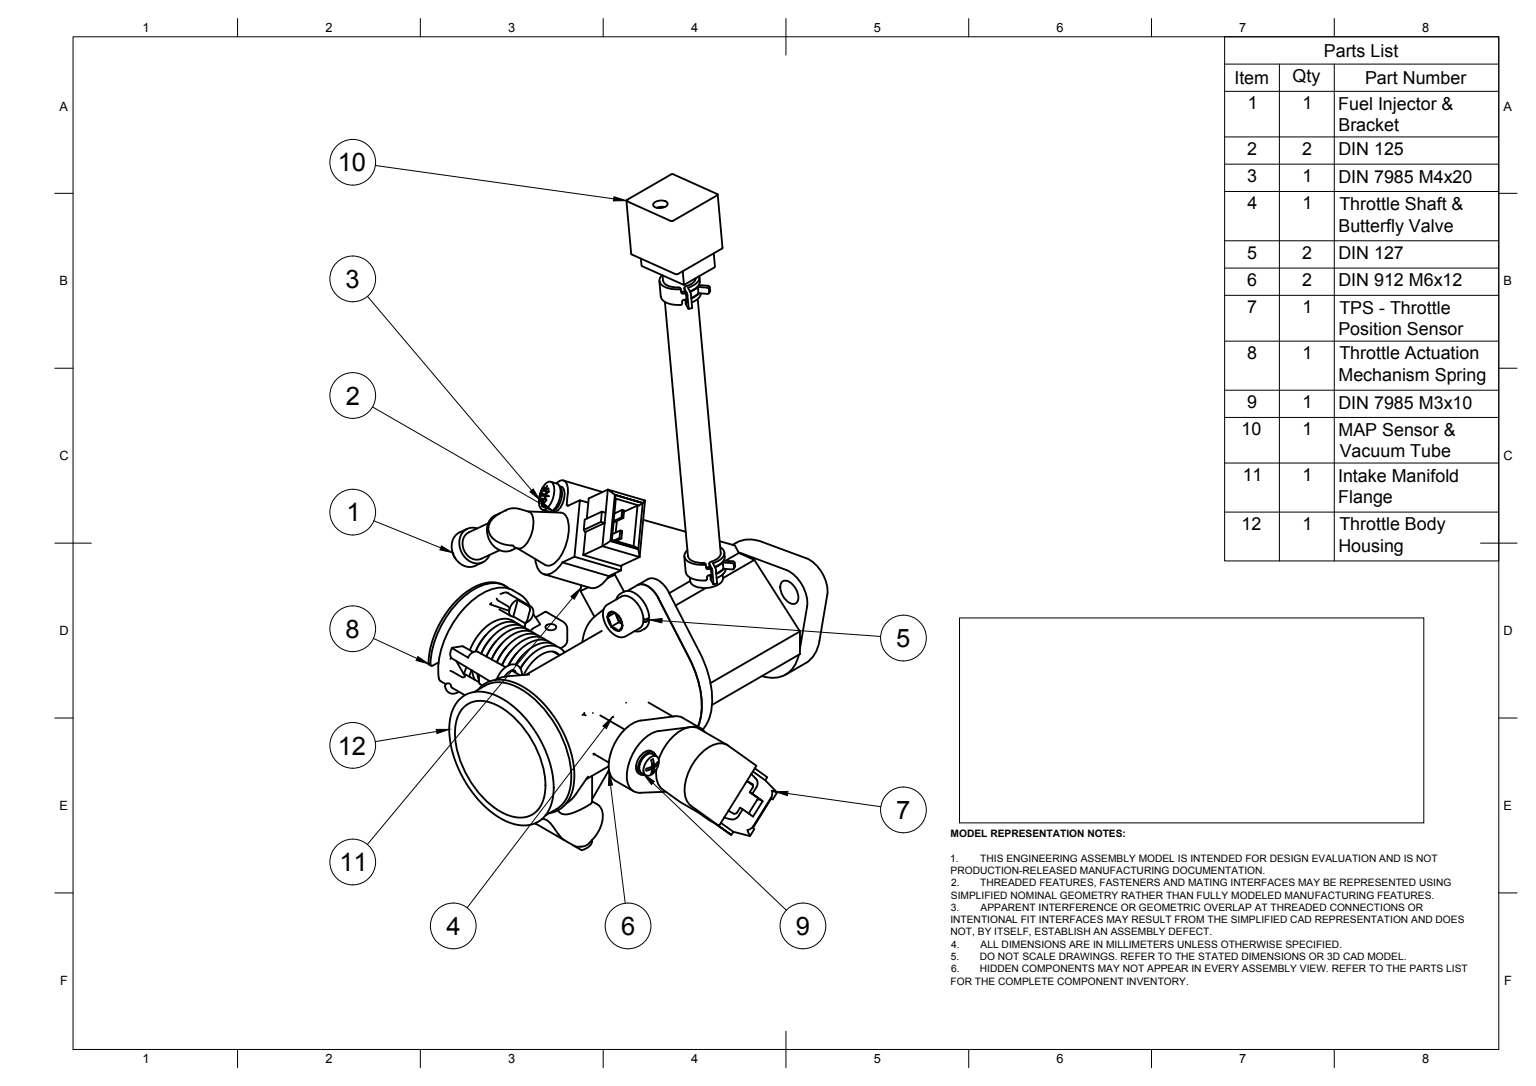
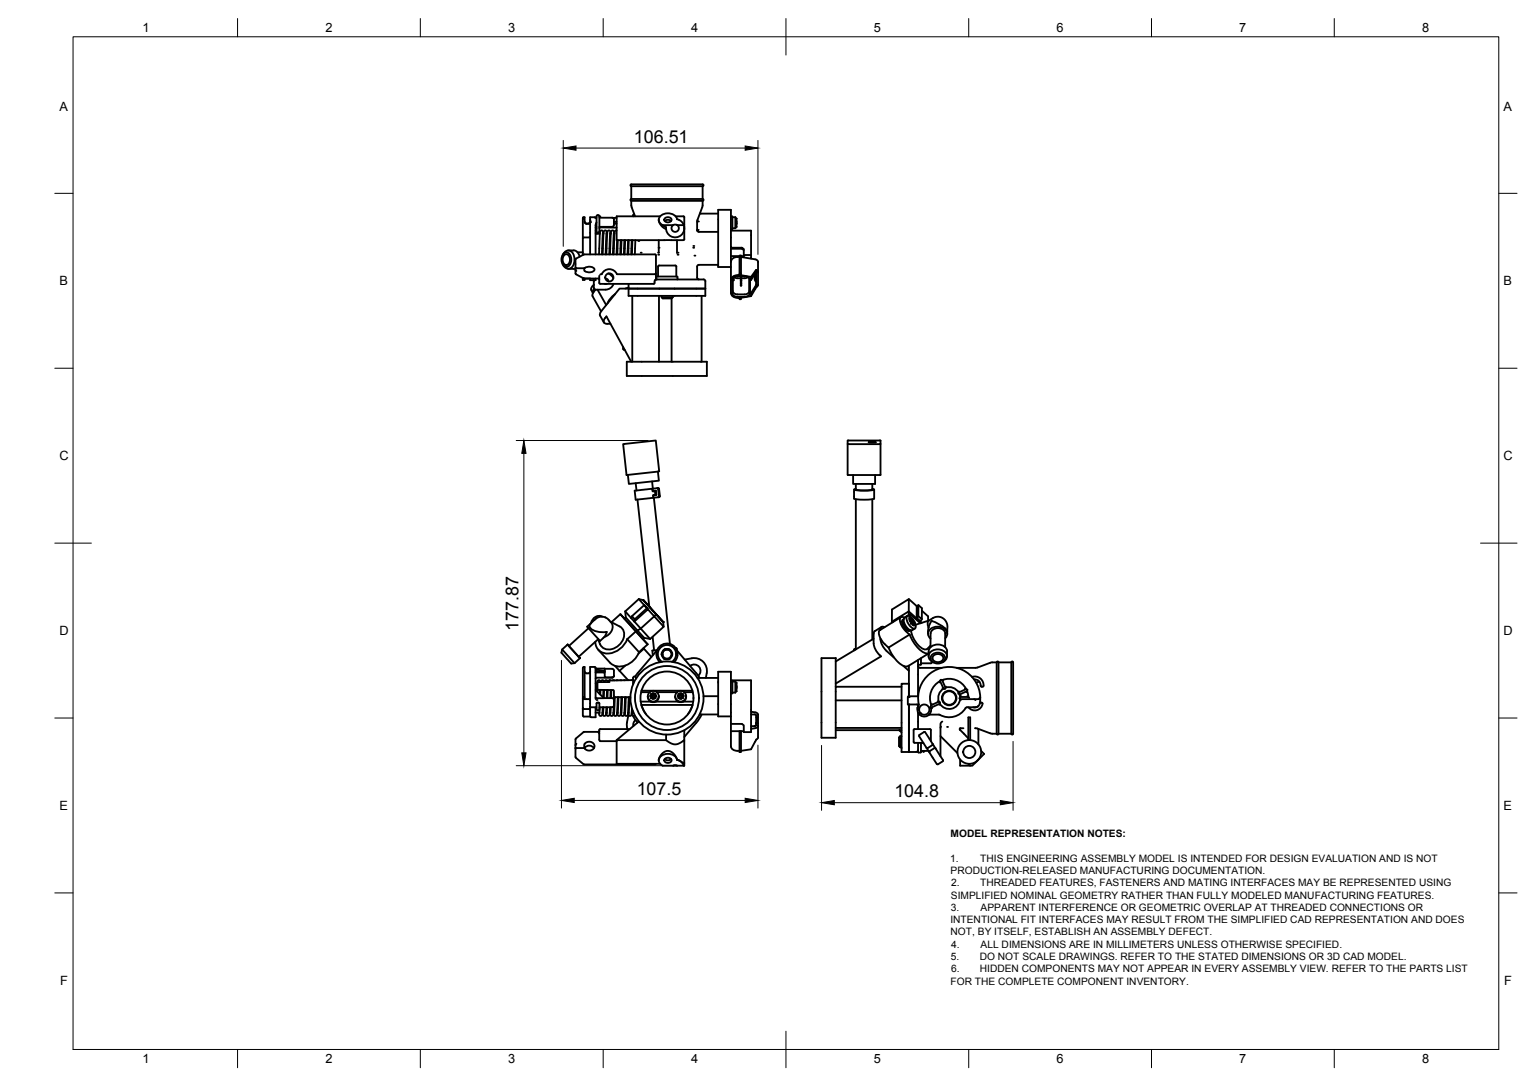
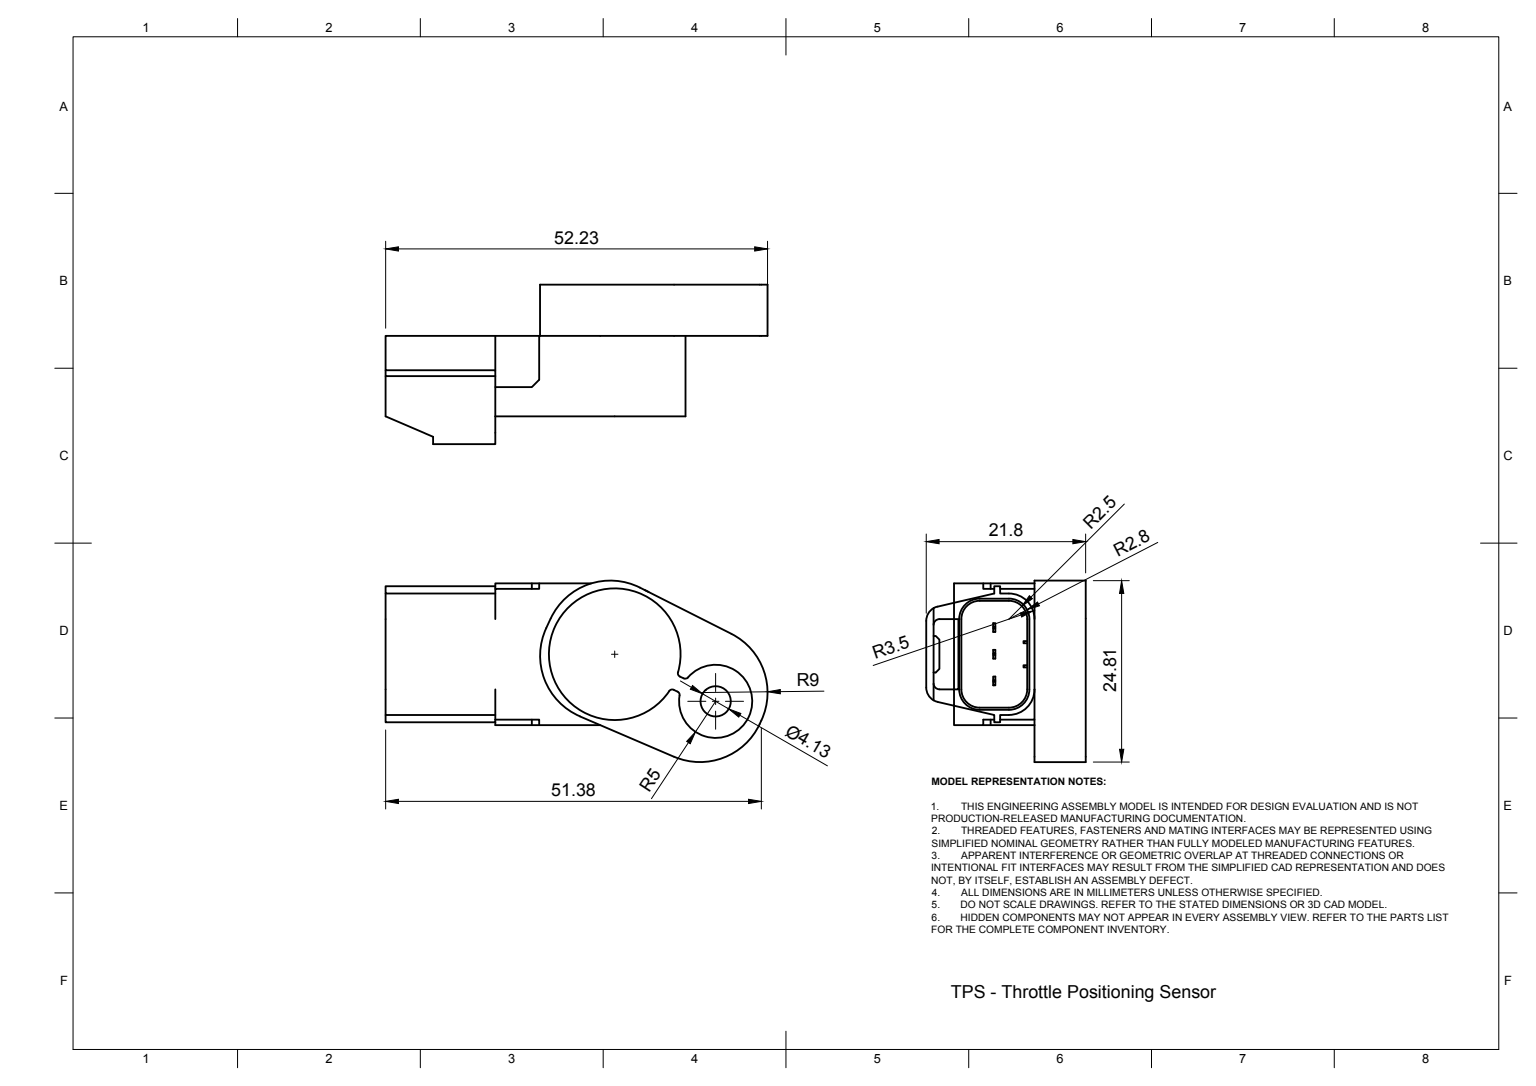
ISO-10303-21;
HEADER;
/* Generated by software containing ST-Developer
 * from STEP Tools, Inc. (www.steptools.com) 
 */

FILE_DESCRIPTION(
/* description */ ('STEP AP214'),
/* implementation_level */ '2;1');

FILE_NAME(
/* name */ 'MAS-617',
/* time_stamp */ '2026-10-07T12:18:07-07:00',
/* author */ (''),
/* organization */ (''),
/* preprocessor_version */ 'ST-DEVELOPER v20.2',
/* originating_system */ 'Autodesk Translation Framework v15.15.0.0',
/* authorisation */ '');

FILE_SCHEMA (('AUTOMOTIVE_DESIGN { 1 0 10303 214 3 1 1 }'));
ENDSEC;

DATA;
#10=MECHANICAL_DESIGN_GEOMETRIC_PRESENTATION_REPRESENTATION('',(#122,#123,
#124,#125,#126,#127,#128,#129,#130,#131,#132,#133),#62974);
#11=ITEM_DEFINED_TRANSFORMATION($,$,#15338,#16941);
#12=ITEM_DEFINED_TRANSFORMATION($,$,#16856,#16942);
#13=ITEM_DEFINED_TRANSFORMATION($,$,#15471,#16943);
#14=ITEM_DEFINED_TRANSFORMATION($,$,#15531,#16944);
#15=ITEM_DEFINED_TRANSFORMATION($,$,#16865,#16945);
#16=ITEM_DEFINED_TRANSFORMATION($,$,#16884,#16946);
#17=ITEM_DEFINED_TRANSFORMATION($,$,#15679,#16947);
#18=ITEM_DEFINED_TRANSFORMATION($,$,#15858,#16948);
#19=ITEM_DEFINED_TRANSFORMATION($,$,#16176,#16949);
#20=ITEM_DEFINED_TRANSFORMATION($,$,#16214,#16950);
#21=ITEM_DEFINED_TRANSFORMATION($,$,#16388,#16951);
#22=ITEM_DEFINED_TRANSFORMATION($,$,#16488,#16952);
#23=ITEM_DEFINED_TRANSFORMATION($,$,#16856,#16953);
#24=ITEM_DEFINED_TRANSFORMATION($,$,#16865,#16954);
#25=ITEM_DEFINED_TRANSFORMATION($,$,#16884,#16955);
#26=(
REPRESENTATION_RELATIONSHIP($,$,#63021,#63020)
REPRESENTATION_RELATIONSHIP_WITH_TRANSFORMATION(#11)
SHAPE_REPRESENTATION_RELATIONSHIP()
);
#27=(
REPRESENTATION_RELATIONSHIP($,$,#63030,#63020)
REPRESENTATION_RELATIONSHIP_WITH_TRANSFORMATION(#12)
SHAPE_REPRESENTATION_RELATIONSHIP()
);
#28=(
REPRESENTATION_RELATIONSHIP($,$,#63022,#63020)
REPRESENTATION_RELATIONSHIP_WITH_TRANSFORMATION(#13)
SHAPE_REPRESENTATION_RELATIONSHIP()
);
#29=(
REPRESENTATION_RELATIONSHIP($,$,#63023,#63020)
REPRESENTATION_RELATIONSHIP_WITH_TRANSFORMATION(#14)
SHAPE_REPRESENTATION_RELATIONSHIP()
);
#30=(
REPRESENTATION_RELATIONSHIP($,$,#63031,#63020)
REPRESENTATION_RELATIONSHIP_WITH_TRANSFORMATION(#15)
SHAPE_REPRESENTATION_RELATIONSHIP()
);
#31=(
REPRESENTATION_RELATIONSHIP($,$,#63032,#63020)
REPRESENTATION_RELATIONSHIP_WITH_TRANSFORMATION(#16)
SHAPE_REPRESENTATION_RELATIONSHIP()
);
#32=(
REPRESENTATION_RELATIONSHIP($,$,#63024,#63020)
REPRESENTATION_RELATIONSHIP_WITH_TRANSFORMATION(#17)
SHAPE_REPRESENTATION_RELATIONSHIP()
);
#33=(
REPRESENTATION_RELATIONSHIP($,$,#63025,#63020)
REPRESENTATION_RELATIONSHIP_WITH_TRANSFORMATION(#18)
SHAPE_REPRESENTATION_RELATIONSHIP()
);
#34=(
REPRESENTATION_RELATIONSHIP($,$,#63026,#63020)
REPRESENTATION_RELATIONSHIP_WITH_TRANSFORMATION(#19)
SHAPE_REPRESENTATION_RELATIONSHIP()
);
#35=(
REPRESENTATION_RELATIONSHIP($,$,#63027,#63020)
REPRESENTATION_RELATIONSHIP_WITH_TRANSFORMATION(#20)
SHAPE_REPRESENTATION_RELATIONSHIP()
);
#36=(
REPRESENTATION_RELATIONSHIP($,$,#63028,#63020)
REPRESENTATION_RELATIONSHIP_WITH_TRANSFORMATION(#21)
SHAPE_REPRESENTATION_RELATIONSHIP()
);
#37=(
REPRESENTATION_RELATIONSHIP($,$,#63029,#63020)
REPRESENTATION_RELATIONSHIP_WITH_TRANSFORMATION(#22)
SHAPE_REPRESENTATION_RELATIONSHIP()
);
#38=(
REPRESENTATION_RELATIONSHIP($,$,#63030,#63020)
REPRESENTATION_RELATIONSHIP_WITH_TRANSFORMATION(#23)
SHAPE_REPRESENTATION_RELATIONSHIP()
);
#39=(
REPRESENTATION_RELATIONSHIP($,$,#63031,#63020)
REPRESENTATION_RELATIONSHIP_WITH_TRANSFORMATION(#24)
SHAPE_REPRESENTATION_RELATIONSHIP()
);
#40=(
REPRESENTATION_RELATIONSHIP($,$,#63032,#63020)
REPRESENTATION_RELATIONSHIP_WITH_TRANSFORMATION(#25)
SHAPE_REPRESENTATION_RELATIONSHIP()
);
#41=CONTEXT_DEPENDENT_SHAPE_REPRESENTATION(#26,#63005);
#42=CONTEXT_DEPENDENT_SHAPE_REPRESENTATION(#27,#63006);
#43=CONTEXT_DEPENDENT_SHAPE_REPRESENTATION(#28,#63007);
#44=CONTEXT_DEPENDENT_SHAPE_REPRESENTATION(#29,#63008);
#45=CONTEXT_DEPENDENT_SHAPE_REPRESENTATION(#30,#63009);
#46=CONTEXT_DEPENDENT_SHAPE_REPRESENTATION(#31,#63010);
#47=CONTEXT_DEPENDENT_SHAPE_REPRESENTATION(#32,#63011);
#48=CONTEXT_DEPENDENT_SHAPE_REPRESENTATION(#33,#63012);
#49=CONTEXT_DEPENDENT_SHAPE_REPRESENTATION(#34,#63013);
#50=CONTEXT_DEPENDENT_SHAPE_REPRESENTATION(#35,#63014);
#51=CONTEXT_DEPENDENT_SHAPE_REPRESENTATION(#36,#63015);
#52=CONTEXT_DEPENDENT_SHAPE_REPRESENTATION(#37,#63016);
#53=CONTEXT_DEPENDENT_SHAPE_REPRESENTATION(#38,#63017);
#54=CONTEXT_DEPENDENT_SHAPE_REPRESENTATION(#39,#63018);
#55=CONTEXT_DEPENDENT_SHAPE_REPRESENTATION(#40,#63019);
#56=NEXT_ASSEMBLY_USAGE_OCCURRENCE('Fuel Injector & Bracket:1',
'Fuel Injector & Bracket:1','Fuel Injector & Bracket:1',#63034,#63035,
'Fuel Injector & Bracket:1');
#57=NEXT_ASSEMBLY_USAGE_OCCURRENCE('DIN 125:1','DIN 125:1','DIN 125:1',
#63034,#63044,'DIN 125:1');
#58=NEXT_ASSEMBLY_USAGE_OCCURRENCE('DIN 7985 M4x20:1',
'DIN 7985 M4x20:1','DIN 7985 M4x20:1',#63034,#63036,'DIN 7985 M4x20:1');
#59=NEXT_ASSEMBLY_USAGE_OCCURRENCE('Throttle Shaft & Butterfly Valve:1',
'Throttle Shaft & Butterfly Valve:1',
'Throttle Shaft & Butterfly Valve:1',#63034,#63037,
'Throttle Shaft & Butterfly Valve:1');
#60=NEXT_ASSEMBLY_USAGE_OCCURRENCE('DIN 127:1','DIN 127:1','DIN 127:1',
#63034,#63045,'DIN 127:1');
#61=NEXT_ASSEMBLY_USAGE_OCCURRENCE('DIN 912 M6x12:1','DIN 912 M6x12:1',
'DIN 912 M6x12:1',#63034,#63046,'DIN 912 M6x12:1');
#62=NEXT_ASSEMBLY_USAGE_OCCURRENCE('TPS - Throttle Position Sensor:1',
'TPS - Throttle Position Sensor:1','TPS - Throttle Position Sensor:1',#63034,
#63038,'TPS - Throttle Position Sensor:1');
#63=NEXT_ASSEMBLY_USAGE_OCCURRENCE(
'Throttle Actuation Mechanism Spring:1',
'Throttle Actuation Mechanism Spring:1',
'Throttle Actuation Mechanism Spring:1',#63034,#63039,
'Throttle Actuation Mechanism Spring:1');
#64=NEXT_ASSEMBLY_USAGE_OCCURRENCE('DIN 7985 M3x10:1',
'DIN 7985 M3x10:1','DIN 7985 M3x10:1',#63034,#63040,'DIN 7985 M3x10:1');
#65=NEXT_ASSEMBLY_USAGE_OCCURRENCE('MAP Sensor & Vacuum Tube:1',
'MAP Sensor & Vacuum Tube:1','MAP Sensor & Vacuum Tube:1',#63034,#63041,
'MAP Sensor & Vacuum Tube:1');
#66=NEXT_ASSEMBLY_USAGE_OCCURRENCE('Intake Manifold Flange:1',
'Intake Manifold Flange:1','Intake Manifold Flange:1',#63034,#63042,
'Intake Manifold Flange:1');
#67=NEXT_ASSEMBLY_USAGE_OCCURRENCE('Throttle Body Housing:1',
'Throttle Body Housing:1','Throttle Body Housing:1',#63034,#63043,
'Throttle Body Housing:1');
#68=NEXT_ASSEMBLY_USAGE_OCCURRENCE('DIN 125:2','DIN 125:2','DIN 125:2',
#63034,#63044,'DIN 125:2');
#69=NEXT_ASSEMBLY_USAGE_OCCURRENCE('DIN 127:2','DIN 127:2','DIN 127:2',
#63034,#63045,'DIN 127:2');
#70=NEXT_ASSEMBLY_USAGE_OCCURRENCE('DIN 912 M6x12:2','DIN 912 M6x12:2',
'DIN 912 M6x12:2',#63034,#63046,'DIN 912 M6x12:2');
#71=(
BOUNDED_CURVE()
B_SPLINE_CURVE(2,(#37611,#37612,#37613,#37614,#37615,#37616,#37617,#37618,
#37619,#37620,#37621,#37622,#37623,#37624,#37625,#37626,#37627,#37628,#37629,
#37630,#37631,#37632,#37633,#37634,#37635,#37636,#37637,#37638,#37639,#37640,
#37641,#37642,#37643,#37644,#37645,#37646,#37647,#37648,#37649,#37650,#37651,
#37652,#37653,#37654,#37655,#37656,#37657,#37658,#37659,#37660,#37661,#37662,
#37663,#37664,#37665,#37666,#37667,#37668,#37669,#37670,#37671,#37672,#37673,
#37674,#37675,#37676,#37677,#37678,#37679,#37680,#37681,#37682,#37683,#37684,
#37685,#37686,#37687,#37688,#37689,#37690,#37691,#37692,#37693,#37694,#37695,
#37696,#37697,#37698,#37699,#37700,#37701,#37702,#37703,#37704,#37705,#37706,
#37707,#37708,#37709,#37710,#37711,#37712,#37713,#37714,#37715,#37716,#37717,
#37718,#37719,#37720,#37721,#37722,#37723,#37724,#37725,#37726,#37727,#37728,
#37729,#37730,#37731),.UNSPECIFIED.,.F.,.F.)
B_SPLINE_CURVE_WITH_KNOTS((3,2,2,2,2,2,2,2,2,2,2,2,2,2,2,2,2,2,2,2,2,2,
2,2,2,2,2,2,2,2,2,2,2,2,2,2,2,2,2,2,2,2,2,2,2,2,2,2,2,2,2,2,2,2,2,2,2,2,
2,2,3),(0.,0.0166666666666666,0.0333333333333333,0.05,0.0666666666666667,
0.0833333333333333,0.1,0.116666666666667,0.133333333333333,0.15,0.166666666666667,
0.183333333333334,0.2,0.216666666666667,0.233333333333334,0.25,0.266666666666667,
0.283333333333334,0.3,0.316666666666666,0.333333333333334,0.35,0.366666666666666,
0.383333333333334,0.4,0.416666666666667,0.433333333333334,0.45,0.466666666666667,
0.483333333333333,0.5,0.516666666666667,0.533333333333333,0.55,0.566666666666667,
0.583333333333333,0.6,0.616666666666667,0.633333333333333,0.65,0.666666666666667,
0.683333333333333,0.7,0.716666666666667,0.733333333333333,0.75,0.766666666666667,
0.783333333333333,0.8,0.816666666666667,0.833333333333333,0.85,0.866666666666667,
0.883333333333333,0.9,0.916666666666667,0.933333333333333,0.95,0.966666666666667,
0.983333333333333,1.),.UNSPECIFIED.)
CURVE()
GEOMETRIC_REPRESENTATION_ITEM()
RATIONAL_B_SPLINE_CURVE((1.,0.866025403784439,1.,0.866025403784439,1.,0.866025403784439,
1.,0.866025403784439,1.,0.866025403784439,1.,0.866025403784439,1.,0.866025403784439,
1.,0.866025403784439,1.,0.866025403784439,1.,0.866025403784439,1.,0.866025403784439,
1.,0.866025403784439,1.,0.866025403784439,1.,0.866025403784439,1.,0.866025403784439,
1.,0.866025403784439,1.,0.866025403784439,1.,0.866025403784439,1.,0.866025403784439,
1.,0.866025403784439,1.,0.866025403784439,1.,0.866025403784439,1.,0.866025403784439,
1.,0.866025403784439,1.,0.866025403784439,1.,0.866025403784439,1.,0.866025403784439,
1.,0.866025403784439,1.,0.866025403784439,1.,0.866025403784439,1.,0.866025403784439,
1.,0.866025403784439,1.,0.866025403784439,1.,0.866025403784439,1.,0.866025403784439,
1.,0.866025403784439,1.,0.866025403784439,1.,0.866025403784439,1.,0.866025403784439,
1.,0.866025403784439,1.,0.866025403784439,1.,0.866025403784439,1.,0.866025403784439,
1.,0.866025403784439,1.,0.866025403784439,1.,0.866025403784439,1.,0.866025403784439,
1.,0.866025403784439,1.,0.866025403784439,1.,0.866025403784439,1.,0.866025403784439,
1.,0.866025403784439,1.,0.866025403784439,1.,0.866025403784439,1.,0.866025403784439,
1.,0.866025403784439,1.,0.866025403784439,1.,0.866025403784439,1.,0.866025403784439,
1.,0.866025403784439,1.))
REPRESENTATION_ITEM('')
);
#72=(
BOUNDED_CURVE()
B_SPLINE_CURVE(2,(#37732,#37733,#37734,#37735,#37736,#37737,#37738,#37739,
#37740,#37741,#37742,#37743,#37744,#37745,#37746,#37747,#37748,#37749,#37750,
#37751,#37752,#37753,#37754,#37755,#37756,#37757,#37758,#37759,#37760,#37761,
#37762,#37763,#37764,#37765,#37766,#37767,#37768,#37769,#37770,#37771,#37772,
#37773,#37774,#37775,#37776,#37777,#37778,#37779,#37780,#37781,#37782,#37783,
#37784,#37785,#37786,#37787,#37788,#37789,#37790,#37791,#37792,#37793,#37794,
#37795,#37796,#37797,#37798,#37799,#37800,#37801,#37802,#37803,#37804,#37805,
#37806,#37807,#37808,#37809,#37810,#37811,#37812,#37813,#37814,#37815,#37816,
#37817,#37818,#37819,#37820,#37821,#37822,#37823,#37824,#37825,#37826,#37827,
#37828,#37829,#37830,#37831,#37832,#37833,#37834,#37835,#37836,#37837,#37838,
#37839,#37840,#37841,#37842,#37843,#37844,#37845,#37846,#37847,#37848,#37849,
#37850,#37851,#37852),.UNSPECIFIED.,.F.,.F.)
B_SPLINE_CURVE_WITH_KNOTS((3,2,2,2,2,2,2,2,2,2,2,2,2,2,2,2,2,2,2,2,2,2,
2,2,2,2,2,2,2,2,2,2,2,2,2,2,2,2,2,2,2,2,2,2,2,2,2,2,2,2,2,2,2,2,2,2,2,2,
2,2,3),(0.,0.0166666666666666,0.0333333333333333,0.05,0.0666666666666667,
0.0833333333333333,0.1,0.116666666666667,0.133333333333333,0.15,0.166666666666667,
0.183333333333334,0.2,0.216666666666667,0.233333333333334,0.25,0.266666666666667,
0.283333333333334,0.3,0.316666666666666,0.333333333333334,0.35,0.366666666666666,
0.383333333333334,0.4,0.416666666666667,0.433333333333334,0.45,0.466666666666667,
0.483333333333333,0.5,0.516666666666667,0.533333333333333,0.55,0.566666666666667,
0.583333333333333,0.6,0.616666666666667,0.633333333333333,0.65,0.666666666666667,
0.683333333333333,0.7,0.716666666666667,0.733333333333333,0.75,0.766666666666667,
0.783333333333333,0.8,0.816666666666667,0.833333333333333,0.85,0.866666666666667,
0.883333333333333,0.9,0.916666666666667,0.933333333333333,0.95,0.966666666666667,
0.983333333333333,1.),.UNSPECIFIED.)
CURVE()
GEOMETRIC_REPRESENTATION_ITEM()
RATIONAL_B_SPLINE_CURVE((1.,0.866025403784439,1.,0.866025403784439,1.,0.866025403784439,
1.,0.866025403784439,1.,0.866025403784439,1.,0.866025403784439,1.,0.866025403784439,
1.,0.866025403784439,1.,0.866025403784439,1.,0.866025403784439,1.,0.866025403784439,
1.,0.866025403784439,1.,0.866025403784439,1.,0.866025403784439,1.,0.866025403784439,
1.,0.866025403784439,1.,0.866025403784439,1.,0.866025403784439,1.,0.866025403784439,
1.,0.866025403784439,1.,0.866025403784439,1.,0.866025403784439,1.,0.866025403784439,
1.,0.866025403784439,1.,0.866025403784439,1.,0.866025403784439,1.,0.866025403784439,
1.,0.866025403784439,1.,0.866025403784439,1.,0.866025403784439,1.,0.866025403784439,
1.,0.866025403784439,1.,0.866025403784439,1.,0.866025403784439,1.,0.866025403784439,
1.,0.866025403784439,1.,0.866025403784439,1.,0.866025403784439,1.,0.866025403784439,
1.,0.866025403784439,1.,0.866025403784439,1.,0.866025403784439,1.,0.866025403784439,
1.,0.866025403784439,1.,0.866025403784439,1.,0.866025403784439,1.,0.866025403784439,
1.,0.866025403784439,1.,0.866025403784439,1.,0.866025403784439,1.,0.866025403784439,
1.,0.866025403784439,1.,0.866025403784439,1.,0.866025403784439,1.,0.866025403784439,
1.,0.866025403784439,1.,0.866025403784439,1.,0.866025403784439,1.,0.866025403784439,
1.,0.866025403784439,1.))
REPRESENTATION_ITEM('')
);
#73=(
BOUNDED_CURVE()
B_SPLINE_CURVE(2,(#62798,#62799,#62800),.UNSPECIFIED.,.F.,.F.)
B_SPLINE_CURVE_WITH_KNOTS((3,3),(-0.604448710450841,-0.208150383555822),
 .UNSPECIFIED.)
CURVE()
GEOMETRIC_REPRESENTATION_ITEM()
RATIONAL_B_SPLINE_CURVE((1.32194252928783,1.52287779373958,1.32194252928783))
REPRESENTATION_ITEM('')
);
#74=(
BOUNDED_CURVE()
B_SPLINE_CURVE(2,(#62844,#62845,#62846),.UNSPECIFIED.,.F.,.F.)
B_SPLINE_CURVE_WITH_KNOTS((3,3),(0.208150383555825,0.60444871045084),
 .UNSPECIFIED.)
CURVE()
GEOMETRIC_REPRESENTATION_ITEM()
RATIONAL_B_SPLINE_CURVE((1.32194252928783,1.52287779373957,1.32194252928783))
REPRESENTATION_ITEM('')
);
#75=(
BOUNDED_CURVE()
B_SPLINE_CURVE(2,(#62851,#62852,#62853),.UNSPECIFIED.,.F.,.F.)
B_SPLINE_CURVE_WITH_KNOTS((3,3),(0.208150383555826,0.604448710450838),
 .UNSPECIFIED.)
CURVE()
GEOMETRIC_REPRESENTATION_ITEM()
RATIONAL_B_SPLINE_CURVE((1.32194252928783,1.52287779373957,1.32194252928783))
REPRESENTATION_ITEM('')
);
#76=(
BOUNDED_CURVE()
B_SPLINE_CURVE(2,(#62858,#62859,#62860),.UNSPECIFIED.,.F.,.F.)
B_SPLINE_CURVE_WITH_KNOTS((3,3),(0.208150383555825,0.60444871045084),
 .UNSPECIFIED.)
CURVE()
GEOMETRIC_REPRESENTATION_ITEM()
RATIONAL_B_SPLINE_CURVE((1.32194252928783,1.52287779373957,1.32194252928783))
REPRESENTATION_ITEM('')
);
#77=(
BOUNDED_CURVE()
B_SPLINE_CURVE(2,(#62869,#62870,#62871),.UNSPECIFIED.,.F.,.F.)
B_SPLINE_CURVE_WITH_KNOTS((3,3),(0.208150383555823,0.604448710450839),
 .UNSPECIFIED.)
CURVE()
GEOMETRIC_REPRESENTATION_ITEM()
RATIONAL_B_SPLINE_CURVE((1.32194252928783,1.52287779373958,1.32194252928783))
REPRESENTATION_ITEM('')
);
#78=(
BOUNDED_CURVE()
B_SPLINE_CURVE(2,(#62876,#62877,#62878),.UNSPECIFIED.,.F.,.F.)
B_SPLINE_CURVE_WITH_KNOTS((3,3),(0.208150383555823,0.604448710450836),
 .UNSPECIFIED.)
CURVE()
GEOMETRIC_REPRESENTATION_ITEM()
RATIONAL_B_SPLINE_CURVE((1.32194252928783,1.52287779373958,1.32194252928783))
REPRESENTATION_ITEM('')
);
#79=SPHERICAL_SURFACE('',#15475,8.00000000000091);
#80=SPHERICAL_SURFACE('',#15545,6.);
#81=SPHERICAL_SURFACE('',#15579,6.);
#82=SPHERICAL_SURFACE('',#16177,6.);
#83=SPHERICAL_SURFACE('',#16593,0.5);
#84=SPHERICAL_SURFACE('',#16603,0.5);
#85=SPHERICAL_SURFACE('',#16608,0.5);
#86=SPHERICAL_SURFACE('',#16674,0.5);
#87=SPHERICAL_SURFACE('',#16680,0.5);
#88=SPHERICAL_SURFACE('',#16687,0.5);
#89=SPHERICAL_SURFACE('',#16695,0.5);
#90=SPHERICAL_SURFACE('',#16702,0.5);
#91=SPHERICAL_SURFACE('',#16709,0.5);
#92=SPHERICAL_SURFACE('',#16717,0.5);
#93=SPHERICAL_SURFACE('',#16725,0.5);
#94=SPHERICAL_SURFACE('',#16730,0.5);
#95=SPHERICAL_SURFACE('',#16733,0.5);
#96=SPHERICAL_SURFACE('',#16778,0.5);
#97=SPHERICAL_SURFACE('',#16816,1.);
#98=SHAPE_REPRESENTATION_RELATIONSHIP('SRR','None',#63021,#110);
#99=SHAPE_REPRESENTATION_RELATIONSHIP('SRR','None',#63022,#111);
#100=SHAPE_REPRESENTATION_RELATIONSHIP('SRR','None',#63023,#112);
#101=SHAPE_REPRESENTATION_RELATIONSHIP('SRR','None',#63024,#113);
#102=SHAPE_REPRESENTATION_RELATIONSHIP('SRR','None',#63025,#114);
#103=SHAPE_REPRESENTATION_RELATIONSHIP('SRR','None',#63026,#115);
#104=SHAPE_REPRESENTATION_RELATIONSHIP('SRR','None',#63027,#116);
#105=SHAPE_REPRESENTATION_RELATIONSHIP('SRR','None',#63028,#117);
#106=SHAPE_REPRESENTATION_RELATIONSHIP('SRR','None',#63029,#118);
#107=SHAPE_REPRESENTATION_RELATIONSHIP('SRR','None',#63030,#119);
#108=SHAPE_REPRESENTATION_RELATIONSHIP('SRR','None',#63031,#120);
#109=SHAPE_REPRESENTATION_RELATIONSHIP('SRR','None',#63032,#121);
#110=ADVANCED_BREP_SHAPE_REPRESENTATION('',(#134),#62962);
#111=ADVANCED_BREP_SHAPE_REPRESENTATION('',(#135),#62963);
#112=ADVANCED_BREP_SHAPE_REPRESENTATION('',(#136),#62964);
#113=ADVANCED_BREP_SHAPE_REPRESENTATION('',(#137),#62965);
#114=ADVANCED_BREP_SHAPE_REPRESENTATION('',(#138),#62966);
#115=ADVANCED_BREP_SHAPE_REPRESENTATION('',(#139),#62967);
#116=ADVANCED_BREP_SHAPE_REPRESENTATION('',(#140),#62968);
#117=ADVANCED_BREP_SHAPE_REPRESENTATION('',(#141),#62969);
#118=ADVANCED_BREP_SHAPE_REPRESENTATION('',(#142),#62970);
#119=ADVANCED_BREP_SHAPE_REPRESENTATION('',(#143),#62971);
#120=ADVANCED_BREP_SHAPE_REPRESENTATION('',(#144),#62972);
#121=ADVANCED_BREP_SHAPE_REPRESENTATION('',(#145),#62973);
#122=STYLED_ITEM('',(#63090),#134);
#123=STYLED_ITEM('',(#63090),#135);
#124=STYLED_ITEM('',(#63090),#136);
#125=STYLED_ITEM('',(#63090),#137);
#126=STYLED_ITEM('',(#63090),#138);
#127=STYLED_ITEM('',(#63090),#139);
#128=STYLED_ITEM('',(#63090),#140);
#129=STYLED_ITEM('',(#63090),#141);
#130=STYLED_ITEM('',(#63090),#142);
#131=STYLED_ITEM('',(#63090),#143);
#132=STYLED_ITEM('',(#63090),#144);
#133=STYLED_ITEM('',(#63090),#145);
#134=MANIFOLD_SOLID_BREP('Body1',#15192);
#135=MANIFOLD_SOLID_BREP('Body1',#15193);
#136=MANIFOLD_SOLID_BREP('Body1',#15194);
#137=MANIFOLD_SOLID_BREP('Body1',#15195);
#138=MANIFOLD_SOLID_BREP('Body1',#15196);
#139=MANIFOLD_SOLID_BREP('Body1',#15197);
#140=MANIFOLD_SOLID_BREP('Body1',#15198);
#141=MANIFOLD_SOLID_BREP('Body1',#15199);
#142=MANIFOLD_SOLID_BREP('Body1',#15200);
#143=MANIFOLD_SOLID_BREP('Body1',#15201);
#144=MANIFOLD_SOLID_BREP('Body1',#15202);
#145=MANIFOLD_SOLID_BREP('Body1',#15203);
#146=(
BOUNDED_SURFACE()
B_SPLINE_SURFACE(2,2,((#27768,#27769,#27770,#27771,#27772,#27773,#27774),
(#27775,#27776,#27777,#27778,#27779,#27780,#27781),(#27782,#27783,#27784,
#27785,#27786,#27787,#27788)),.UNSPECIFIED.,.F.,.F.,.F.)
B_SPLINE_SURFACE_WITH_KNOTS((3,3),(3,2,2,3),(-1.57079632681342,3.50763862399952E-12),
(-1.6184333897888,-0.539477796596266,0.539477796596266,1.6184333897888),
 .UNSPECIFIED.)
GEOMETRIC_REPRESENTATION_ITEM()
RATIONAL_B_SPLINE_SURFACE(((1.,0.857977047969415,1.,0.857977047969415,1.,
0.857977047969415,1.),(0.707106781178761,0.606681388714908,0.707106781178761,
0.606681388714908,0.707106781178761,0.606681388714908,0.707106781178761),
(1.,0.857977047969415,1.,0.857977047969415,1.,0.857977047969415,1.)))
REPRESENTATION_ITEM('')
SURFACE()
);
#147=(
BOUNDED_SURFACE()
B_SPLINE_SURFACE(3,1,((#34070,#34071),(#34072,#34073),(#34074,#34075),(#34076,
#34077)),.UNSPECIFIED.,.F.,.F.,.F.)
B_SPLINE_SURFACE_WITH_KNOTS((4,4),(2,2),(0.,1.),(0.,0.12),.UNSPECIFIED.)
GEOMETRIC_REPRESENTATION_ITEM()
RATIONAL_B_SPLINE_SURFACE(((1.,1.),(0.333333333333333,0.333333333333333),
(0.333333333333333,0.333333333333333),(1.,1.)))
REPRESENTATION_ITEM('')
SURFACE()
);
#148=(
BOUNDED_SURFACE()
B_SPLINE_SURFACE(3,1,((#34465,#34466),(#34467,#34468),(#34469,#34470),(#34471,
#34472)),.UNSPECIFIED.,.F.,.F.,.F.)
B_SPLINE_SURFACE_WITH_KNOTS((4,4),(2,2),(0.,1.),(0.,0.120000000000004),
 .UNSPECIFIED.)
GEOMETRIC_REPRESENTATION_ITEM()
RATIONAL_B_SPLINE_SURFACE(((1.,1.),(0.333333333333333,0.333333333333333),
(0.333333333333333,0.333333333333333),(1.,1.)))
REPRESENTATION_ITEM('')
SURFACE()
);
#149=(
BOUNDED_SURFACE()
B_SPLINE_SURFACE(3,2,((#36764,#36765,#36766,#36767,#36768,#36769,#36770,
#36771,#36772,#36773,#36774,#36775,#36776,#36777,#36778,#36779,#36780,#36781,
#36782,#36783,#36784,#36785,#36786,#36787,#36788,#36789,#36790,#36791,#36792,
#36793,#36794,#36795,#36796,#36797,#36798,#36799,#36800,#36801,#36802,#36803,
#36804,#36805,#36806,#36807,#36808,#36809,#36810,#36811,#36812,#36813,#36814,
#36815,#36816,#36817,#36818,#36819,#36820,#36821,#36822,#36823,#36824,#36825,
#36826,#36827,#36828,#36829,#36830,#36831,#36832,#36833,#36834,#36835,#36836,
#36837,#36838,#36839,#36840,#36841,#36842,#36843,#36844,#36845,#36846,#36847,
#36848,#36849,#36850,#36851,#36852,#36853,#36854,#36855,#36856,#36857,#36858,
#36859,#36860,#36861,#36862,#36863,#36864,#36865,#36866,#36867,#36868,#36869,
#36870,#36871,#36872,#36873,#36874,#36875,#36876,#36877,#36878,#36879,#36880,
#36881,#36882,#36883,#36884),(#36885,#36886,#36887,#36888,#36889,#36890,
#36891,#36892,#36893,#36894,#36895,#36896,#36897,#36898,#36899,#36900,#36901,
#36902,#36903,#36904,#36905,#36906,#36907,#36908,#36909,#36910,#36911,#36912,
#36913,#36914,#36915,#36916,#36917,#36918,#36919,#36920,#36921,#36922,#36923,
#36924,#36925,#36926,#36927,#36928,#36929,#36930,#36931,#36932,#36933,#36934,
#36935,#36936,#36937,#36938,#36939,#36940,#36941,#36942,#36943,#36944,#36945,
#36946,#36947,#36948,#36949,#36950,#36951,#36952,#36953,#36954,#36955,#36956,
#36957,#36958,#36959,#36960,#36961,#36962,#36963,#36964,#36965,#36966,#36967,
#36968,#36969,#36970,#36971,#36972,#36973,#36974,#36975,#36976,#36977,#36978,
#36979,#36980,#36981,#36982,#36983,#36984,#36985,#36986,#36987,#36988,#36989,
#36990,#36991,#36992,#36993,#36994,#36995,#36996,#36997,#36998,#36999,#37000,
#37001,#37002,#37003,#37004,#37005),(#37006,#37007,#37008,#37009,#37010,
#37011,#37012,#37013,#37014,#37015,#37016,#37017,#37018,#37019,#37020,#37021,
#37022,#37023,#37024,#37025,#37026,#37027,#37028,#37029,#37030,#37031,#37032,
#37033,#37034,#37035,#37036,#37037,#37038,#37039,#37040,#37041,#37042,#37043,
#37044,#37045,#37046,#37047,#37048,#37049,#37050,#37051,#37052,#37053,#37054,
#37055,#37056,#37057,#37058,#37059,#37060,#37061,#37062,#37063,#37064,#37065,
#37066,#37067,#37068,#37069,#37070,#37071,#37072,#37073,#37074,#37075,#37076,
#37077,#37078,#37079,#37080,#37081,#37082,#37083,#37084,#37085,#37086,#37087,
#37088,#37089,#37090,#37091,#37092,#37093,#37094,#37095,#37096,#37097,#37098,
#37099,#37100,#37101,#37102,#37103,#37104,#37105,#37106,#37107,#37108,#37109,
#37110,#37111,#37112,#37113,#37114,#37115,#37116,#37117,#37118,#37119,#37120,
#37121,#37122,#37123,#37124,#37125,#37126),(#37127,#37128,#37129,#37130,
#37131,#37132,#37133,#37134,#37135,#37136,#37137,#37138,#37139,#37140,#37141,
#37142,#37143,#37144,#37145,#37146,#37147,#37148,#37149,#37150,#37151,#37152,
#37153,#37154,#37155,#37156,#37157,#37158,#37159,#37160,#37161,#37162,#37163,
#37164,#37165,#37166,#37167,#37168,#37169,#37170,#37171,#37172,#37173,#37174,
#37175,#37176,#37177,#37178,#37179,#37180,#37181,#37182,#37183,#37184,#37185,
#37186,#37187,#37188,#37189,#37190,#37191,#37192,#37193,#37194,#37195,#37196,
#37197,#37198,#37199,#37200,#37201,#37202,#37203,#37204,#37205,#37206,#37207,
#37208,#37209,#37210,#37211,#37212,#37213,#37214,#37215,#37216,#37217,#37218,
#37219,#37220,#37221,#37222,#37223,#37224,#37225,#37226,#37227,#37228,#37229,
#37230,#37231,#37232,#37233,#37234,#37235,#37236,#37237,#37238,#37239,#37240,
#37241,#37242,#37243,#37244,#37245,#37246,#37247),(#37248,#37249,#37250,
#37251,#37252,#37253,#37254,#37255,#37256,#37257,#37258,#37259,#37260,#37261,
#37262,#37263,#37264,#37265,#37266,#37267,#37268,#37269,#37270,#37271,#37272,
#37273,#37274,#37275,#37276,#37277,#37278,#37279,#37280,#37281,#37282,#37283,
#37284,#37285,#37286,#37287,#37288,#37289,#37290,#37291,#37292,#37293,#37294,
#37295,#37296,#37297,#37298,#37299,#37300,#37301,#37302,#37303,#37304,#37305,
#37306,#37307,#37308,#37309,#37310,#37311,#37312,#37313,#37314,#37315,#37316,
#37317,#37318,#37319,#37320,#37321,#37322,#37323,#37324,#37325,#37326,#37327,
#37328,#37329,#37330,#37331,#37332,#37333,#37334,#37335,#37336,#37337,#37338,
#37339,#37340,#37341,#37342,#37343,#37344,#37345,#37346,#37347,#37348,#37349,
#37350,#37351,#37352,#37353,#37354,#37355,#37356,#37357,#37358,#37359,#37360,
#37361,#37362,#37363,#37364,#37365,#37366,#37367,#37368),(#37369,#37370,
#37371,#37372,#37373,#37374,#37375,#37376,#37377,#37378,#37379,#37380,#37381,
#37382,#37383,#37384,#37385,#37386,#37387,#37388,#37389,#37390,#37391,#37392,
#37393,#37394,#37395,#37396,#37397,#37398,#37399,#37400,#37401,#37402,#37403,
#37404,#37405,#37406,#37407,#37408,#37409,#37410,#37411,#37412,#37413,#37414,
#37415,#37416,#37417,#37418,#37419,#37420,#37421,#37422,#37423,#37424,#37425,
#37426,#37427,#37428,#37429,#37430,#37431,#37432,#37433,#37434,#37435,#37436,
#37437,#37438,#37439,#37440,#37441,#37442,#37443,#37444,#37445,#37446,#37447,
#37448,#37449,#37450,#37451,#37452,#37453,#37454,#37455,#37456,#37457,#37458,
#37459,#37460,#37461,#37462,#37463,#37464,#37465,#37466,#37467,#37468,#37469,
#37470,#37471,#37472,#37473,#37474,#37475,#37476,#37477,#37478,#37479,#37480,
#37481,#37482,#37483,#37484,#37485,#37486,#37487,#37488,#37489),(#37490,
#37491,#37492,#37493,#37494,#37495,#37496,#37497,#37498,#37499,#37500,#37501,
#37502,#37503,#37504,#37505,#37506,#37507,#37508,#37509,#37510,#37511,#37512,
#37513,#37514,#37515,#37516,#37517,#37518,#37519,#37520,#37521,#37522,#37523,
#37524,#37525,#37526,#37527,#37528,#37529,#37530,#37531,#37532,#37533,#37534,
#37535,#37536,#37537,#37538,#37539,#37540,#37541,#37542,#37543,#37544,#37545,
#37546,#37547,#37548,#37549,#37550,#37551,#37552,#37553,#37554,#37555,#37556,
#37557,#37558,#37559,#37560,#37561,#37562,#37563,#37564,#37565,#37566,#37567,
#37568,#37569,#37570,#37571,#37572,#37573,#37574,#37575,#37576,#37577,#37578,
#37579,#37580,#37581,#37582,#37583,#37584,#37585,#37586,#37587,#37588,#37589,
#37590,#37591,#37592,#37593,#37594,#37595,#37596,#37597,#37598,#37599,#37600,
#37601,#37602,#37603,#37604,#37605,#37606,#37607,#37608,#37609,#37610)),
 .UNSPECIFIED.,.T.,.F.,.F.)
B_SPLINE_SURFACE_WITH_KNOTS((4,3,4),(3,2,2,2,2,2,2,2,2,2,2,2,2,2,2,2,2,
2,2,2,2,2,2,2,2,2,2,2,2,2,2,2,2,2,2,2,2,2,2,2,2,2,2,2,2,2,2,2,2,2,2,2,2,
2,2,2,2,2,2,2,3),(0.,0.5,1.),(0.,0.0166666666666666,0.0333333333333333,
0.05,0.0666666666666667,0.0833333333333333,0.1,0.116666666666667,0.133333333333333,
0.15,0.166666666666667,0.183333333333334,0.2,0.216666666666667,0.233333333333334,
0.25,0.266666666666667,0.283333333333334,0.3,0.316666666666666,0.333333333333334,
0.35,0.366666666666666,0.383333333333334,0.4,0.416666666666667,0.433333333333334,
0.45,0.466666666666667,0.483333333333333,0.5,0.516666666666667,0.533333333333333,
0.55,0.566666666666667,0.583333333333333,0.6,0.616666666666667,0.633333333333333,
0.65,0.666666666666667,0.683333333333333,0.7,0.716666666666667,0.733333333333333,
0.75,0.766666666666667,0.783333333333333,0.8,0.816666666666667,0.833333333333333,
0.85,0.866666666666667,0.883333333333333,0.9,0.916666666666667,0.933333333333333,
0.95,0.966666666666667,0.983333333333333,1.),.UNSPECIFIED.)
GEOMETRIC_REPRESENTATION_ITEM()
RATIONAL_B_SPLINE_SURFACE(((1.,0.866025403784439,1.,0.866025403784439,1.,
0.866025403784439,1.,0.866025403784439,1.,0.866025403784439,1.,0.866025403784439,
1.,0.866025403784439,1.,0.866025403784439,1.,0.866025403784439,1.,0.866025403784439,
1.,0.866025403784439,1.,0.866025403784439,1.,0.866025403784439,1.,0.866025403784439,
1.,0.866025403784439,1.,0.866025403784439,1.,0.866025403784439,1.,0.866025403784439,
1.,0.866025403784439,1.,0.866025403784439,1.,0.866025403784439,1.,0.866025403784439,
1.,0.866025403784439,1.,0.866025403784439,1.,0.866025403784439,1.,0.866025403784439,
1.,0.866025403784439,1.,0.866025403784439,1.,0.866025403784439,1.,0.866025403784439,
1.,0.866025403784439,1.,0.866025403784439,1.,0.866025403784439,1.,0.866025403784439,
1.,0.866025403784439,1.,0.866025403784439,1.,0.866025403784439,1.,0.866025403784439,
1.,0.866025403784439,1.,0.866025403784439,1.,0.866025403784439,1.,0.866025403784439,
1.,0.866025403784439,1.,0.866025403784439,1.,0.866025403784439,1.,0.866025403784439,
1.,0.866025403784439,1.,0.866025403784439,1.,0.866025403784439,1.,0.866025403784439,
1.,0.866025403784439,1.,0.866025403784439,1.,0.866025403784439,1.,0.866025403784439,
1.,0.866025403784439,1.,0.866025403784439,1.,0.866025403784439,1.,0.866025403784439,
1.,0.866025403784439,1.,0.866025403784439,1.),(0.333333333333334,0.288675134594813,
0.333333333333334,0.288675134594813,0.333333333333334,0.288675134594813,
0.333333333333334,0.288675134594813,0.333333333333334,0.288675134594813,
0.333333333333334,0.288675134594813,0.333333333333334,0.288675134594813,
0.333333333333334,0.288675134594813,0.333333333333334,0.288675134594813,
0.333333333333334,0.288675134594813,0.333333333333334,0.288675134594813,
0.333333333333334,0.288675134594813,0.333333333333334,0.288675134594813,
0.333333333333334,0.288675134594813,0.333333333333334,0.288675134594813,
0.333333333333334,0.288675134594813,0.333333333333334,0.288675134594813,
0.333333333333334,0.288675134594813,0.333333333333334,0.288675134594813,
0.333333333333334,0.288675134594813,0.333333333333334,0.288675134594813,
0.333333333333334,0.288675134594813,0.333333333333334,0.288675134594813,
0.333333333333334,0.288675134594813,0.333333333333334,0.288675134594813,
0.333333333333334,0.288675134594813,0.333333333333334,0.288675134594813,
0.333333333333334,0.288675134594813,0.333333333333334,0.288675134594813,
0.333333333333334,0.288675134594813,0.333333333333334,0.288675134594813,
0.333333333333334,0.288675134594813,0.333333333333334,0.288675134594813,
0.333333333333334,0.288675134594813,0.333333333333334,0.288675134594813,
0.333333333333334,0.288675134594813,0.333333333333334,0.288675134594813,
0.333333333333334,0.288675134594813,0.333333333333334,0.288675134594813,
0.333333333333334,0.288675134594813,0.333333333333334,0.288675134594813,
0.333333333333334,0.288675134594813,0.333333333333334,0.288675134594813,
0.333333333333334,0.288675134594813,0.333333333333334,0.288675134594813,
0.333333333333334,0.288675134594813,0.333333333333334,0.288675134594813,
0.333333333333334,0.288675134594813,0.333333333333334,0.288675134594813,
0.333333333333334,0.288675134594813,0.333333333333334,0.288675134594813,
0.333333333333334,0.288675134594813,0.333333333333334,0.288675134594813,
0.333333333333334,0.288675134594813,0.333333333333334,0.288675134594813,
0.333333333333334,0.288675134594813,0.333333333333334,0.288675134594813,
0.333333333333334,0.288675134594813,0.333333333333334,0.288675134594813,
0.333333333333334,0.288675134594813,0.333333333333334),(0.333333333333334,
0.288675134594813,0.333333333333334,0.288675134594813,0.333333333333334,
0.288675134594813,0.333333333333334,0.288675134594813,0.333333333333334,
0.288675134594813,0.333333333333334,0.288675134594813,0.333333333333334,
0.288675134594813,0.333333333333334,0.288675134594813,0.333333333333334,
0.288675134594813,0.333333333333334,0.288675134594813,0.333333333333334,
0.288675134594813,0.333333333333334,0.288675134594813,0.333333333333334,
0.288675134594813,0.333333333333334,0.288675134594813,0.333333333333334,
0.288675134594813,0.333333333333334,0.288675134594813,0.333333333333334,
0.288675134594813,0.333333333333334,0.288675134594813,0.333333333333334,
0.288675134594813,0.333333333333334,0.288675134594813,0.333333333333334,
0.288675134594813,0.333333333333334,0.288675134594813,0.333333333333334,
0.288675134594813,0.333333333333334,0.288675134594813,0.333333333333334,
0.288675134594813,0.333333333333334,0.288675134594813,0.333333333333334,
0.288675134594813,0.333333333333334,0.288675134594813,0.333333333333334,
0.288675134594813,0.333333333333334,0.288675134594813,0.333333333333334,
0.288675134594813,0.333333333333334,0.288675134594813,0.333333333333334,
0.288675134594813,0.333333333333334,0.288675134594813,0.333333333333334,
0.288675134594813,0.333333333333334,0.288675134594813,0.333333333333334,
0.288675134594813,0.333333333333334,0.288675134594813,0.333333333333334,
0.288675134594813,0.333333333333334,0.288675134594813,0.333333333333334,
0.288675134594813,0.333333333333334,0.288675134594813,0.333333333333334,
0.288675134594813,0.333333333333334,0.288675134594813,0.333333333333334,
0.288675134594813,0.333333333333334,0.288675134594813,0.333333333333334,
0.288675134594813,0.333333333333334,0.288675134594813,0.333333333333334,
0.288675134594813,0.333333333333334,0.288675134594813,0.333333333333334,
0.288675134594813,0.333333333333334,0.288675134594813,0.333333333333334,
0.288675134594813,0.333333333333334,0.288675134594813,0.333333333333334,
0.288675134594813,0.333333333333334,0.288675134594813,0.333333333333334,
0.288675134594813,0.333333333333334,0.288675134594813,0.333333333333334,
0.288675134594813,0.333333333333334,0.288675134594813,0.333333333333334),
(1.,0.866025403784439,1.,0.866025403784439,1.,0.866025403784439,1.,0.866025403784439,
1.,0.866025403784439,1.,0.866025403784439,1.,0.866025403784439,1.,0.866025403784439,
1.,0.866025403784439,1.,0.866025403784439,1.,0.866025403784439,1.,0.866025403784439,
1.,0.866025403784439,1.,0.866025403784439,1.,0.866025403784439,1.,0.866025403784439,
1.,0.866025403784439,1.,0.866025403784439,1.,0.866025403784439,1.,0.866025403784439,
1.,0.866025403784439,1.,0.866025403784439,1.,0.866025403784439,1.,0.866025403784439,
1.,0.866025403784439,1.,0.866025403784439,1.,0.866025403784439,1.,0.866025403784439,
1.,0.866025403784439,1.,0.866025403784439,1.,0.866025403784439,1.,0.866025403784439,
1.,0.866025403784439,1.,0.866025403784439,1.,0.866025403784439,1.,0.866025403784439,
1.,0.866025403784439,1.,0.866025403784439,1.,0.866025403784439,1.,0.866025403784439,
1.,0.866025403784439,1.,0.866025403784439,1.,0.866025403784439,1.,0.866025403784439,
1.,0.866025403784439,1.,0.866025403784439,1.,0.866025403784439,1.,0.866025403784439,
1.,0.866025403784439,1.,0.866025403784439,1.,0.866025403784439,1.,0.866025403784439,
1.,0.866025403784439,1.,0.866025403784439,1.,0.866025403784439,1.,0.866025403784439,
1.,0.866025403784439,1.,0.866025403784439,1.,0.866025403784439,1.,0.866025403784439,
1.),(0.333333333333334,0.288675134594813,0.333333333333334,0.288675134594813,
0.333333333333334,0.288675134594813,0.333333333333334,0.288675134594813,
0.333333333333334,0.288675134594813,0.333333333333334,0.288675134594813,
0.333333333333334,0.288675134594813,0.333333333333334,0.288675134594813,
0.333333333333334,0.288675134594813,0.333333333333334,0.288675134594813,
0.333333333333334,0.288675134594813,0.333333333333334,0.288675134594813,
0.333333333333334,0.288675134594813,0.333333333333334,0.288675134594813,
0.333333333333334,0.288675134594813,0.333333333333334,0.288675134594813,
0.333333333333334,0.288675134594813,0.333333333333334,0.288675134594813,
0.333333333333334,0.288675134594813,0.333333333333334,0.288675134594813,
0.333333333333334,0.288675134594813,0.333333333333334,0.288675134594813,
0.333333333333334,0.288675134594813,0.333333333333334,0.288675134594813,
0.333333333333334,0.288675134594813,0.333333333333334,0.288675134594813,
0.333333333333334,0.288675134594813,0.333333333333334,0.288675134594813,
0.333333333333334,0.288675134594813,0.333333333333334,0.288675134594813,
0.333333333333334,0.288675134594813,0.333333333333334,0.288675134594813,
0.333333333333334,0.288675134594813,0.333333333333334,0.288675134594813,
0.333333333333334,0.288675134594813,0.333333333333334,0.288675134594813,
0.333333333333334,0.288675134594813,0.333333333333334,0.288675134594813,
0.333333333333334,0.288675134594813,0.333333333333334,0.288675134594813,
0.333333333333334,0.288675134594813,0.333333333333334,0.288675134594813,
0.333333333333334,0.288675134594813,0.333333333333334,0.288675134594813,
0.333333333333334,0.288675134594813,0.333333333333334,0.288675134594813,
0.333333333333334,0.288675134594813,0.333333333333334,0.288675134594813,
0.333333333333334,0.288675134594813,0.333333333333334,0.288675134594813,
0.333333333333334,0.288675134594813,0.333333333333334,0.288675134594813,
0.333333333333334,0.288675134594813,0.333333333333334,0.288675134594813,
0.333333333333334,0.288675134594813,0.333333333333334,0.288675134594813,
0.333333333333334,0.288675134594813,0.333333333333334,0.288675134594813,
0.333333333333334,0.288675134594813,0.333333333333334,0.288675134594813,
0.333333333333334),(0.333333333333334,0.288675134594813,0.333333333333334,
0.288675134594813,0.333333333333334,0.288675134594813,0.333333333333334,
0.288675134594813,0.333333333333334,0.288675134594813,0.333333333333334,
0.288675134594813,0.333333333333334,0.288675134594813,0.333333333333334,
0.288675134594813,0.333333333333334,0.288675134594813,0.333333333333334,
0.288675134594813,0.333333333333334,0.288675134594813,0.333333333333334,
0.288675134594813,0.333333333333334,0.288675134594813,0.333333333333334,
0.288675134594813,0.333333333333334,0.288675134594813,0.333333333333334,
0.288675134594813,0.333333333333334,0.288675134594813,0.333333333333334,
0.288675134594813,0.333333333333334,0.288675134594813,0.333333333333334,
0.288675134594813,0.333333333333334,0.288675134594813,0.333333333333334,
0.288675134594813,0.333333333333334,0.288675134594813,0.333333333333334,
0.288675134594813,0.333333333333334,0.288675134594813,0.333333333333334,
0.288675134594813,0.333333333333334,0.288675134594813,0.333333333333334,
0.288675134594813,0.333333333333334,0.288675134594813,0.333333333333334,
0.288675134594813,0.333333333333334,0.288675134594813,0.333333333333334,
0.288675134594813,0.333333333333334,0.288675134594813,0.333333333333334,
0.288675134594813,0.333333333333334,0.288675134594813,0.333333333333334,
0.288675134594813,0.333333333333334,0.288675134594813,0.333333333333334,
0.288675134594813,0.333333333333334,0.288675134594813,0.333333333333334,
0.288675134594813,0.333333333333334,0.288675134594813,0.333333333333334,
0.288675134594813,0.333333333333334,0.288675134594813,0.333333333333334,
0.288675134594813,0.333333333333334,0.288675134594813,0.333333333333334,
0.288675134594813,0.333333333333334,0.288675134594813,0.333333333333334,
0.288675134594813,0.333333333333334,0.288675134594813,0.333333333333334,
0.288675134594813,0.333333333333334,0.288675134594813,0.333333333333334,
0.288675134594813,0.333333333333334,0.288675134594813,0.333333333333334,
0.288675134594813,0.333333333333334,0.288675134594813,0.333333333333334,
0.288675134594813,0.333333333333334,0.288675134594813,0.333333333333334,
0.288675134594813,0.333333333333334,0.288675134594813,0.333333333333334,
0.288675134594813,0.333333333333334),(1.,0.866025403784439,1.,0.866025403784439,
1.,0.866025403784439,1.,0.866025403784439,1.,0.866025403784439,1.,0.866025403784439,
1.,0.866025403784439,1.,0.866025403784439,1.,0.866025403784439,1.,0.866025403784439,
1.,0.866025403784439,1.,0.866025403784439,1.,0.866025403784439,1.,0.866025403784439,
1.,0.866025403784439,1.,0.866025403784439,1.,0.866025403784439,1.,0.866025403784439,
1.,0.866025403784439,1.,0.866025403784439,1.,0.866025403784439,1.,0.866025403784439,
1.,0.866025403784439,1.,0.866025403784439,1.,0.866025403784439,1.,0.866025403784439,
1.,0.866025403784439,1.,0.866025403784439,1.,0.866025403784439,1.,0.866025403784439,
1.,0.866025403784439,1.,0.866025403784439,1.,0.866025403784439,1.,0.866025403784439,
1.,0.866025403784439,1.,0.866025403784439,1.,0.866025403784439,1.,0.866025403784439,
1.,0.866025403784439,1.,0.866025403784439,1.,0.866025403784439,1.,0.866025403784439,
1.,0.866025403784439,1.,0.866025403784439,1.,0.866025403784439,1.,0.866025403784439,
1.,0.866025403784439,1.,0.866025403784439,1.,0.866025403784439,1.,0.866025403784439,
1.,0.866025403784439,1.,0.866025403784439,1.,0.866025403784439,1.,0.866025403784439,
1.,0.866025403784439,1.,0.866025403784439,1.,0.866025403784439,1.,0.866025403784439,
1.,0.866025403784439,1.,0.866025403784439,1.)))
REPRESENTATION_ITEM('')
SURFACE()
);
#150=(
BOUNDED_SURFACE()
B_SPLINE_SURFACE(3,2,((#37853,#37854,#37855),(#37856,#37857,#37858),(#37859,
#37860,#37861),(#37862,#37863,#37864),(#37865,#37866,#37867),(#37868,#37869,
#37870),(#37871,#37872,#37873),(#37874,#37875,#37876),(#37877,#37878,#37879),
(#37880,#37881,#37882),(#37883,#37884,#37885),(#37886,#37887,#37888),(#37889,
#37890,#37891),(#37892,#37893,#37894),(#37895,#37896,#37897),(#37898,#37899,
#37900),(#37901,#37902,#37903),(#37904,#37905,#37906),(#37907,#37908,#37909),
(#37910,#37911,#37912),(#37913,#37914,#37915),(#37916,#37917,#37918),(#37919,
#37920,#37921),(#37922,#37923,#37924),(#37925,#37926,#37927),(#37928,#37929,
#37930),(#37931,#37932,#37933),(#37934,#37935,#37936),(#37937,#37938,#37939),
(#37940,#37941,#37942),(#37943,#37944,#37945),(#37946,#37947,#37948),(#37949,
#37950,#37951),(#37952,#37953,#37954),(#37955,#37956,#37957),(#37958,#37959,
#37960),(#37961,#37962,#37963),(#37964,#37965,#37966),(#37967,#37968,#37969),
(#37970,#37971,#37972),(#37973,#37974,#37975),(#37976,#37977,#37978),(#37979,
#37980,#37981),(#37982,#37983,#37984),(#37985,#37986,#37987),(#37988,#37989,
#37990),(#37991,#37992,#37993),(#37994,#37995,#37996),(#37997,#37998,#37999),
(#38000,#38001,#38002),(#38003,#38004,#38005),(#38006,#38007,#38008),(#38009,
#38010,#38011),(#38012,#38013,#38014),(#38015,#38016,#38017),(#38018,#38019,
#38020),(#38021,#38022,#38023),(#38024,#38025,#38026),(#38027,#38028,#38029),
(#38030,#38031,#38032),(#38033,#38034,#38035),(#38036,#38037,#38038),(#38039,
#38040,#38041),(#38042,#38043,#38044),(#38045,#38046,#38047),(#38048,#38049,
#38050),(#38051,#38052,#38053),(#38054,#38055,#38056),(#38057,#38058,#38059),
(#38060,#38061,#38062),(#38063,#38064,#38065),(#38066,#38067,#38068),(#38069,
#38070,#38071),(#38072,#38073,#38074),(#38075,#38076,#38077),(#38078,#38079,
#38080),(#38081,#38082,#38083),(#38084,#38085,#38086),(#38087,#38088,#38089),
(#38090,#38091,#38092),(#38093,#38094,#38095),(#38096,#38097,#38098),(#38099,
#38100,#38101),(#38102,#38103,#38104),(#38105,#38106,#38107),(#38108,#38109,
#38110),(#38111,#38112,#38113),(#38114,#38115,#38116),(#38117,#38118,#38119),
(#38120,#38121,#38122),(#38123,#38124,#38125),(#38126,#38127,#38128),(#38129,
#38130,#38131),(#38132,#38133,#38134),(#38135,#38136,#38137),(#38138,#38139,
#38140),(#38141,#38142,#38143),(#38144,#38145,#38146),(#38147,#38148,#38149),
(#38150,#38151,#38152),(#38153,#38154,#38155),(#38156,#38157,#38158),(#38159,
#38160,#38161),(#38162,#38163,#38164),(#38165,#38166,#38167),(#38168,#38169,
#38170),(#38171,#38172,#38173),(#38174,#38175,#38176),(#38177,#38178,#38179),
(#38180,#38181,#38182),(#38183,#38184,#38185),(#38186,#38187,#38188),(#38189,
#38190,#38191),(#38192,#38193,#38194),(#38195,#38196,#38197),(#38198,#38199,
#38200),(#38201,#38202,#38203),(#38204,#38205,#38206),(#38207,#38208,#38209),
(#38210,#38211,#38212),(#38213,#38214,#38215),(#38216,#38217,#38218),(#38219,
#38220,#38221),(#38222,#38223,#38224),(#38225,#38226,#38227),(#38228,#38229,
#38230),(#38231,#38232,#38233),(#38234,#38235,#38236),(#38237,#38238,#38239),
(#38240,#38241,#38242),(#38243,#38244,#38245),(#38246,#38247,#38248),(#38249,
#38250,#38251),(#38252,#38253,#38254),(#38255,#38256,#38257),(#38258,#38259,
#38260),(#38261,#38262,#38263),(#38264,#38265,#38266),(#38267,#38268,#38269),
(#38270,#38271,#38272),(#38273,#38274,#38275),(#38276,#38277,#38278),(#38279,
#38280,#38281),(#38282,#38283,#38284),(#38285,#38286,#38287),(#38288,#38289,
#38290),(#38291,#38292,#38293),(#38294,#38295,#38296)),.UNSPECIFIED.,.T.,
 .F.,.F.)
B_SPLINE_SURFACE_WITH_KNOTS((4,2,2,2,2,2,2,2,2,2,2,2,2,2,2,2,2,2,2,2,2,
2,2,2,2,2,2,2,2,2,2,2,2,2,2,2,2,2,2,2,2,2,2,2,2,2,2,2,2,2,2,2,2,2,2,2,2,
2,2,2,2,2,2,2,2,2,2,2,2,2,2,2,2,4),(3,3),(0.,5.88439546912971E-5,8.82659320369456E-5,
0.00010297692070977,0.000117687909382594,0.000176531864073891,0.000191242852746715,
0.00020595384141954,0.000235375818765188,0.000294219773456485,0.000301575267792897,
0.00030893076212931,0.000323641750802134,0.000353063728147782,0.000382485705493431,
0.000397196694166255,0.000404552188502667,0.000411907682839079,0.000470751637530376,
0.000500173614876025,0.000514884603548849,0.000529595592221674,0.00058843954691297,
0.000603150535585795,0.000617861524258619,0.000647283501604268,0.000706127456295565,
0.000713482950631977,0.000720838444968389,0.000735549433641213,0.000764971410986862,
0.00079439338833251,0.000809104377005334,0.000823815365678159,0.000882659320369456,
0.00089737030904228,0.000912081297715104,0.000941503275060753,0.000970925252406401,
0.000985636241079226,0.00100034722975205,0.00105919118444335,0.00107390217311617,
0.001088613161789,0.00111803513913464,0.00117687909382594,0.00120630107117159,
0.00123572304851724,0.00126514502586289,0.00127985601453571,0.00129456700320854,
0.00135341095789983,0.00136812194657266,0.00138283293524548,0.00141225491259113,
0.00147109886728243,0.00147845436161884,0.00148580985595525,0.00150052084462807,
0.00152994282197372,0.00155936479931937,0.0015740757879922,0.00158878677666502,
0.00164763073135632,0.00167705270870197,0.00168440820303838,0.00169176369737479,
0.00170647468604761,0.00176531864073891,0.00178002962941174,0.00179474061808456,
0.00182416259543021,0.00185358457277586,0.00188300655012151),(0.,1.),
 .UNSPECIFIED.)
GEOMETRIC_REPRESENTATION_ITEM()
RATIONAL_B_SPLINE_SURFACE(((1.,0.715726527571974,1.),(1.,0.712824837312312,
1.),(1.,0.709939183288703,1.),(1.,0.70563780485041,1.),(1.,0.704208324053071,
1.),(1.,0.702070408823295,1.),(1.,0.701358182508267,1.),(1.,0.699938470033913,
1.),(1.,0.699235558344621,1.),(1.,0.695754807328025,1.),(1.,0.693077556893273,
1.),(1.,0.689858407232006,1.),(1.,0.689220997236269,1.),(1.,0.687959045727463,
1.),(1.,0.687333603220981,1.),(1.,0.685482641655898,1.),(1.,0.684295233247551,
1.),(1.,0.680865948622576,1.),(1.,0.678755828779441,1.),(1.,0.676577048170574,
1.),(1.,0.676337696500587,1.),(1.,0.675864499150325,1.),(1.,0.675630328898002,
1.),(1.,0.674939074618547,1.),(1.,0.674493188941281,1.),(1.,0.673199210425328,
1.),(1.,0.672394697221168,1.),(1.,0.670898516819421,1.),(1.,0.67020685543305,
1.),(1.,0.669254011840167,1.),(1.,0.668950530912342,1.),(1.,0.668516758864078,
1.),(1.,0.668375744076451,1.),(1.,0.668100931680429,1.),(1.,0.66796703830326,
1.),(1.,0.666801110120948,1.),(1.,0.666028636022973,1.),(1.,0.665248431462833,
1.),(1.,0.665051947055941,1.),(1.,0.664854970332435,1.),(1.,0.664805603591522,
1.),(1.,0.664740760515236,1.),(1.,0.664725098690157,1.),(1.,0.664729031892036,
1.),(1.,0.664992831063146,1.),(1.,0.665649916349412,1.),(1.,0.665797857858843,
1.),(1.,0.666127492088933,1.),(1.,0.666309421952839,1.),(1.,0.666899952411735,
1.),(1.,0.667354870043226,1.),(1.,0.668899800350139,1.),(1.,0.670168108270442,
1.),(1.,0.671877972859038,1.),(1.,0.672071972172369,1.),(1.,0.672465766634245,
1.),(1.,0.672665825106501,1.),(1.,0.673275414881356,1.),(1.,0.673694356676243,
1.),(1.,0.674988511758639,1.),(1.,0.675900966431535,1.),(1.,0.677825804601594,
1.),(1.,0.678838181026788,1.),(1.,0.680434320387322,1.),(1.,0.680979480786494,
1.),(1.,0.682095794766937,1.),(1.,0.682662909252039,1.),(1.,0.68554058312361,
1.),(1.,0.687978699058213,1.),(1.,0.69120098153353,1.),(1.,0.691854240148126,
1.),(1.,0.693178775224038,1.),(1.,0.693851046877455,1.),(1.,0.695888940711959,
1.),(1.,0.697266250733029,1.),(1.,0.700058726696578,1.),(1.,0.701473890706926,
1.),(1.,0.703625959383263,1.),(1.,0.704345718616287,1.),(1.,0.705783355102051,
1.),(1.,0.706502269097388,1.),(1.,0.71009740810345,1.),(1.,0.712975541569779,
1.),(1.,0.716575141001572,1.),(1.,0.717295144791949,1.),(1.,0.718735249984781,
1.),(1.,0.719451276741359,1.),(1.,0.721578968626909,1.),(1.,0.722973916817993,
1.),(1.,0.727088200171688,1.),(1.,0.729737986565996,1.),(1.,0.733557197223877,
1.),(1.,0.734784504108155,1.),(1.,0.737143649706032,1.),(1.,0.738276364056428,
1.),(1.,0.740446615586834,1.),(1.,0.741484163457107,1.),(1.,0.742965865508942,
1.),(1.,0.743447540320556,1.),(1.,0.744384190268116,1.),(1.,0.744835768417984,
1.),(1.,0.747010115951137,1.),(1.,0.748485471872314,1.),(1.,0.749993321046985,
1.),(1.,0.750277933331016,1.),(1.,0.750812495848506,1.),(1.,0.751062871482513,
1.),(1.,0.751757652067472,1.),(1.,0.752142025968554,1.),(1.,0.753064753379183,
1.),(1.,0.753374703098945,1.),(1.,0.753370274811438,1.),(1.,0.753364836618584,
1.),(1.,0.753343954153974,1.),(1.,0.753328486568168,1.),(1.,0.753267330936153,
1.),(1.,0.753206862795746,1.),(1.,0.752967583346212,1.),(1.,0.752731013298035,
1.),(1.,0.752107006678872,1.),(1.,0.751719566002465,1.),(1.,0.751024658994972,
1.),(1.,0.75077403600156,1.),(1.,0.750234324747068,1.),(1.,0.749944553237197,
1.),(1.,0.748414981448763,1.),(1.,0.746926622748835,1.),(1.,0.744319366838701,
1.),(1.,0.743387383255421,1.),(1.,0.742142765249864,1.),(1.,0.741889533171004,
1.),(1.,0.74137762258562,1.),(1.,0.74111874517533,1.),(1.,0.740333498527515,
1.),(1.,0.739798515633772,1.),(1.,0.737067782822572,1.),(1.,0.73470619863159,
1.),(1.,0.731541347327889,1.),(1.,0.73089763158831,1.),(1.,0.729588498808487,
1.),(1.,0.728926359265131,1.),(1.,0.726927210402846,1.),(1.,0.725573615722195,
1.),(1.,0.722827030199711,1.),(1.,0.721434033464342,1.),(1.,0.718609414473237,
1.),(1.,0.717177372701805,1.),(1.,0.715726527571974,1.)))
REPRESENTATION_ITEM('')
SURFACE()
);
#151=(
BOUNDED_SURFACE()
B_SPLINE_SURFACE(3,2,((#38515,#38516,#38517),(#38518,#38519,#38520),(#38521,
#38522,#38523),(#38524,#38525,#38526),(#38527,#38528,#38529),(#38530,#38531,
#38532),(#38533,#38534,#38535),(#38536,#38537,#38538),(#38539,#38540,#38541),
(#38542,#38543,#38544),(#38545,#38546,#38547),(#38548,#38549,#38550),(#38551,
#38552,#38553),(#38554,#38555,#38556),(#38557,#38558,#38559),(#38560,#38561,
#38562),(#38563,#38564,#38565),(#38566,#38567,#38568),(#38569,#38570,#38571),
(#38572,#38573,#38574),(#38575,#38576,#38577),(#38578,#38579,#38580),(#38581,
#38582,#38583),(#38584,#38585,#38586),(#38587,#38588,#38589),(#38590,#38591,
#38592),(#38593,#38594,#38595),(#38596,#38597,#38598),(#38599,#38600,#38601),
(#38602,#38603,#38604),(#38605,#38606,#38607),(#38608,#38609,#38610),(#38611,
#38612,#38613),(#38614,#38615,#38616),(#38617,#38618,#38619),(#38620,#38621,
#38622),(#38623,#38624,#38625),(#38626,#38627,#38628),(#38629,#38630,#38631),
(#38632,#38633,#38634),(#38635,#38636,#38637),(#38638,#38639,#38640),(#38641,
#38642,#38643),(#38644,#38645,#38646),(#38647,#38648,#38649),(#38650,#38651,
#38652),(#38653,#38654,#38655),(#38656,#38657,#38658),(#38659,#38660,#38661),
(#38662,#38663,#38664),(#38665,#38666,#38667),(#38668,#38669,#38670),(#38671,
#38672,#38673),(#38674,#38675,#38676),(#38677,#38678,#38679),(#38680,#38681,
#38682),(#38683,#38684,#38685),(#38686,#38687,#38688),(#38689,#38690,#38691),
(#38692,#38693,#38694),(#38695,#38696,#38697),(#38698,#38699,#38700),(#38701,
#38702,#38703),(#38704,#38705,#38706),(#38707,#38708,#38709),(#38710,#38711,
#38712),(#38713,#38714,#38715),(#38716,#38717,#38718),(#38719,#38720,#38721),
(#38722,#38723,#38724),(#38725,#38726,#38727),(#38728,#38729,#38730),(#38731,
#38732,#38733),(#38734,#38735,#38736),(#38737,#38738,#38739),(#38740,#38741,
#38742),(#38743,#38744,#38745),(#38746,#38747,#38748),(#38749,#38750,#38751),
(#38752,#38753,#38754),(#38755,#38756,#38757),(#38758,#38759,#38760),(#38761,
#38762,#38763),(#38764,#38765,#38766),(#38767,#38768,#38769),(#38770,#38771,
#38772),(#38773,#38774,#38775),(#38776,#38777,#38778),(#38779,#38780,#38781),
(#38782,#38783,#38784),(#38785,#38786,#38787),(#38788,#38789,#38790),(#38791,
#38792,#38793),(#38794,#38795,#38796),(#38797,#38798,#38799),(#38800,#38801,
#38802),(#38803,#38804,#38805),(#38806,#38807,#38808),(#38809,#38810,#38811),
(#38812,#38813,#38814),(#38815,#38816,#38817),(#38818,#38819,#38820),(#38821,
#38822,#38823),(#38824,#38825,#38826),(#38827,#38828,#38829),(#38830,#38831,
#38832),(#38833,#38834,#38835),(#38836,#38837,#38838),(#38839,#38840,#38841),
(#38842,#38843,#38844),(#38845,#38846,#38847),(#38848,#38849,#38850),(#38851,
#38852,#38853),(#38854,#38855,#38856),(#38857,#38858,#38859),(#38860,#38861,
#38862),(#38863,#38864,#38865),(#38866,#38867,#38868),(#38869,#38870,#38871),
(#38872,#38873,#38874),(#38875,#38876,#38877),(#38878,#38879,#38880),(#38881,
#38882,#38883),(#38884,#38885,#38886),(#38887,#38888,#38889),(#38890,#38891,
#38892),(#38893,#38894,#38895),(#38896,#38897,#38898),(#38899,#38900,#38901),
(#38902,#38903,#38904),(#38905,#38906,#38907),(#38908,#38909,#38910),(#38911,
#38912,#38913),(#38914,#38915,#38916),(#38917,#38918,#38919),(#38920,#38921,
#38922),(#38923,#38924,#38925),(#38926,#38927,#38928),(#38929,#38930,#38931),
(#38932,#38933,#38934),(#38935,#38936,#38937),(#38938,#38939,#38940),(#38941,
#38942,#38943),(#38944,#38945,#38946),(#38947,#38948,#38949),(#38950,#38951,
#38952),(#38953,#38954,#38955),(#38956,#38957,#38958)),.UNSPECIFIED.,.T.,
 .F.,.F.)
B_SPLINE_SURFACE_WITH_KNOTS((4,2,2,2,2,2,2,2,2,2,2,2,2,2,2,2,2,2,2,2,2,
2,2,2,2,2,2,2,2,2,2,2,2,2,2,2,2,2,2,2,2,2,2,2,2,2,2,2,2,2,2,2,2,2,2,2,2,
2,2,2,2,2,2,2,2,2,2,2,2,2,2,2,2,4),(3,3),(0.,2.94572120696205E-5,5.89144241392409E-5,
8.83716362088614E-5,0.000103100242243672,0.000117828848278482,0.000176743272417723,
0.000206200484487343,0.000235657696556964,0.000294572120696205,0.000309300726731015,
0.000324029332765825,0.000353486544835446,0.000382943756905066,0.000397672362939876,
0.000405036665957281,0.000412400968974686,0.000471315393113927,0.000500772605183548,
0.000515501211218358,0.000530229817253168,0.000589144241392409,0.00060387284742722,
0.00061860145346203,0.00064805866553165,0.000706973089670891,0.000721701695705701,
0.000736430301740512,0.000765887513810132,0.000795344725879752,0.000810073331914563,
0.000824801937949373,0.000883716362088614,0.000898444968123424,0.000913173574158234,
0.000942630786227855,0.000972087998297475,0.000986816604332285,0.0010015452103671,
0.00106045963450634,0.00107518824054115,0.00108255254355855,0.00108991684657596,
0.00111937405864558,0.00117828848278482,0.00119301708881963,0.00120774569485444,
0.00123720290692406,0.00126666011899368,0.00128138872502849,0.0012961173310633,
0.00135503175520254,0.00136976036123735,0.00137712466425476,0.00138448896727216,
0.00141394617934178,0.00147286060348102,0.00148758920951583,0.00150231781555064,
0.00153177502762026,0.00156123223968988,0.00157596084572469,0.00159068945175951,
0.00164960387589875,0.00167906108796837,0.00168642539098577,0.00169378969400318,
0.00170851830003799,0.00176743272417723,0.00178216133021204,0.00179688993624685,
0.00182634714831647,0.00185580436038609,0.00188526157245571),(0.,1.),
 .UNSPECIFIED.)
GEOMETRIC_REPRESENTATION_ITEM()
RATIONAL_B_SPLINE_SURFACE(((1.,0.706768250621048,1.),(1.,0.708426298986424,
1.),(1.,0.71008008713948,1.),(1.,0.713376962618569,1.),(1.,0.715020497077106,
1.),(1.,0.718297519423347,1.),(1.,0.719931010200883,1.),(1.,0.722372962983203,
1.),(1.,0.723186044045656,1.),(1.,0.724807250742798,1.),(1.,0.725609732738587,
1.),(1.,0.729581079301821,1.),(1.,0.732629067598119,1.),(1.,0.736998113914005,
1.),(1.,0.738421550016217,1.),(1.,0.741190319959484,1.),(1.,0.742514778054944,
1.),(1.,0.74631005642732,1.),(1.,0.748604628218609,1.),(1.,0.751158032017892,
1.),(1.,0.751653549012408,1.),(1.,0.752608572928937,1.),(1.,0.75306560396881,
1.),(1.,0.754375982622539,1.),(1.,0.755168745312861,1.),(1.,0.756593080986396,
1.),(1.,0.757224656832598,1.),(1.,0.758048217054286,1.),(1.,0.758302072136257,
1.),(1.,0.758651166057736,1.),(1.,0.758762248731274,1.),(1.,0.758973701473796,
1.),(1.,0.759074180129559,1.),(1.,0.75992529243238,1.),(1.,0.760313664756985,
1.),(1.,0.760358379138884,1.),(1.,0.760283061324181,1.),(1.,0.760031210406024,
1.),(1.,0.759923663695399,1.),(1.,0.759664049141739,1.),(1.,0.759511979981949,
1.),(1.,0.758642742016197,1.),(1.,0.757601675913755,1.),(1.,0.755877310483683,
1.),(1.,0.755511111609718,1.),(1.,0.754735567621713,1.),(1.,0.75432615177884,
1.),(1.,0.753047436476538,1.),(1.,0.752123540268788,1.),(1.,0.749147228369339,
1.),(1.,0.746892043597223,1.),(1.,0.743737116871849,1.),(1.,0.743092518946092,
1.),(1.,0.741782460083778,1.),(1.,0.74111613029348,1.),(1.,0.739084256899976,
1.),(1.,0.737685905862985,1.),(1.,0.734804890076589,1.),(1.,0.733322221436288,
1.),(1.,0.731035362741923,1.),(1.,0.730261837049612,1.),(1.,0.728696721731266,
1.),(1.,0.727910041758493,1.),(1.,0.723956994901979,1.),(1.,0.72073248846334,
1.),(1.,0.716630623834303,1.),(1.,0.715806638742097,1.),(1.,0.71415140110213,
1.),(1.,0.713318880580274,1.),(1.,0.710818889674067,1.),(1.,0.709159874596443,
1.),(1.,0.705856827432451,1.),(1.,0.704212795668421,1.),(1.,0.701757740368045,
1.),(1.,0.70094258809021,1.),(1.,0.699329967906212,1.),(1.,0.698530836824196,
1.),(1.,0.694570217898487,1.),(1.,0.691513076412309,1.),(1.,0.68782527710447,
1.),(1.,0.687094446903374,1.),(1.,0.686008340574591,1.),(1.,0.685647981698853,
1.),(1.,0.684934623703741,1.),(1.,0.684581117243663,1.),(1.,0.682829208835022,
1.),(1.,0.681477582738208,1.),(1.,0.677566315979365,1.),(1.,0.675148976138824,
1.),(1.,0.672364992202017,1.),(1.,0.671822976516116,1.),(1.,0.670773369616535,
1.),(1.,0.670264872579329,1.),(1.,0.668787238113039,1.),(1.,0.667865848198686,
1.),(1.,0.666147791049292,1.),(1.,0.665351122681227,1.),(1.,0.664250505737303,
1.),(1.,0.663899342689736,1.),(1.,0.663229258567818,1.),(1.,0.662912812691936,
1.),(1.,0.661423454802151,1.),(1.,0.660523869740149,1.),(1.,0.659755087773086,
1.),(1.,0.659619291059147,1.),(1.,0.659442901571928,1.),(1.,0.659388657238171,
1.),(1.,0.659289365428024,1.),(1.,0.659244263596543,1.),(1.,0.659042755870835,
1.),(1.,0.658958196453633,1.),(1.,0.658926561787994,1.),(1.,0.65919923542524,
1.),(1.,0.659916945733705,1.),(1.,0.660080071316468,1.),(1.,0.66044206006233,
1.),(1.,0.660640827665059,1.),(1.,0.66128959367181,1.),(1.,0.661791926833545,
1.),(1.,0.662935104672839,1.),(1.,0.663575947273059,1.),(1.,0.664643501128785,
1.),(1.,0.665017098787334,1.),(1.,0.665800623734546,1.),(1.,0.666211239135607,
1.),(1.,0.668333553785471,1.),(1.,0.670266144225975,1.),(1.,0.673518819932723,
1.),(1.,0.674662432543349,1.),(1.,0.676169720992961,1.),(1.,0.676475354929264,
1.),(1.,0.677091212222312,1.),(1.,0.677401785378898,1.),(1.,0.67834139879166,
1.),(1.,0.678978329515477,1.),(1.,0.68221536599383,1.),(1.,0.684971199140434,
1.),(1.,0.68863449272668,1.),(1.,0.689378165047444,1.),(1.,0.690888190776147,
1.),(1.,0.691650293315998,1.),(1.,0.693949128739525,1.),(1.,0.695502049311963,
1.),(1.,0.698649001495033,1.),(1.,0.700243032118734,1.),(1.,0.703473401016461,
1.),(1.,0.705110202255672,1.),(1.,0.706768250621048,1.)))
REPRESENTATION_ITEM('')
SURFACE()
);
#152=(
BOUNDED_SURFACE()
B_SPLINE_SURFACE(3,2,((#39384,#39385,#39386),(#39387,#39388,#39389),(#39390,
#39391,#39392),(#39393,#39394,#39395),(#39396,#39397,#39398),(#39399,#39400,
#39401),(#39402,#39403,#39404),(#39405,#39406,#39407),(#39408,#39409,#39410),
(#39411,#39412,#39413),(#39414,#39415,#39416),(#39417,#39418,#39419),(#39420,
#39421,#39422),(#39423,#39424,#39425),(#39426,#39427,#39428),(#39429,#39430,
#39431),(#39432,#39433,#39434),(#39435,#39436,#39437),(#39438,#39439,#39440),
(#39441,#39442,#39443),(#39444,#39445,#39446),(#39447,#39448,#39449),(#39450,
#39451,#39452),(#39453,#39454,#39455),(#39456,#39457,#39458),(#39459,#39460,
#39461),(#39462,#39463,#39464),(#39465,#39466,#39467),(#39468,#39469,#39470),
(#39471,#39472,#39473),(#39474,#39475,#39476),(#39477,#39478,#39479),(#39480,
#39481,#39482),(#39483,#39484,#39485),(#39486,#39487,#39488),(#39489,#39490,
#39491),(#39492,#39493,#39494),(#39495,#39496,#39497),(#39498,#39499,#39500),
(#39501,#39502,#39503),(#39504,#39505,#39506),(#39507,#39508,#39509),(#39510,
#39511,#39512),(#39513,#39514,#39515),(#39516,#39517,#39518),(#39519,#39520,
#39521),(#39522,#39523,#39524),(#39525,#39526,#39527),(#39528,#39529,#39530),
(#39531,#39532,#39533),(#39534,#39535,#39536),(#39537,#39538,#39539),(#39540,
#39541,#39542),(#39543,#39544,#39545),(#39546,#39547,#39548),(#39549,#39550,
#39551),(#39552,#39553,#39554),(#39555,#39556,#39557),(#39558,#39559,#39560),
(#39561,#39562,#39563),(#39564,#39565,#39566),(#39567,#39568,#39569),(#39570,
#39571,#39572),(#39573,#39574,#39575),(#39576,#39577,#39578),(#39579,#39580,
#39581),(#39582,#39583,#39584),(#39585,#39586,#39587),(#39588,#39589,#39590),
(#39591,#39592,#39593),(#39594,#39595,#39596),(#39597,#39598,#39599),(#39600,
#39601,#39602),(#39603,#39604,#39605),(#39606,#39607,#39608),(#39609,#39610,
#39611),(#39612,#39613,#39614),(#39615,#39616,#39617),(#39618,#39619,#39620),
(#39621,#39622,#39623),(#39624,#39625,#39626),(#39627,#39628,#39629),(#39630,
#39631,#39632),(#39633,#39634,#39635),(#39636,#39637,#39638),(#39639,#39640,
#39641),(#39642,#39643,#39644),(#39645,#39646,#39647),(#39648,#39649,#39650),
(#39651,#39652,#39653),(#39654,#39655,#39656),(#39657,#39658,#39659),(#39660,
#39661,#39662),(#39663,#39664,#39665),(#39666,#39667,#39668),(#39669,#39670,
#39671),(#39672,#39673,#39674),(#39675,#39676,#39677),(#39678,#39679,#39680),
(#39681,#39682,#39683),(#39684,#39685,#39686),(#39687,#39688,#39689),(#39690,
#39691,#39692),(#39693,#39694,#39695),(#39696,#39697,#39698),(#39699,#39700,
#39701),(#39702,#39703,#39704),(#39705,#39706,#39707),(#39708,#39709,#39710),
(#39711,#39712,#39713),(#39714,#39715,#39716),(#39717,#39718,#39719),(#39720,
#39721,#39722),(#39723,#39724,#39725),(#39726,#39727,#39728),(#39729,#39730,
#39731),(#39732,#39733,#39734),(#39735,#39736,#39737),(#39738,#39739,#39740),
(#39741,#39742,#39743),(#39744,#39745,#39746),(#39747,#39748,#39749),(#39750,
#39751,#39752),(#39753,#39754,#39755),(#39756,#39757,#39758),(#39759,#39760,
#39761),(#39762,#39763,#39764),(#39765,#39766,#39767),(#39768,#39769,#39770),
(#39771,#39772,#39773),(#39774,#39775,#39776),(#39777,#39778,#39779),(#39780,
#39781,#39782),(#39783,#39784,#39785),(#39786,#39787,#39788),(#39789,#39790,
#39791),(#39792,#39793,#39794),(#39795,#39796,#39797),(#39798,#39799,#39800),
(#39801,#39802,#39803),(#39804,#39805,#39806),(#39807,#39808,#39809),(#39810,
#39811,#39812),(#39813,#39814,#39815),(#39816,#39817,#39818),(#39819,#39820,
#39821),(#39822,#39823,#39824),(#39825,#39826,#39827)),.UNSPECIFIED.,.T.,
 .F.,.F.)
B_SPLINE_SURFACE_WITH_KNOTS((4,2,2,2,2,2,2,2,2,2,2,2,2,2,2,2,2,2,2,2,2,
2,2,2,2,2,2,2,2,2,2,2,2,2,2,2,2,2,2,2,2,2,2,2,2,2,2,2,2,2,2,2,2,2,2,2,2,
2,2,2,2,2,2,2,2,2,2,2,2,2,2,2,2,4),(3,3),(0.,2.94572120696205E-5,5.89144241392409E-5,
8.83716362088614E-5,0.000103100242243672,0.000117828848278482,0.000176743272417723,
0.000206200484487343,0.000235657696556964,0.000294572120696205,0.000309300726731015,
0.000324029332765825,0.000353486544835446,0.000382943756905066,0.000397672362939876,
0.000405036665957281,0.000412400968974686,0.000471315393113927,0.000500772605183548,
0.000515501211218358,0.000530229817253168,0.000589144241392409,0.00060387284742722,
0.00061860145346203,0.00064805866553165,0.000706973089670891,0.000721701695705701,
0.000736430301740512,0.000765887513810132,0.000795344725879752,0.000810073331914563,
0.000824801937949373,0.000883716362088614,0.000898444968123424,0.000913173574158234,
0.000942630786227855,0.000972087998297475,0.000986816604332285,0.0010015452103671,
0.00106045963450634,0.00107518824054115,0.00108255254355855,0.00108991684657596,
0.00111937405864558,0.00117828848278482,0.00119301708881963,0.00120774569485444,
0.00123720290692406,0.00126666011899368,0.00128138872502849,0.0012961173310633,
0.00135503175520254,0.00136976036123735,0.00137712466425476,0.00138448896727216,
0.00141394617934178,0.00147286060348102,0.00148758920951583,0.00150231781555064,
0.00153177502762026,0.00156123223968988,0.00157596084572469,0.00159068945175951,
0.00164960387589875,0.00167906108796837,0.00168642539098577,0.00169378969400318,
0.00170851830003799,0.00176743272417723,0.00178216133021204,0.00179688993624685,
0.00182634714831647,0.00185580436038609,0.00188526157245571),(0.,1.),
 .UNSPECIFIED.)
GEOMETRIC_REPRESENTATION_ITEM()
RATIONAL_B_SPLINE_SURFACE(((1.,0.706768250621048,1.),(1.,0.708426298986424,
1.),(1.,0.71008008713948,1.),(1.,0.713376962618569,1.),(1.,0.715020497077106,
1.),(1.,0.718297519423347,1.),(1.,0.719931010200883,1.),(1.,0.722372962983203,
1.),(1.,0.723186044045656,1.),(1.,0.724807250742798,1.),(1.,0.725609732738587,
1.),(1.,0.729581079301821,1.),(1.,0.732629067598119,1.),(1.,0.736998113914005,
1.),(1.,0.738421550016217,1.),(1.,0.741190319959484,1.),(1.,0.742514778054944,
1.),(1.,0.74631005642732,1.),(1.,0.748604628218609,1.),(1.,0.751158032017892,
1.),(1.,0.751653549012408,1.),(1.,0.752608572928937,1.),(1.,0.75306560396881,
1.),(1.,0.754375982622539,1.),(1.,0.755168745312861,1.),(1.,0.756593080986396,
1.),(1.,0.757224656832598,1.),(1.,0.758048217054286,1.),(1.,0.758302072136257,
1.),(1.,0.758651166057736,1.),(1.,0.758762248731274,1.),(1.,0.758973701473796,
1.),(1.,0.759074180129559,1.),(1.,0.75992529243238,1.),(1.,0.760313664756985,
1.),(1.,0.760358379138884,1.),(1.,0.760283061324181,1.),(1.,0.760031210406024,
1.),(1.,0.759923663695399,1.),(1.,0.759664049141739,1.),(1.,0.759511979981949,
1.),(1.,0.758642742016197,1.),(1.,0.757601675913755,1.),(1.,0.755877310483683,
1.),(1.,0.755511111609718,1.),(1.,0.754735567621713,1.),(1.,0.75432615177884,
1.),(1.,0.753047436476538,1.),(1.,0.752123540268788,1.),(1.,0.749147228369339,
1.),(1.,0.746892043597223,1.),(1.,0.743737116871849,1.),(1.,0.743092518946092,
1.),(1.,0.741782460083778,1.),(1.,0.74111613029348,1.),(1.,0.739084256899976,
1.),(1.,0.737685905862985,1.),(1.,0.734804890076589,1.),(1.,0.733322221436288,
1.),(1.,0.731035362741923,1.),(1.,0.730261837049612,1.),(1.,0.728696721731266,
1.),(1.,0.727910041758493,1.),(1.,0.723956994901979,1.),(1.,0.72073248846334,
1.),(1.,0.716630623834303,1.),(1.,0.715806638742097,1.),(1.,0.71415140110213,
1.),(1.,0.713318880580274,1.),(1.,0.710818889674067,1.),(1.,0.709159874596443,
1.),(1.,0.705856827432451,1.),(1.,0.704212795668421,1.),(1.,0.701757740368045,
1.),(1.,0.70094258809021,1.),(1.,0.699329967906212,1.),(1.,0.698530836824196,
1.),(1.,0.694570217898487,1.),(1.,0.691513076412309,1.),(1.,0.68782527710447,
1.),(1.,0.687094446903374,1.),(1.,0.686008340574591,1.),(1.,0.685647981698853,
1.),(1.,0.684934623703741,1.),(1.,0.684581117243663,1.),(1.,0.682829208835022,
1.),(1.,0.681477582738208,1.),(1.,0.677566315979365,1.),(1.,0.675148976138824,
1.),(1.,0.672364992202017,1.),(1.,0.671822976516116,1.),(1.,0.670773369616535,
1.),(1.,0.670264872579329,1.),(1.,0.668787238113039,1.),(1.,0.667865848198686,
1.),(1.,0.666147791049292,1.),(1.,0.665351122681227,1.),(1.,0.664250505737303,
1.),(1.,0.663899342689736,1.),(1.,0.663229258567818,1.),(1.,0.662912812691936,
1.),(1.,0.661423454802151,1.),(1.,0.660523869740149,1.),(1.,0.659755087773086,
1.),(1.,0.659619291059147,1.),(1.,0.659442901571928,1.),(1.,0.659388657238171,
1.),(1.,0.659289365428024,1.),(1.,0.659244263596543,1.),(1.,0.659042755870835,
1.),(1.,0.658958196453633,1.),(1.,0.658926561787994,1.),(1.,0.65919923542524,
1.),(1.,0.659916945733705,1.),(1.,0.660080071316468,1.),(1.,0.66044206006233,
1.),(1.,0.660640827665059,1.),(1.,0.66128959367181,1.),(1.,0.661791926833545,
1.),(1.,0.662935104672839,1.),(1.,0.663575947273059,1.),(1.,0.664643501128785,
1.),(1.,0.665017098787334,1.),(1.,0.665800623734546,1.),(1.,0.666211239135607,
1.),(1.,0.668333553785471,1.),(1.,0.670266144225975,1.),(1.,0.673518819932723,
1.),(1.,0.674662432543349,1.),(1.,0.676169720992961,1.),(1.,0.676475354929264,
1.),(1.,0.677091212222312,1.),(1.,0.677401785378898,1.),(1.,0.67834139879166,
1.),(1.,0.678978329515477,1.),(1.,0.68221536599383,1.),(1.,0.684971199140434,
1.),(1.,0.68863449272668,1.),(1.,0.689378165047444,1.),(1.,0.690888190776147,
1.),(1.,0.691650293315998,1.),(1.,0.693949128739525,1.),(1.,0.695502049311963,
1.),(1.,0.698649001495033,1.),(1.,0.700243032118734,1.),(1.,0.703473401016461,
1.),(1.,0.705110202255672,1.),(1.,0.706768250621048,1.)))
REPRESENTATION_ITEM('')
SURFACE()
);
#153=(
BOUNDED_SURFACE()
B_SPLINE_SURFACE(3,2,((#40039,#40040,#40041),(#40042,#40043,#40044),(#40045,
#40046,#40047),(#40048,#40049,#40050),(#40051,#40052,#40053),(#40054,#40055,
#40056),(#40057,#40058,#40059),(#40060,#40061,#40062),(#40063,#40064,#40065),
(#40066,#40067,#40068),(#40069,#40070,#40071),(#40072,#40073,#40074),(#40075,
#40076,#40077),(#40078,#40079,#40080),(#40081,#40082,#40083),(#40084,#40085,
#40086),(#40087,#40088,#40089),(#40090,#40091,#40092),(#40093,#40094,#40095),
(#40096,#40097,#40098),(#40099,#40100,#40101),(#40102,#40103,#40104),(#40105,
#40106,#40107),(#40108,#40109,#40110),(#40111,#40112,#40113),(#40114,#40115,
#40116),(#40117,#40118,#40119),(#40120,#40121,#40122),(#40123,#40124,#40125),
(#40126,#40127,#40128),(#40129,#40130,#40131),(#40132,#40133,#40134),(#40135,
#40136,#40137),(#40138,#40139,#40140),(#40141,#40142,#40143),(#40144,#40145,
#40146),(#40147,#40148,#40149),(#40150,#40151,#40152),(#40153,#40154,#40155),
(#40156,#40157,#40158),(#40159,#40160,#40161),(#40162,#40163,#40164),(#40165,
#40166,#40167),(#40168,#40169,#40170),(#40171,#40172,#40173),(#40174,#40175,
#40176),(#40177,#40178,#40179),(#40180,#40181,#40182),(#40183,#40184,#40185),
(#40186,#40187,#40188),(#40189,#40190,#40191),(#40192,#40193,#40194),(#40195,
#40196,#40197),(#40198,#40199,#40200),(#40201,#40202,#40203),(#40204,#40205,
#40206),(#40207,#40208,#40209),(#40210,#40211,#40212),(#40213,#40214,#40215),
(#40216,#40217,#40218),(#40219,#40220,#40221),(#40222,#40223,#40224),(#40225,
#40226,#40227),(#40228,#40229,#40230),(#40231,#40232,#40233),(#40234,#40235,
#40236),(#40237,#40238,#40239),(#40240,#40241,#40242),(#40243,#40244,#40245),
(#40246,#40247,#40248),(#40249,#40250,#40251),(#40252,#40253,#40254),(#40255,
#40256,#40257),(#40258,#40259,#40260),(#40261,#40262,#40263),(#40264,#40265,
#40266),(#40267,#40268,#40269),(#40270,#40271,#40272),(#40273,#40274,#40275),
(#40276,#40277,#40278),(#40279,#40280,#40281),(#40282,#40283,#40284),(#40285,
#40286,#40287),(#40288,#40289,#40290),(#40291,#40292,#40293),(#40294,#40295,
#40296),(#40297,#40298,#40299),(#40300,#40301,#40302),(#40303,#40304,#40305),
(#40306,#40307,#40308),(#40309,#40310,#40311),(#40312,#40313,#40314),(#40315,
#40316,#40317),(#40318,#40319,#40320),(#40321,#40322,#40323),(#40324,#40325,
#40326),(#40327,#40328,#40329),(#40330,#40331,#40332),(#40333,#40334,#40335),
(#40336,#40337,#40338),(#40339,#40340,#40341),(#40342,#40343,#40344),(#40345,
#40346,#40347),(#40348,#40349,#40350),(#40351,#40352,#40353),(#40354,#40355,
#40356),(#40357,#40358,#40359),(#40360,#40361,#40362),(#40363,#40364,#40365),
(#40366,#40367,#40368),(#40369,#40370,#40371),(#40372,#40373,#40374),(#40375,
#40376,#40377),(#40378,#40379,#40380),(#40381,#40382,#40383),(#40384,#40385,
#40386),(#40387,#40388,#40389),(#40390,#40391,#40392),(#40393,#40394,#40395),
(#40396,#40397,#40398),(#40399,#40400,#40401),(#40402,#40403,#40404),(#40405,
#40406,#40407),(#40408,#40409,#40410),(#40411,#40412,#40413),(#40414,#40415,
#40416),(#40417,#40418,#40419),(#40420,#40421,#40422),(#40423,#40424,#40425),
(#40426,#40427,#40428),(#40429,#40430,#40431),(#40432,#40433,#40434),(#40435,
#40436,#40437),(#40438,#40439,#40440),(#40441,#40442,#40443),(#40444,#40445,
#40446),(#40447,#40448,#40449),(#40450,#40451,#40452),(#40453,#40454,#40455),
(#40456,#40457,#40458),(#40459,#40460,#40461),(#40462,#40463,#40464),(#40465,
#40466,#40467),(#40468,#40469,#40470),(#40471,#40472,#40473),(#40474,#40475,
#40476),(#40477,#40478,#40479),(#40480,#40481,#40482)),.UNSPECIFIED.,.T.,
 .F.,.F.)
B_SPLINE_SURFACE_WITH_KNOTS((4,2,2,2,2,2,2,2,2,2,2,2,2,2,2,2,2,2,2,2,2,
2,2,2,2,2,2,2,2,2,2,2,2,2,2,2,2,2,2,2,2,2,2,2,2,2,2,2,2,2,2,2,2,2,2,2,2,
2,2,2,2,2,2,2,2,2,2,2,2,2,2,2,2,4),(3,3),(0.,5.88439546912971E-5,8.82659320369456E-5,
0.00010297692070977,0.000117687909382594,0.000176531864073891,0.000191242852746715,
0.00020595384141954,0.000235375818765188,0.000294219773456485,0.000301575267792897,
0.00030893076212931,0.000323641750802134,0.000353063728147782,0.000382485705493431,
0.000397196694166255,0.000404552188502667,0.000411907682839079,0.000470751637530376,
0.000500173614876025,0.000514884603548849,0.000529595592221674,0.00058843954691297,
0.000603150535585795,0.000617861524258619,0.000647283501604268,0.000706127456295565,
0.000713482950631977,0.000720838444968389,0.000735549433641213,0.000764971410986862,
0.00079439338833251,0.000809104377005334,0.000823815365678159,0.000882659320369456,
0.00089737030904228,0.000912081297715104,0.000941503275060753,0.000970925252406401,
0.000985636241079226,0.00100034722975205,0.00105919118444335,0.00107390217311617,
0.001088613161789,0.00111803513913464,0.00117687909382594,0.00120630107117159,
0.00123572304851724,0.00126514502586289,0.00127985601453571,0.00129456700320854,
0.00135341095789983,0.00136812194657266,0.00138283293524548,0.00141225491259113,
0.00147109886728243,0.00147845436161884,0.00148580985595525,0.00150052084462807,
0.00152994282197372,0.00155936479931937,0.0015740757879922,0.00158878677666502,
0.00164763073135632,0.00167705270870197,0.00168440820303838,0.00169176369737479,
0.00170647468604761,0.00176531864073891,0.00178002962941174,0.00179474061808456,
0.00182416259543021,0.00185358457277586,0.00188300655012151),(0.,1.),
 .UNSPECIFIED.)
GEOMETRIC_REPRESENTATION_ITEM()
RATIONAL_B_SPLINE_SURFACE(((1.,0.715726527571974,1.),(1.,0.712824837312312,
1.),(1.,0.709939183288703,1.),(1.,0.70563780485041,1.),(1.,0.704208324053071,
1.),(1.,0.702070408823295,1.),(1.,0.701358182508267,1.),(1.,0.699938470033913,
1.),(1.,0.699235558344621,1.),(1.,0.695754807328025,1.),(1.,0.693077556893273,
1.),(1.,0.689858407232006,1.),(1.,0.689220997236269,1.),(1.,0.687959045727463,
1.),(1.,0.687333603220981,1.),(1.,0.685482641655898,1.),(1.,0.684295233247551,
1.),(1.,0.680865948622576,1.),(1.,0.678755828779441,1.),(1.,0.676577048170574,
1.),(1.,0.676337696500587,1.),(1.,0.675864499150325,1.),(1.,0.675630328898002,
1.),(1.,0.674939074618547,1.),(1.,0.674493188941281,1.),(1.,0.673199210425328,
1.),(1.,0.672394697221168,1.),(1.,0.670898516819421,1.),(1.,0.67020685543305,
1.),(1.,0.669254011840167,1.),(1.,0.668950530912342,1.),(1.,0.668516758864078,
1.),(1.,0.668375744076451,1.),(1.,0.668100931680429,1.),(1.,0.66796703830326,
1.),(1.,0.666801110120948,1.),(1.,0.666028636022973,1.),(1.,0.665248431462833,
1.),(1.,0.665051947055941,1.),(1.,0.664854970332435,1.),(1.,0.664805603591522,
1.),(1.,0.664740760515236,1.),(1.,0.664725098690157,1.),(1.,0.664729031892036,
1.),(1.,0.664992831063146,1.),(1.,0.665649916349412,1.),(1.,0.665797857858843,
1.),(1.,0.666127492088933,1.),(1.,0.666309421952839,1.),(1.,0.666899952411735,
1.),(1.,0.667354870043226,1.),(1.,0.668899800350139,1.),(1.,0.670168108270442,
1.),(1.,0.671877972859038,1.),(1.,0.672071972172369,1.),(1.,0.672465766634245,
1.),(1.,0.672665825106501,1.),(1.,0.673275414881356,1.),(1.,0.673694356676243,
1.),(1.,0.674988511758639,1.),(1.,0.675900966431535,1.),(1.,0.677825804601594,
1.),(1.,0.678838181026788,1.),(1.,0.680434320387322,1.),(1.,0.680979480786494,
1.),(1.,0.682095794766937,1.),(1.,0.682662909252039,1.),(1.,0.68554058312361,
1.),(1.,0.687978699058213,1.),(1.,0.69120098153353,1.),(1.,0.691854240148126,
1.),(1.,0.693178775224038,1.),(1.,0.693851046877455,1.),(1.,0.695888940711959,
1.),(1.,0.697266250733029,1.),(1.,0.700058726696578,1.),(1.,0.701473890706926,
1.),(1.,0.703625959383263,1.),(1.,0.704345718616287,1.),(1.,0.705783355102051,
1.),(1.,0.706502269097388,1.),(1.,0.71009740810345,1.),(1.,0.712975541569779,
1.),(1.,0.716575141001572,1.),(1.,0.717295144791949,1.),(1.,0.718735249984781,
1.),(1.,0.719451276741359,1.),(1.,0.721578968626909,1.),(1.,0.722973916817993,
1.),(1.,0.727088200171688,1.),(1.,0.729737986565996,1.),(1.,0.733557197223877,
1.),(1.,0.734784504108155,1.),(1.,0.737143649706032,1.),(1.,0.738276364056428,
1.),(1.,0.740446615586834,1.),(1.,0.741484163457107,1.),(1.,0.742965865508942,
1.),(1.,0.743447540320556,1.),(1.,0.744384190268116,1.),(1.,0.744835768417984,
1.),(1.,0.747010115951137,1.),(1.,0.748485471872314,1.),(1.,0.749993321046985,
1.),(1.,0.750277933331016,1.),(1.,0.750812495848506,1.),(1.,0.751062871482513,
1.),(1.,0.751757652067472,1.),(1.,0.752142025968554,1.),(1.,0.753064753379183,
1.),(1.,0.753374703098945,1.),(1.,0.753370274811438,1.),(1.,0.753364836618584,
1.),(1.,0.753343954153974,1.),(1.,0.753328486568168,1.),(1.,0.753267330936153,
1.),(1.,0.753206862795746,1.),(1.,0.752967583346212,1.),(1.,0.752731013298035,
1.),(1.,0.752107006678872,1.),(1.,0.751719566002465,1.),(1.,0.751024658994972,
1.),(1.,0.75077403600156,1.),(1.,0.750234324747068,1.),(1.,0.749944553237197,
1.),(1.,0.748414981448763,1.),(1.,0.746926622748835,1.),(1.,0.744319366838701,
1.),(1.,0.743387383255421,1.),(1.,0.742142765249864,1.),(1.,0.741889533171004,
1.),(1.,0.74137762258562,1.),(1.,0.74111874517533,1.),(1.,0.740333498527515,
1.),(1.,0.739798515633772,1.),(1.,0.737067782822572,1.),(1.,0.73470619863159,
1.),(1.,0.731541347327889,1.),(1.,0.73089763158831,1.),(1.,0.729588498808487,
1.),(1.,0.728926359265131,1.),(1.,0.726927210402846,1.),(1.,0.725573615722195,
1.),(1.,0.722827030199711,1.),(1.,0.721434033464342,1.),(1.,0.718609414473237,
1.),(1.,0.717177372701805,1.),(1.,0.715726527571974,1.)))
REPRESENTATION_ITEM('')
SURFACE()
);
#154=(
BOUNDED_SURFACE()
B_SPLINE_SURFACE(3,2,((#40484,#40485,#40486,#40487,#40488,#40489,#40490,
#40491,#40492,#40493,#40494,#40495,#40496,#40497,#40498,#40499,#40500,#40501,
#40502,#40503,#40504,#40505,#40506,#40507,#40508,#40509,#40510,#40511,#40512,
#40513,#40514,#40515,#40516,#40517,#40518,#40519,#40520,#40521,#40522,#40523,
#40524,#40525,#40526,#40527,#40528,#40529,#40530,#40531,#40532,#40533,#40534,
#40535,#40536,#40537,#40538,#40539,#40540,#40541,#40542,#40543,#40544,#40545,
#40546,#40547,#40548,#40549,#40550,#40551,#40552,#40553,#40554,#40555,#40556,
#40557,#40558,#40559,#40560,#40561,#40562,#40563,#40564,#40565,#40566,#40567,
#40568,#40569,#40570,#40571,#40572,#40573,#40574,#40575,#40576,#40577,#40578,
#40579,#40580,#40581,#40582,#40583,#40584,#40585,#40586,#40587,#40588,#40589,
#40590,#40591,#40592,#40593,#40594,#40595,#40596,#40597,#40598,#40599,#40600,
#40601,#40602,#40603,#40604),(#40605,#40606,#40607,#40608,#40609,#40610,
#40611,#40612,#40613,#40614,#40615,#40616,#40617,#40618,#40619,#40620,#40621,
#40622,#40623,#40624,#40625,#40626,#40627,#40628,#40629,#40630,#40631,#40632,
#40633,#40634,#40635,#40636,#40637,#40638,#40639,#40640,#40641,#40642,#40643,
#40644,#40645,#40646,#40647,#40648,#40649,#40650,#40651,#40652,#40653,#40654,
#40655,#40656,#40657,#40658,#40659,#40660,#40661,#40662,#40663,#40664,#40665,
#40666,#40667,#40668,#40669,#40670,#40671,#40672,#40673,#40674,#40675,#40676,
#40677,#40678,#40679,#40680,#40681,#40682,#40683,#40684,#40685,#40686,#40687,
#40688,#40689,#40690,#40691,#40692,#40693,#40694,#40695,#40696,#40697,#40698,
#40699,#40700,#40701,#40702,#40703,#40704,#40705,#40706,#40707,#40708,#40709,
#40710,#40711,#40712,#40713,#40714,#40715,#40716,#40717,#40718,#40719,#40720,
#40721,#40722,#40723,#40724,#40725),(#40726,#40727,#40728,#40729,#40730,
#40731,#40732,#40733,#40734,#40735,#40736,#40737,#40738,#40739,#40740,#40741,
#40742,#40743,#40744,#40745,#40746,#40747,#40748,#40749,#40750,#40751,#40752,
#40753,#40754,#40755,#40756,#40757,#40758,#40759,#40760,#40761,#40762,#40763,
#40764,#40765,#40766,#40767,#40768,#40769,#40770,#40771,#40772,#40773,#40774,
#40775,#40776,#40777,#40778,#40779,#40780,#40781,#40782,#40783,#40784,#40785,
#40786,#40787,#40788,#40789,#40790,#40791,#40792,#40793,#40794,#40795,#40796,
#40797,#40798,#40799,#40800,#40801,#40802,#40803,#40804,#40805,#40806,#40807,
#40808,#40809,#40810,#40811,#40812,#40813,#40814,#40815,#40816,#40817,#40818,
#40819,#40820,#40821,#40822,#40823,#40824,#40825,#40826,#40827,#40828,#40829,
#40830,#40831,#40832,#40833,#40834,#40835,#40836,#40837,#40838,#40839,#40840,
#40841,#40842,#40843,#40844,#40845,#40846),(#40847,#40848,#40849,#40850,
#40851,#40852,#40853,#40854,#40855,#40856,#40857,#40858,#40859,#40860,#40861,
#40862,#40863,#40864,#40865,#40866,#40867,#40868,#40869,#40870,#40871,#40872,
#40873,#40874,#40875,#40876,#40877,#40878,#40879,#40880,#40881,#40882,#40883,
#40884,#40885,#40886,#40887,#40888,#40889,#40890,#40891,#40892,#40893,#40894,
#40895,#40896,#40897,#40898,#40899,#40900,#40901,#40902,#40903,#40904,#40905,
#40906,#40907,#40908,#40909,#40910,#40911,#40912,#40913,#40914,#40915,#40916,
#40917,#40918,#40919,#40920,#40921,#40922,#40923,#40924,#40925,#40926,#40927,
#40928,#40929,#40930,#40931,#40932,#40933,#40934,#40935,#40936,#40937,#40938,
#40939,#40940,#40941,#40942,#40943,#40944,#40945,#40946,#40947,#40948,#40949,
#40950,#40951,#40952,#40953,#40954,#40955,#40956,#40957,#40958,#40959,#40960,
#40961,#40962,#40963,#40964,#40965,#40966,#40967),(#40968,#40969,#40970,
#40971,#40972,#40973,#40974,#40975,#40976,#40977,#40978,#40979,#40980,#40981,
#40982,#40983,#40984,#40985,#40986,#40987,#40988,#40989,#40990,#40991,#40992,
#40993,#40994,#40995,#40996,#40997,#40998,#40999,#41000,#41001,#41002,#41003,
#41004,#41005,#41006,#41007,#41008,#41009,#41010,#41011,#41012,#41013,#41014,
#41015,#41016,#41017,#41018,#41019,#41020,#41021,#41022,#41023,#41024,#41025,
#41026,#41027,#41028,#41029,#41030,#41031,#41032,#41033,#41034,#41035,#41036,
#41037,#41038,#41039,#41040,#41041,#41042,#41043,#41044,#41045,#41046,#41047,
#41048,#41049,#41050,#41051,#41052,#41053,#41054,#41055,#41056,#41057,#41058,
#41059,#41060,#41061,#41062,#41063,#41064,#41065,#41066,#41067,#41068,#41069,
#41070,#41071,#41072,#41073,#41074,#41075,#41076,#41077,#41078,#41079,#41080,
#41081,#41082,#41083,#41084,#41085,#41086,#41087,#41088),(#41089,#41090,
#41091,#41092,#41093,#41094,#41095,#41096,#41097,#41098,#41099,#41100,#41101,
#41102,#41103,#41104,#41105,#41106,#41107,#41108,#41109,#41110,#41111,#41112,
#41113,#41114,#41115,#41116,#41117,#41118,#41119,#41120,#41121,#41122,#41123,
#41124,#41125,#41126,#41127,#41128,#41129,#41130,#41131,#41132,#41133,#41134,
#41135,#41136,#41137,#41138,#41139,#41140,#41141,#41142,#41143,#41144,#41145,
#41146,#41147,#41148,#41149,#41150,#41151,#41152,#41153,#41154,#41155,#41156,
#41157,#41158,#41159,#41160,#41161,#41162,#41163,#41164,#41165,#41166,#41167,
#41168,#41169,#41170,#41171,#41172,#41173,#41174,#41175,#41176,#41177,#41178,
#41179,#41180,#41181,#41182,#41183,#41184,#41185,#41186,#41187,#41188,#41189,
#41190,#41191,#41192,#41193,#41194,#41195,#41196,#41197,#41198,#41199,#41200,
#41201,#41202,#41203,#41204,#41205,#41206,#41207,#41208,#41209),(#41210,
#41211,#41212,#41213,#41214,#41215,#41216,#41217,#41218,#41219,#41220,#41221,
#41222,#41223,#41224,#41225,#41226,#41227,#41228,#41229,#41230,#41231,#41232,
#41233,#41234,#41235,#41236,#41237,#41238,#41239,#41240,#41241,#41242,#41243,
#41244,#41245,#41246,#41247,#41248,#41249,#41250,#41251,#41252,#41253,#41254,
#41255,#41256,#41257,#41258,#41259,#41260,#41261,#41262,#41263,#41264,#41265,
#41266,#41267,#41268,#41269,#41270,#41271,#41272,#41273,#41274,#41275,#41276,
#41277,#41278,#41279,#41280,#41281,#41282,#41283,#41284,#41285,#41286,#41287,
#41288,#41289,#41290,#41291,#41292,#41293,#41294,#41295,#41296,#41297,#41298,
#41299,#41300,#41301,#41302,#41303,#41304,#41305,#41306,#41307,#41308,#41309,
#41310,#41311,#41312,#41313,#41314,#41315,#41316,#41317,#41318,#41319,#41320,
#41321,#41322,#41323,#41324,#41325,#41326,#41327,#41328,#41329,#41330)),
 .UNSPECIFIED.,.T.,.F.,.F.)
B_SPLINE_SURFACE_WITH_KNOTS((4,3,4),(3,2,2,2,2,2,2,2,2,2,2,2,2,2,2,2,2,
2,2,2,2,2,2,2,2,2,2,2,2,2,2,2,2,2,2,2,2,2,2,2,2,2,2,2,2,2,2,2,2,2,2,2,2,
2,2,2,2,2,2,2,3),(0.,0.5,1.),(0.,0.0166666666666666,0.0333333333333333,
0.05,0.0666666666666667,0.0833333333333333,0.1,0.116666666666667,0.133333333333333,
0.15,0.166666666666667,0.183333333333334,0.2,0.216666666666667,0.233333333333334,
0.25,0.266666666666667,0.283333333333334,0.3,0.316666666666666,0.333333333333334,
0.35,0.366666666666666,0.383333333333334,0.4,0.416666666666667,0.433333333333334,
0.45,0.466666666666667,0.483333333333333,0.5,0.516666666666667,0.533333333333333,
0.55,0.566666666666667,0.583333333333333,0.6,0.616666666666667,0.633333333333333,
0.65,0.666666666666667,0.683333333333333,0.7,0.716666666666667,0.733333333333333,
0.75,0.766666666666667,0.783333333333333,0.8,0.816666666666667,0.833333333333333,
0.85,0.866666666666667,0.883333333333333,0.9,0.916666666666667,0.933333333333333,
0.95,0.966666666666667,0.983333333333333,1.),.UNSPECIFIED.)
GEOMETRIC_REPRESENTATION_ITEM()
RATIONAL_B_SPLINE_SURFACE(((1.,0.866025403784439,1.,0.866025403784439,1.,
0.866025403784439,1.,0.866025403784439,1.,0.866025403784439,1.,0.866025403784439,
1.,0.866025403784439,1.,0.866025403784439,1.,0.866025403784439,1.,0.866025403784439,
1.,0.866025403784439,1.,0.866025403784439,1.,0.866025403784439,1.,0.866025403784439,
1.,0.866025403784439,1.,0.866025403784439,1.,0.866025403784439,1.,0.866025403784439,
1.,0.866025403784439,1.,0.866025403784439,1.,0.866025403784439,1.,0.866025403784439,
1.,0.866025403784439,1.,0.866025403784439,1.,0.866025403784439,1.,0.866025403784439,
1.,0.866025403784439,1.,0.866025403784439,1.,0.866025403784439,1.,0.866025403784439,
1.,0.866025403784439,1.,0.866025403784439,1.,0.866025403784439,1.,0.866025403784439,
1.,0.866025403784439,1.,0.866025403784439,1.,0.866025403784439,1.,0.866025403784439,
1.,0.866025403784439,1.,0.866025403784439,1.,0.866025403784439,1.,0.866025403784439,
1.,0.866025403784439,1.,0.866025403784439,1.,0.866025403784439,1.,0.866025403784439,
1.,0.866025403784439,1.,0.866025403784439,1.,0.866025403784439,1.,0.866025403784439,
1.,0.866025403784439,1.,0.866025403784439,1.,0.866025403784439,1.,0.866025403784439,
1.,0.866025403784439,1.,0.866025403784439,1.,0.866025403784439,1.,0.866025403784439,
1.,0.866025403784439,1.,0.866025403784439,1.),(0.333333333333334,0.288675134594813,
0.333333333333334,0.288675134594813,0.333333333333334,0.288675134594813,
0.333333333333334,0.288675134594813,0.333333333333334,0.288675134594813,
0.333333333333334,0.288675134594813,0.333333333333334,0.288675134594813,
0.333333333333334,0.288675134594813,0.333333333333334,0.288675134594813,
0.333333333333334,0.288675134594813,0.333333333333334,0.288675134594813,
0.333333333333334,0.288675134594813,0.333333333333334,0.288675134594813,
0.333333333333334,0.288675134594813,0.333333333333334,0.288675134594813,
0.333333333333334,0.288675134594813,0.333333333333334,0.288675134594813,
0.333333333333334,0.288675134594813,0.333333333333334,0.288675134594813,
0.333333333333334,0.288675134594813,0.333333333333334,0.288675134594813,
0.333333333333334,0.288675134594813,0.333333333333334,0.288675134594813,
0.333333333333334,0.288675134594813,0.333333333333334,0.288675134594813,
0.333333333333334,0.288675134594813,0.333333333333334,0.288675134594813,
0.333333333333334,0.288675134594813,0.333333333333334,0.288675134594813,
0.333333333333334,0.288675134594813,0.333333333333334,0.288675134594813,
0.333333333333334,0.288675134594813,0.333333333333334,0.288675134594813,
0.333333333333334,0.288675134594813,0.333333333333334,0.288675134594813,
0.333333333333334,0.288675134594813,0.333333333333334,0.288675134594813,
0.333333333333334,0.288675134594813,0.333333333333334,0.288675134594813,
0.333333333333334,0.288675134594813,0.333333333333334,0.288675134594813,
0.333333333333334,0.288675134594813,0.333333333333334,0.288675134594813,
0.333333333333334,0.288675134594813,0.333333333333334,0.288675134594813,
0.333333333333334,0.288675134594813,0.333333333333334,0.288675134594813,
0.333333333333334,0.288675134594813,0.333333333333334,0.288675134594813,
0.333333333333334,0.288675134594813,0.333333333333334,0.288675134594813,
0.333333333333334,0.288675134594813,0.333333333333334,0.288675134594813,
0.333333333333334,0.288675134594813,0.333333333333334,0.288675134594813,
0.333333333333334,0.288675134594813,0.333333333333334,0.288675134594813,
0.333333333333334,0.288675134594813,0.333333333333334,0.288675134594813,
0.333333333333334,0.288675134594813,0.333333333333334),(0.333333333333334,
0.288675134594813,0.333333333333334,0.288675134594813,0.333333333333334,
0.288675134594813,0.333333333333334,0.288675134594813,0.333333333333334,
0.288675134594813,0.333333333333334,0.288675134594813,0.333333333333334,
0.288675134594813,0.333333333333334,0.288675134594813,0.333333333333334,
0.288675134594813,0.333333333333334,0.288675134594813,0.333333333333334,
0.288675134594813,0.333333333333334,0.288675134594813,0.333333333333334,
0.288675134594813,0.333333333333334,0.288675134594813,0.333333333333334,
0.288675134594813,0.333333333333334,0.288675134594813,0.333333333333334,
0.288675134594813,0.333333333333334,0.288675134594813,0.333333333333334,
0.288675134594813,0.333333333333334,0.288675134594813,0.333333333333334,
0.288675134594813,0.333333333333334,0.288675134594813,0.333333333333334,
0.288675134594813,0.333333333333334,0.288675134594813,0.333333333333334,
0.288675134594813,0.333333333333334,0.288675134594813,0.333333333333334,
0.288675134594813,0.333333333333334,0.288675134594813,0.333333333333334,
0.288675134594813,0.333333333333334,0.288675134594813,0.333333333333334,
0.288675134594813,0.333333333333334,0.288675134594813,0.333333333333334,
0.288675134594813,0.333333333333334,0.288675134594813,0.333333333333334,
0.288675134594813,0.333333333333334,0.288675134594813,0.333333333333334,
0.288675134594813,0.333333333333334,0.288675134594813,0.333333333333334,
0.288675134594813,0.333333333333334,0.288675134594813,0.333333333333334,
0.288675134594813,0.333333333333334,0.288675134594813,0.333333333333334,
0.288675134594813,0.333333333333334,0.288675134594813,0.333333333333334,
0.288675134594813,0.333333333333334,0.288675134594813,0.333333333333334,
0.288675134594813,0.333333333333334,0.288675134594813,0.333333333333334,
0.288675134594813,0.333333333333334,0.288675134594813,0.333333333333334,
0.288675134594813,0.333333333333334,0.288675134594813,0.333333333333334,
0.288675134594813,0.333333333333334,0.288675134594813,0.333333333333334,
0.288675134594813,0.333333333333334,0.288675134594813,0.333333333333334,
0.288675134594813,0.333333333333334,0.288675134594813,0.333333333333334,
0.288675134594813,0.333333333333334,0.288675134594813,0.333333333333334),
(1.,0.866025403784439,1.,0.866025403784439,1.,0.866025403784439,1.,0.866025403784439,
1.,0.866025403784439,1.,0.866025403784439,1.,0.866025403784439,1.,0.866025403784439,
1.,0.866025403784439,1.,0.866025403784439,1.,0.866025403784439,1.,0.866025403784439,
1.,0.866025403784439,1.,0.866025403784439,1.,0.866025403784439,1.,0.866025403784439,
1.,0.866025403784439,1.,0.866025403784439,1.,0.866025403784439,1.,0.866025403784439,
1.,0.866025403784439,1.,0.866025403784439,1.,0.866025403784439,1.,0.866025403784439,
1.,0.866025403784439,1.,0.866025403784439,1.,0.866025403784439,1.,0.866025403784439,
1.,0.866025403784439,1.,0.866025403784439,1.,0.866025403784439,1.,0.866025403784439,
1.,0.866025403784439,1.,0.866025403784439,1.,0.866025403784439,1.,0.866025403784439,
1.,0.866025403784439,1.,0.866025403784439,1.,0.866025403784439,1.,0.866025403784439,
1.,0.866025403784439,1.,0.866025403784439,1.,0.866025403784439,1.,0.866025403784439,
1.,0.866025403784439,1.,0.866025403784439,1.,0.866025403784439,1.,0.866025403784439,
1.,0.866025403784439,1.,0.866025403784439,1.,0.866025403784439,1.,0.866025403784439,
1.,0.866025403784439,1.,0.866025403784439,1.,0.866025403784439,1.,0.866025403784439,
1.,0.866025403784439,1.,0.866025403784439,1.,0.866025403784439,1.,0.866025403784439,
1.),(0.333333333333334,0.288675134594813,0.333333333333334,0.288675134594813,
0.333333333333334,0.288675134594813,0.333333333333334,0.288675134594813,
0.333333333333334,0.288675134594813,0.333333333333334,0.288675134594813,
0.333333333333334,0.288675134594813,0.333333333333334,0.288675134594813,
0.333333333333334,0.288675134594813,0.333333333333334,0.288675134594813,
0.333333333333334,0.288675134594813,0.333333333333334,0.288675134594813,
0.333333333333334,0.288675134594813,0.333333333333334,0.288675134594813,
0.333333333333334,0.288675134594813,0.333333333333334,0.288675134594813,
0.333333333333334,0.288675134594813,0.333333333333334,0.288675134594813,
0.333333333333334,0.288675134594813,0.333333333333334,0.288675134594813,
0.333333333333334,0.288675134594813,0.333333333333334,0.288675134594813,
0.333333333333334,0.288675134594813,0.333333333333334,0.288675134594813,
0.333333333333334,0.288675134594813,0.333333333333334,0.288675134594813,
0.333333333333334,0.288675134594813,0.333333333333334,0.288675134594813,
0.333333333333334,0.288675134594813,0.333333333333334,0.288675134594813,
0.333333333333334,0.288675134594813,0.333333333333334,0.288675134594813,
0.333333333333334,0.288675134594813,0.333333333333334,0.288675134594813,
0.333333333333334,0.288675134594813,0.333333333333334,0.288675134594813,
0.333333333333334,0.288675134594813,0.333333333333334,0.288675134594813,
0.333333333333334,0.288675134594813,0.333333333333334,0.288675134594813,
0.333333333333334,0.288675134594813,0.333333333333334,0.288675134594813,
0.333333333333334,0.288675134594813,0.333333333333334,0.288675134594813,
0.333333333333334,0.288675134594813,0.333333333333334,0.288675134594813,
0.333333333333334,0.288675134594813,0.333333333333334,0.288675134594813,
0.333333333333334,0.288675134594813,0.333333333333334,0.288675134594813,
0.333333333333334,0.288675134594813,0.333333333333334,0.288675134594813,
0.333333333333334,0.288675134594813,0.333333333333334,0.288675134594813,
0.333333333333334,0.288675134594813,0.333333333333334,0.288675134594813,
0.333333333333334,0.288675134594813,0.333333333333334,0.288675134594813,
0.333333333333334,0.288675134594813,0.333333333333334,0.288675134594813,
0.333333333333334),(0.333333333333334,0.288675134594813,0.333333333333334,
0.288675134594813,0.333333333333334,0.288675134594813,0.333333333333334,
0.288675134594813,0.333333333333334,0.288675134594813,0.333333333333334,
0.288675134594813,0.333333333333334,0.288675134594813,0.333333333333334,
0.288675134594813,0.333333333333334,0.288675134594813,0.333333333333334,
0.288675134594813,0.333333333333334,0.288675134594813,0.333333333333334,
0.288675134594813,0.333333333333334,0.288675134594813,0.333333333333334,
0.288675134594813,0.333333333333334,0.288675134594813,0.333333333333334,
0.288675134594813,0.333333333333334,0.288675134594813,0.333333333333334,
0.288675134594813,0.333333333333334,0.288675134594813,0.333333333333334,
0.288675134594813,0.333333333333334,0.288675134594813,0.333333333333334,
0.288675134594813,0.333333333333334,0.288675134594813,0.333333333333334,
0.288675134594813,0.333333333333334,0.288675134594813,0.333333333333334,
0.288675134594813,0.333333333333334,0.288675134594813,0.333333333333334,
0.288675134594813,0.333333333333334,0.288675134594813,0.333333333333334,
0.288675134594813,0.333333333333334,0.288675134594813,0.333333333333334,
0.288675134594813,0.333333333333334,0.288675134594813,0.333333333333334,
0.288675134594813,0.333333333333334,0.288675134594813,0.333333333333334,
0.288675134594813,0.333333333333334,0.288675134594813,0.333333333333334,
0.288675134594813,0.333333333333334,0.288675134594813,0.333333333333334,
0.288675134594813,0.333333333333334,0.288675134594813,0.333333333333334,
0.288675134594813,0.333333333333334,0.288675134594813,0.333333333333334,
0.288675134594813,0.333333333333334,0.288675134594813,0.333333333333334,
0.288675134594813,0.333333333333334,0.288675134594813,0.333333333333334,
0.288675134594813,0.333333333333334,0.288675134594813,0.333333333333334,
0.288675134594813,0.333333333333334,0.288675134594813,0.333333333333334,
0.288675134594813,0.333333333333334,0.288675134594813,0.333333333333334,
0.288675134594813,0.333333333333334,0.288675134594813,0.333333333333334,
0.288675134594813,0.333333333333334,0.288675134594813,0.333333333333334,
0.288675134594813,0.333333333333334,0.288675134594813,0.333333333333334,
0.288675134594813,0.333333333333334),(1.,0.866025403784439,1.,0.866025403784439,
1.,0.866025403784439,1.,0.866025403784439,1.,0.866025403784439,1.,0.866025403784439,
1.,0.866025403784439,1.,0.866025403784439,1.,0.866025403784439,1.,0.866025403784439,
1.,0.866025403784439,1.,0.866025403784439,1.,0.866025403784439,1.,0.866025403784439,
1.,0.866025403784439,1.,0.866025403784439,1.,0.866025403784439,1.,0.866025403784439,
1.,0.866025403784439,1.,0.866025403784439,1.,0.866025403784439,1.,0.866025403784439,
1.,0.866025403784439,1.,0.866025403784439,1.,0.866025403784439,1.,0.866025403784439,
1.,0.866025403784439,1.,0.866025403784439,1.,0.866025403784439,1.,0.866025403784439,
1.,0.866025403784439,1.,0.866025403784439,1.,0.866025403784439,1.,0.866025403784439,
1.,0.866025403784439,1.,0.866025403784439,1.,0.866025403784439,1.,0.866025403784439,
1.,0.866025403784439,1.,0.866025403784439,1.,0.866025403784439,1.,0.866025403784439,
1.,0.866025403784439,1.,0.866025403784439,1.,0.866025403784439,1.,0.866025403784439,
1.,0.866025403784439,1.,0.866025403784439,1.,0.866025403784439,1.,0.866025403784439,
1.,0.866025403784439,1.,0.866025403784439,1.,0.866025403784439,1.,0.866025403784439,
1.,0.866025403784439,1.,0.866025403784439,1.,0.866025403784439,1.,0.866025403784439,
1.,0.866025403784439,1.,0.866025403784439,1.)))
REPRESENTATION_ITEM('')
SURFACE()
);
#155=(
BOUNDED_SURFACE()
B_SPLINE_SURFACE(3,2,((#41507,#41508,#41509),(#41510,#41511,#41512),(#41513,
#41514,#41515),(#41516,#41517,#41518),(#41519,#41520,#41521),(#41522,#41523,
#41524),(#41525,#41526,#41527),(#41528,#41529,#41530),(#41531,#41532,#41533),
(#41534,#41535,#41536),(#41537,#41538,#41539),(#41540,#41541,#41542),(#41543,
#41544,#41545),(#41546,#41547,#41548),(#41549,#41550,#41551),(#41552,#41553,
#41554),(#41555,#41556,#41557),(#41558,#41559,#41560),(#41561,#41562,#41563),
(#41564,#41565,#41566),(#41567,#41568,#41569),(#41570,#41571,#41572),(#41573,
#41574,#41575),(#41576,#41577,#41578),(#41579,#41580,#41581),(#41582,#41583,
#41584),(#41585,#41586,#41587),(#41588,#41589,#41590),(#41591,#41592,#41593),
(#41594,#41595,#41596),(#41597,#41598,#41599),(#41600,#41601,#41602),(#41603,
#41604,#41605),(#41606,#41607,#41608),(#41609,#41610,#41611),(#41612,#41613,
#41614),(#41615,#41616,#41617),(#41618,#41619,#41620),(#41621,#41622,#41623),
(#41624,#41625,#41626),(#41627,#41628,#41629),(#41630,#41631,#41632)),
 .UNSPECIFIED.,.F.,.F.,.F.)
B_SPLINE_SURFACE_WITH_KNOTS((4,2,2,2,2,2,2,2,2,2,2,2,2,2,2,2,2,2,2,2,4),
(3,3),(-0.000180428912156006,0.164606365078715,0.329212730157431,0.493819095236146,
0.658425460314861,0.823031825393576,0.987638190472292,1.15224455555101,
1.31685092062972,1.48145728570844,1.64606365078715,1.81067001586587,1.97527638094458,
2.05757956348394,2.1398827460233,2.22218592856266,2.30448911110201,2.38679229364137,
2.46909547618073,2.55139865872009,2.63370184125944),(-0.000180428912158174,
1.),.UNSPECIFIED.)
GEOMETRIC_REPRESENTATION_ITEM()
RATIONAL_B_SPLINE_SURFACE(((1.00002747362388,0.923865794144028,1.),(1.00002747283797,
0.923867972041735,1.),(1.00002778507159,0.923002718203409,1.),(1.00002903107801,
0.919549816980654,1.),(1.00002996427325,0.916963770134614,1.),(1.00003244208062,
0.910097333539332,1.),(1.00003398669916,0.905816926024921,1.),(1.00003767113923,
0.895606699673117,1.),(1.00003981097144,0.889676851216917,1.),(1.00004466281745,
0.876231539283259,1.),(1.00004737484772,0.868716030175813,1.),(1.0000533408798,
0.852183114223139,1.),(1.00005659490622,0.843165639185358,1.),(1.00006360694908,
0.823734044835397,1.),(1.00006736500184,0.813319824861043,1.),(1.00007533847186,
0.791223948081428,1.),(1.00007955394243,0.779542143552474,1.),(1.00008838568606,
0.755067840834176,1.),(1.00009300203695,0.742275126983019,1.),(1.00010256714128,
0.715768553807505,1.),(1.00010751600729,0.702054382506394,1.),(1.00011766312963,
0.673934935852508,1.),(1.00012286154571,0.659529217785071,1.),(1.00013340615476,
0.630308266094241,1.),(1.00013875256542,0.615492429246126,1.),(1.0001467886769,
0.593222962028068,1.),(1.00014946992156,0.585792765217129,1.),(1.00015481886695,
0.570969904149657,1.),(1.0001574865782,0.563577210768261,1.),(1.00016278762071,
0.548887096965589,1.),(1.00016542096244,0.541589647514159,1.),(1.00017062993481,
0.527154676129277,1.),(1.00017320557466,0.520017128655486,1.),(1.00017827307841,
0.505974191505765,1.),(1.00018076494827,0.499068785290728,1.),(1.00018563594977,
0.485570390172216,1.),(1.00018801508117,0.4789774019006,1.),(1.00019262873255,
0.466192168865366,1.),(1.00019486324215,0.459999952835799,1.),(1.00019915310735,
0.448111987809573,1.),(1.00020120841379,0.442416375004484,1.),(1.00020315589889,
0.437019553957336,1.)))
REPRESENTATION_ITEM('')
SURFACE()
);
#156=(
BOUNDED_SURFACE()
B_SPLINE_SURFACE(3,2,((#41656,#41657,#41658),(#41659,#41660,#41661),(#41662,
#41663,#41664),(#41665,#41666,#41667),(#41668,#41669,#41670),(#41671,#41672,
#41673),(#41674,#41675,#41676),(#41677,#41678,#41679),(#41680,#41681,#41682),
(#41683,#41684,#41685),(#41686,#41687,#41688),(#41689,#41690,#41691),(#41692,
#41693,#41694),(#41695,#41696,#41697),(#41698,#41699,#41700),(#41701,#41702,
#41703),(#41704,#41705,#41706),(#41707,#41708,#41709),(#41710,#41711,#41712),
(#41713,#41714,#41715),(#41716,#41717,#41718),(#41719,#41720,#41721),(#41722,
#41723,#41724),(#41725,#41726,#41727),(#41728,#41729,#41730),(#41731,#41732,
#41733),(#41734,#41735,#41736),(#41737,#41738,#41739),(#41740,#41741,#41742),
(#41743,#41744,#41745),(#41746,#41747,#41748),(#41749,#41750,#41751),(#41752,
#41753,#41754),(#41755,#41756,#41757),(#41758,#41759,#41760),(#41761,#41762,
#41763),(#41764,#41765,#41766),(#41767,#41768,#41769),(#41770,#41771,#41772),
(#41773,#41774,#41775),(#41776,#41777,#41778),(#41779,#41780,#41781),(#41782,
#41783,#41784),(#41785,#41786,#41787),(#41788,#41789,#41790),(#41791,#41792,
#41793),(#41794,#41795,#41796),(#41797,#41798,#41799)),.UNSPECIFIED.,.F.,
 .F.,.F.)
B_SPLINE_SURFACE_WITH_KNOTS((4,2,2,2,2,2,2,2,2,2,2,2,2,2,2,2,2,2,2,2,2,
2,2,4),(3,3),(0.00405715139965717,0.0042139480393906,0.00432957425184741,
0.00435848080496162,0.00438738735807582,0.00444520046430423,0.00456082667676104,
0.00458973322987524,0.00461863978298944,0.00467645288921785,0.00479207910167466,
0.00484989220790306,0.00490770531413147,0.00502333152658828,0.00513895773904509,
0.00516786429215929,0.0051967708452735,0.0052545839515019,0.00537021016395871,
0.00548583637641552,0.00560146258887234,0.00565927569510074,0.00571708880132915,
0.00594834122624277),(0.,1.00004117042728),.UNSPECIFIED.)
GEOMETRIC_REPRESENTATION_ITEM()
RATIONAL_B_SPLINE_SURFACE(((1.,0.921979058456473,1.000006424311),(1.,0.924596675875849,
1.00000620877414),(1.,0.926417326016543,1.00000605886026),(1.,0.92821880541024,
1.0000059105249),(1.,0.928558002582939,1.00000588259512),(1.,0.928433280614718,
1.00000589286483),(1.,0.928380610460445,1.00000589720174),(1.,0.928221595227939,
1.00000591029519),(1.,0.92811523092253,1.00000591905332),(1.,0.927717554191574,
1.00000595179836),(1.,0.927347749203701,1.00000598224842),(1.,0.925936429317906,
1.0000060984577),(1.,0.924594290701714,1.00000620897054),(1.,0.922434222240346,
1.00000638683242),(1.,0.921976988327732,1.00000642448146),(1.,0.921020155283146,
1.00000650326791),(1.,0.920520634377084,1.00000654439888),(1.,0.918960875377281,
1.00000667283077),(1.,0.917839524509904,1.00000676516376),(1.,0.914244283327225,
1.00000706119899),(1.,0.911540219248417,1.00000728385394),(1.,0.90705432648433,
1.00000765322618),(1.,0.905483610646325,1.00000778256027),(1.,0.902242131132709,
1.00000804946646),(1.,0.900567342069336,1.00000818737002),(1.,0.895389495139947,
1.00000861371837),(1.,0.891733580942485,1.00000891474946),(1.,0.884041048555298,
1.00000954815915),(1.,0.880004227665733,1.00000988055444),(1.,0.874725766434696,
1.00001031518745),(1.,0.87365841541306,1.00001040307404),(1.,0.871500398344183,
1.00001058076701),(1.,0.870409954167221,1.00001067055512),(1.,0.867119949574412,
1.0000109414569),(1.,0.864896413773187,1.00001112454474),(1.,0.858136741898467,
1.0000116811419),(1.,0.853511773742965,1.00001206196573),(1.,0.844026400946148,
1.00001284299943),(1.,0.839165945656301,1.00001324321348),(1.,0.829204144361192,
1.00001406347671),(1.,0.824102781547739,1.00001448352728),(1.,0.816261555954164,
1.0000151291805),(1.,0.813616239468941,1.00001534699812),(1.,0.80826050162453,
1.00001578799415),(1.,0.805555387411647,1.00001601073556),(1.,0.791956355880912,
1.00001713049144),(1.,0.780780298581849,1.00001805073755),(1.,0.769254523194895,
1.00001899977974)))
REPRESENTATION_ITEM('')
SURFACE()
);
#157=(
BOUNDED_SURFACE()
B_SPLINE_SURFACE(3,2,((#42035,#42036,#42037),(#42038,#42039,#42040),(#42041,
#42042,#42043),(#42044,#42045,#42046),(#42047,#42048,#42049),(#42050,#42051,
#42052),(#42053,#42054,#42055),(#42056,#42057,#42058),(#42059,#42060,#42061),
(#42062,#42063,#42064),(#42065,#42066,#42067),(#42068,#42069,#42070),(#42071,
#42072,#42073),(#42074,#42075,#42076),(#42077,#42078,#42079),(#42080,#42081,
#42082),(#42083,#42084,#42085),(#42086,#42087,#42088),(#42089,#42090,#42091),
(#42092,#42093,#42094),(#42095,#42096,#42097),(#42098,#42099,#42100),(#42101,
#42102,#42103),(#42104,#42105,#42106),(#42107,#42108,#42109),(#42110,#42111,
#42112),(#42113,#42114,#42115),(#42116,#42117,#42118),(#42119,#42120,#42121),
(#42122,#42123,#42124),(#42125,#42126,#42127),(#42128,#42129,#42130),(#42131,
#42132,#42133),(#42134,#42135,#42136),(#42137,#42138,#42139),(#42140,#42141,
#42142),(#42143,#42144,#42145),(#42146,#42147,#42148),(#42149,#42150,#42151),
(#42152,#42153,#42154),(#42155,#42156,#42157),(#42158,#42159,#42160),(#42161,
#42162,#42163),(#42164,#42165,#42166),(#42167,#42168,#42169),(#42170,#42171,
#42172),(#42173,#42174,#42175),(#42176,#42177,#42178),(#42179,#42180,#42181),
(#42182,#42183,#42184),(#42185,#42186,#42187),(#42188,#42189,#42190),(#42191,
#42192,#42193),(#42194,#42195,#42196),(#42197,#42198,#42199),(#42200,#42201,
#42202),(#42203,#42204,#42205),(#42206,#42207,#42208),(#42209,#42210,#42211),
(#42212,#42213,#42214),(#42215,#42216,#42217),(#42218,#42219,#42220),(#42221,
#42222,#42223),(#42224,#42225,#42226),(#42227,#42228,#42229),(#42230,#42231,
#42232)),.UNSPECIFIED.,.F.,.F.,.F.)
B_SPLINE_SURFACE_WITH_KNOTS((4,2,2,2,2,2,2,2,2,2,2,2,2,2,2,2,2,2,2,2,2,
2,2,2,2,2,2,2,2,2,2,2,4),(3,3),(4.7123634827097,4.84407407244766,4.97575916451063,
5.10744425657361,5.23912934863658,5.37081444069955,5.50249953276252,5.63418462482549,
5.76586971688847,5.89755480895144,6.02923990101441,6.16092499307738,6.29261008514036,
6.42429517720333,6.5559802692663,6.68766536132927,6.81935045339224,6.95103554545522,
7.08272063751819,7.21440572958116,7.34609082164413,7.4777759137071,7.60946100577008,
7.74114609783305,7.87283118989602,8.00451628195899,8.13620137402197,8.26788646608494,
8.39957155814791,8.53125665021088,8.66294174227385,8.79462683433682,8.9263119263998),
(-2.54976749745779E-5,1.0000200211984),.UNSPECIFIED.)
GEOMETRIC_REPRESENTATION_ITEM()
RATIONAL_B_SPLINE_SURFACE(((1.00001493677863,0.707089416884705,1.00001172854274),
(1.00001458276126,0.714031705927214,1.00001145056393),(1.0000142339983,
0.72087095578393,1.00001117671096),(1.00001355192398,0.734246449476047,
1.00001064113779),(1.00001321861735,0.740782600388391,1.00001037942132),
(1.00001257176904,0.753467310976227,1.00000987150805),(1.00001225822607,
0.759615896089341,1.00000962531024),(1.00001165474721,0.771450130927326,
1.0000091514512),(1.0000113648101,0.777135804508549,1.00000892378901),(1.00001081189245,
0.787978532648321,1.00000848963125),(1.00001054891083,0.793135608462434,
1.00000828313484),(1.00001005279086,0.802864532786016,1.00000789357533),
(1.00000981965159,0.80743639954397,1.00000771051149),(1.00000938566623,
0.815946862742293,1.00000736974084),(1.00000918481937,0.819885474363816,
1.00000721203341),(1.00000881745384,0.827089521022162,1.00000692357347),
(1.00000865093455,0.8303549682861,1.00000679282047),(1.00000835386198,0.836180568468688,
1.00000655955542),(1.00000822330822,0.838740730840915,1.000006457043),(1.00000799942127,
0.843131159125162,1.00000628124421),(1.00000790608774,0.844961431902458,
1.00000620795757),(1.00000775752295,0.847874791033107,1.00000609130266),
(1.00000770229146,0.848957881819088,1.00000604793422),(1.00000763044669,
0.850366759396511,1.00000599152082),(1.00000761383331,0.850692548296484,
1.00000597847579),(1.00000761937903,0.850583796497954,1.00000598283036),
(1.00000764153815,0.850149255637501,1.00000600022997),(1.00000772442274,
0.848523886858095,1.00000606531197),(1.00000778514834,0.847333056502543,
1.00000611299446),(1.00000794459767,0.844206251360263,1.00000623819604),
(1.00000804332165,0.842270271800573,1.00000631571532),(1.00000827783294,
0.837671499782725,1.00000649985648),(1.00000841362062,0.8350087000993,1.00000660647865),
(1.00000872095034,0.828981956938996,1.00000684779773),(1.00000889249289,
0.825618003623282,1.00000698249505),(1.00000926963831,0.818222172985636,
1.00000727863429),(1.00000947524183,0.814190283024086,1.00000744007671),
(1.00000991841571,0.805499632828679,1.0000077880623),(1.00001015598685,
0.800840856978932,1.00000797460609),(1.00001066058466,0.79094568201105,
1.00000837082251),(1.00001092761227,0.785709264204444,1.00000858049589),
(1.00001148817145,0.774716685456562,1.00000902065386),(1.00001178170412,
0.768960502851546,1.00000925113933),(1.00001239185506,0.756995428492058,
1.00000973023737),(1.00001270847456,0.750786512573754,1.00000997885091),
(1.00001336088375,0.737992752755806,1.00001049113065),(1.00001369667475,
0.73140788332834,1.00001075479788),(1.00001438298174,0.717949387037515,
1.00001129369459),(1.00001473349899,0.711075735492579,1.00001156892506),
(1.00001544425076,0.697137876382458,1.00001212701611),(1.0000158044863,
0.690073648827045,1.0000124098775),(1.00001652907635,0.675864420871923,
1.00001297883454),(1.00001689343131,0.668719411333768,1.00001326493055),
(1.0000176200554,0.654470295700902,1.00001383548474),(1.00001798232397,
0.647366200462238,1.00001411994249),(1.00001869797199,0.633332325987409,
1.00001468187813),(1.00001905134922,0.626402590046828,1.0000149593543),
(1.00001974186121,0.612861633591743,1.00001550155282),(1.00002007899133,
0.606250503907858,1.00001576627155),(1.00002072921578,0.593499586974255,
1.00001627683581),(1.00002104230228,0.587359953302464,1.00001652267519),
(1.00002163640176,0.57570964848589,1.00001698916942),(1.00002191740319,
0.570199203714092,1.00001720981521),(1.00002243935165,0.55996378210997,
1.00001761965557),(1.00002268029487,0.555238879860998,1.00001780884716),
(1.00002289743305,0.550980794913776,1.00001797934674)))
REPRESENTATION_ITEM('')
SURFACE()
);
#158=(
BOUNDED_SURFACE()
B_SPLINE_SURFACE(3,2,((#42415,#42416,#42417),(#42418,#42419,#42420),(#42421,
#42422,#42423),(#42424,#42425,#42426),(#42427,#42428,#42429),(#42430,#42431,
#42432),(#42433,#42434,#42435),(#42436,#42437,#42438),(#42439,#42440,#42441),
(#42442,#42443,#42444),(#42445,#42446,#42447),(#42448,#42449,#42450),(#42451,
#42452,#42453),(#42454,#42455,#42456),(#42457,#42458,#42459),(#42460,#42461,
#42462),(#42463,#42464,#42465),(#42466,#42467,#42468),(#42469,#42470,#42471),
(#42472,#42473,#42474),(#42475,#42476,#42477),(#42478,#42479,#42480),(#42481,
#42482,#42483),(#42484,#42485,#42486),(#42487,#42488,#42489),(#42490,#42491,
#42492),(#42493,#42494,#42495),(#42496,#42497,#42498),(#42499,#42500,#42501),
(#42502,#42503,#42504),(#42505,#42506,#42507),(#42508,#42509,#42510),(#42511,
#42512,#42513),(#42514,#42515,#42516)),.UNSPECIFIED.,.F.,.F.,.F.)
B_SPLINE_SURFACE_WITH_KNOTS((4,2,2,2,2,2,2,2,2,2,2,2,2,2,2,2,4),(3,3),(1.55194677087336,
1.74947440896781,1.94700204706227,2.14452968515673,2.34205732325119,2.53958496134565,
2.73711259944011,2.93464023753456,3.13216787562902,3.32969551372348,3.52722315181794,
3.7247507899124,3.92227842800686,4.11980606610132,4.31733370419577,4.51486134229023,
4.71238898038469),(-2.42766963556483E-5,1.),.UNSPECIFIED.)
GEOMETRIC_REPRESENTATION_ITEM()
RATIONAL_B_SPLINE_SURFACE(((1.00001436631327,0.704113091369118,1.),(1.00001385873323,
0.714567150498244,1.),(1.00001336171142,0.724803753602056,1.),(1.0000124041668,
0.744525230800647,1.),(1.00001194367891,0.754009385402698,1.),(1.00001107227999,
0.771956615694544,1.),(1.00001066136108,0.780419853575295,1.),(1.00000989969439,
0.796107051746786,1.),(1.00000954894,0.803331148053762,1.),(1.00000891601262,
0.816366846433687,1.),(1.00000863383454,0.822178553085928,1.),(1.0000081444562,
0.832257732352426,1.),(1.00000793725231,0.836525279419831,1.),(1.00000760233045,
0.843423290914308,1.),(1.00000747461017,0.846053802860064,1.),(1.00000730136028,
0.849622037199957,1.),(1.00000725582954,0.850559783059377,1.),(1.0000072479093,
0.850722907291969,1.),(1.00000728551976,0.849948286719655,1.),(1.00000744309521,
0.846702881275639,1.),(1.00000756306123,0.844232075124759,1.),(1.00000788280972,
0.837646572592139,1.),(1.00000808259438,0.833531831096325,1.),(1.0000085576446,
0.823747752192612,1.),(1.00000883291365,0.818078343045833,1.),(1.00000945271828,
0.805312919420194,1.),(1.00000979725879,0.798216803347918,1.),(1.00001054739183,
0.782767151031959,1.),(1.00001095299081,0.774413481699587,1.),(1.00001181486088,
0.756662506520888,1.),(1.00001227113974,0.747265040418406,1.),(1.00001322161599,
0.727689142842311,1.),(1.00001371577882,0.717511422999973,1.),(1.00001422130471,
0.707099670706811,1.)))
REPRESENTATION_ITEM('')
SURFACE()
);
#159=(
BOUNDED_SURFACE()
B_SPLINE_SURFACE(3,2,((#42564,#42565,#42566),(#42567,#42568,#42569),(#42570,
#42571,#42572),(#42573,#42574,#42575),(#42576,#42577,#42578),(#42579,#42580,
#42581),(#42582,#42583,#42584),(#42585,#42586,#42587),(#42588,#42589,#42590),
(#42591,#42592,#42593),(#42594,#42595,#42596),(#42597,#42598,#42599),(#42600,
#42601,#42602),(#42603,#42604,#42605),(#42606,#42607,#42608),(#42609,#42610,
#42611),(#42612,#42613,#42614),(#42615,#42616,#42617),(#42618,#42619,#42620),
(#42621,#42622,#42623),(#42624,#42625,#42626),(#42627,#42628,#42629),(#42630,
#42631,#42632),(#42633,#42634,#42635),(#42636,#42637,#42638),(#42639,#42640,
#42641)),.UNSPECIFIED.,.F.,.F.,.F.)
B_SPLINE_SURFACE_WITH_KNOTS((4,2,2,2,2,2,2,2,2,2,2,2,4),(3,3),(-8.02309607639273E-18,
0.000231201308553261,0.00046240261710653,0.000578003271383164,0.000635803598521482,
0.000693603925659799,0.000924805234213068,0.00115600654276634,0.00138720785131961,
0.00150280850559624,0.00156060883273456,0.00161840915987287,0.00184961046842614),
(0.,1.),.UNSPECIFIED.)
GEOMETRIC_REPRESENTATION_ITEM()
RATIONAL_B_SPLINE_SURFACE(((1.,0.707106781186546,1.),(1.,0.720929919393816,
1.),(1.,0.734604162805705,1.),(1.,0.761404742811728,1.),(1.,0.774530928339215,
1.),(1.,0.793676981797689,1.),(1.,0.799968971951391,1.),(1.,0.809258992556117,
1.),(1.,0.812331025452392,1.),(1.,0.818423859772064,1.),(1.,0.821445484452913,
1.),(1.,0.836344837847268,1.),(1.,0.847660204338874,1.),(1.,0.869100951414214,
1.),(1.,0.879226501171938,1.),(1.,0.898300415096302,1.),(1.,0.907248884122996,
1.),(1.,0.919790865749779,1.),(1.,0.923824653174569,1.),(1.,0.929654417556856,
1.),(1.,0.931560846523734,1.),(1.,0.935299871240406,1.),(1.,0.937133447719843,
1.),(1.,0.946081718428858,1.),(1.,0.952565822325163,1.),(1.,0.95841150296378,
1.)))
REPRESENTATION_ITEM('')
SURFACE()
);
#160=(
BOUNDED_SURFACE()
B_SPLINE_SURFACE(3,2,((#42685,#42686,#42687),(#42688,#42689,#42690),(#42691,
#42692,#42693),(#42694,#42695,#42696),(#42697,#42698,#42699),(#42700,#42701,
#42702),(#42703,#42704,#42705),(#42706,#42707,#42708),(#42709,#42710,#42711),
(#42712,#42713,#42714),(#42715,#42716,#42717),(#42718,#42719,#42720),(#42721,
#42722,#42723),(#42724,#42725,#42726),(#42727,#42728,#42729),(#42730,#42731,
#42732),(#42733,#42734,#42735),(#42736,#42737,#42738),(#42739,#42740,#42741),
(#42742,#42743,#42744),(#42745,#42746,#42747),(#42748,#42749,#42750),(#42751,
#42752,#42753),(#42754,#42755,#42756),(#42757,#42758,#42759),(#42760,#42761,
#42762)),.UNSPECIFIED.,.F.,.F.,.F.)
B_SPLINE_SURFACE_WITH_KNOTS((4,2,2,2,2,2,2,2,2,2,2,2,4),(3,3),(2.4611389315421E-17,
0.000231201308553273,0.000462402617106521,0.000578003271383145,0.000635803598521457,
0.000693603925659769,0.000924805234213017,0.00115600654276626,0.00138720785131951,
0.00150280850559614,0.00156060883273445,0.00161840915987276,0.00184961046842601),
(0.,1.),.UNSPECIFIED.)
GEOMETRIC_REPRESENTATION_ITEM()
RATIONAL_B_SPLINE_SURFACE(((1.,0.707106781186553,1.),(1.,0.720929919393856,
1.),(1.,0.734604162805657,1.),(1.,0.76140474281178,1.),(1.,0.774530928339167,
1.),(1.,0.79367698179771,1.),(1.,0.799968971951349,1.),(1.,0.809258992556132,
1.),(1.,0.812331025452404,1.),(1.,0.818423859772045,1.),(1.,0.821445484452912,
1.),(1.,0.836344837847255,1.),(1.,0.847660204338855,1.),(1.,0.869100951414219,
1.),(1.,0.879226501171922,1.),(1.,0.898300415096301,1.),(1.,0.907248884123008,
1.),(1.,0.919790865749757,1.),(1.,0.923824653174548,1.),(1.,0.929654417556854,
1.),(1.,0.931560846523727,1.),(1.,0.935299871240392,1.),(1.,0.937133447719837,
1.),(1.,0.946081718428836,1.),(1.,0.952565822325914,1.),(1.,0.958411502963771,
1.)))
REPRESENTATION_ITEM('')
SURFACE()
);
#161=(
BOUNDED_SURFACE()
B_SPLINE_SURFACE(3,2,((#42989,#42990,#42991),(#42992,#42993,#42994),(#42995,
#42996,#42997),(#42998,#42999,#43000),(#43001,#43002,#43003),(#43004,#43005,
#43006),(#43007,#43008,#43009),(#43010,#43011,#43012),(#43013,#43014,#43015),
(#43016,#43017,#43018),(#43019,#43020,#43021),(#43022,#43023,#43024),(#43025,
#43026,#43027),(#43028,#43029,#43030),(#43031,#43032,#43033),(#43034,#43035,
#43036),(#43037,#43038,#43039),(#43040,#43041,#43042),(#43043,#43044,#43045),
(#43046,#43047,#43048),(#43049,#43050,#43051),(#43052,#43053,#43054),(#43055,
#43056,#43057),(#43058,#43059,#43060),(#43061,#43062,#43063),(#43064,#43065,
#43066),(#43067,#43068,#43069),(#43070,#43071,#43072),(#43073,#43074,#43075),
(#43076,#43077,#43078),(#43079,#43080,#43081),(#43082,#43083,#43084),(#43085,
#43086,#43087),(#43088,#43089,#43090),(#43091,#43092,#43093),(#43094,#43095,
#43096),(#43097,#43098,#43099),(#43100,#43101,#43102),(#43103,#43104,#43105),
(#43106,#43107,#43108),(#43109,#43110,#43111),(#43112,#43113,#43114)),
 .UNSPECIFIED.,.F.,.F.,.F.)
B_SPLINE_SURFACE_WITH_KNOTS((4,2,2,2,2,2,2,2,2,2,2,2,2,2,2,2,2,2,2,2,4),
(3,3),(-1.14925430283463E-17,0.000184433511101772,0.000368867022203556,
0.000553300533305339,0.000645517288856231,0.000691625666631677,0.000737734044407122,
0.000922167555508906,0.00110660106661069,0.00147546808881426,0.00156768484436515,
0.00161379322214059,0.00165990159991604,0.00184433511101782,0.00221320213322139,
0.00258206915542496,0.00276650266652674,0.00285871942207763,0.00290482779985308,
0.0029278819887408,0.00295093617762852),(0.,1.),.UNSPECIFIED.)
GEOMETRIC_REPRESENTATION_ITEM()
RATIONAL_B_SPLINE_SURFACE(((1.,0.707106781186548,1.),(1.,0.718133109232454,
1.),(1.,0.729066449118189,1.),(1.,0.750613820444198,1.),(1.,0.761227677789341,
1.),(1.,0.782035992265971,1.),(1.,0.792230829853422,1.),(1.,0.807152370816259,
1.),(1.,0.812064584782534,1.),(1.,0.819334468682991,1.),(1.,0.821740098050387,
1.),(1.,0.826498417096085,1.),(1.,0.828853542546963,1.),(1.,0.840509377458955,
1.),(1.,0.849450761297905,1.),(1.,0.866576104208724,1.),(1.,0.874760117668752,
1.),(1.,0.898186376934544,1.),(1.,0.912305286226077,1.),(1.,0.928084784593313,
1.),(1.,0.931147041015764,1.),(1.,0.935599437228533,1.),(1.,0.937060508010849,
1.),(1.,0.939926548778915,1.),(1.,0.941332681223158,1.),(1.,0.948230522590508,
1.),(1.,0.953324197247602,1.),(1.,0.967382764235203,1.),(1.,0.975129434277988,
1.),(1.,0.987528841798518,1.),(1.,0.992181040796599,1.),(1.,0.996857896678297,
1.),(1.,0.998032308863382,1.),(1.,0.999210733877751,1.),(1.,0.999506280906549,
1.),(1.,0.999802327869022,1.),(1.,0.999876460522184,1.),(1.,0.99995062376894,
1.),(1.,0.999969172009759,1.),(1.,0.999993884192384,1.),(1.,1.00000001991537,
1.),(1.,1.,1.)))
REPRESENTATION_ITEM('')
SURFACE()
);
#162=(
BOUNDED_SURFACE()
B_SPLINE_SURFACE(3,2,((#43231,#43232,#43233),(#43234,#43235,#43236),(#43237,
#43238,#43239),(#43240,#43241,#43242),(#43243,#43244,#43245),(#43246,#43247,
#43248),(#43249,#43250,#43251),(#43252,#43253,#43254),(#43255,#43256,#43257),
(#43258,#43259,#43260),(#43261,#43262,#43263),(#43264,#43265,#43266),(#43267,
#43268,#43269),(#43270,#43271,#43272),(#43273,#43274,#43275),(#43276,#43277,
#43278),(#43279,#43280,#43281),(#43282,#43283,#43284)),.UNSPECIFIED.,.F.,
 .F.,.F.)
B_SPLINE_SURFACE_WITH_KNOTS((4,2,2,2,2,2,2,2,4),(3,3),(-0.000256146907527732,
0.196349540849362,0.392699081698724,0.589048622548086,0.785398163397448,
0.98174770424681,1.17809724509617,1.37444678594553,1.57105247370244),(0.,
1.00025614690754),.UNSPECIFIED.)
GEOMETRIC_REPRESENTATION_ITEM()
RATIONAL_B_SPLINE_SURFACE(((0.999999999999999,0.923860025992052,1.00003900603776),
(1.,0.92386380976833,1.00003900409936),(1.,0.922631950619233,1.00003963517318),
(1.,0.917721587618823,1.00004215072178),(1.,0.914045686726666,1.00004403386307),
(1.,0.904303507747054,1.00004902472111),(1.,0.898237178126564,1.00005213246425),
(1.,0.883805658263611,1.00005952564262),(1.,0.875440377644158,1.00006381112414),
(1.,0.856541795567702,1.00007349275085),(1.,0.846008345896188,1.00007888897197),
(1.,0.822947010606607,1.00009070315141),(1.,0.810418887616988,1.00009712123133),
(1.,0.783590096545192,1.00011086545506),(1.,0.769289052220745,1.00011819179162),
(1.,0.739173873609776,1.00013361961136),(1.,0.723358473879048,1.00014172174282),
(1.,0.706967696454818,1.00015011863672)))
REPRESENTATION_ITEM('')
SURFACE()
);
#163=(
BOUNDED_SURFACE()
B_SPLINE_SURFACE(3,2,((#43297,#43298,#43299),(#43300,#43301,#43302),(#43303,
#43304,#43305),(#43306,#43307,#43308),(#43309,#43310,#43311),(#43312,#43313,
#43314),(#43315,#43316,#43317),(#43318,#43319,#43320),(#43321,#43322,#43323),
(#43324,#43325,#43326),(#43327,#43328,#43329),(#43330,#43331,#43332),(#43333,
#43334,#43335),(#43336,#43337,#43338),(#43339,#43340,#43341),(#43342,#43343,
#43344),(#43345,#43346,#43347),(#43348,#43349,#43350)),.UNSPECIFIED.,.F.,
 .F.,.F.)
B_SPLINE_SURFACE_WITH_KNOTS((4,2,2,2,2,2,2,2,4),(3,3),(1.57060699273548,
1.76832396488935,1.96585160298381,2.16337924107827,2.36090687917273,2.55843451726719,
2.75596215536165,2.9534897934561,3.15101743155056),(0.,1.00018933405942),
 .UNSPECIFIED.)
GEOMETRIC_REPRESENTATION_ITEM()
RATIONAL_B_SPLINE_SURFACE(((1.,0.707003978702482,1.00011094825221),(1.,
0.72348593060803,1.00010470706249),(1.,0.739385892154352,1.00009868625396),
(1.,0.769656517851604,1.00008722373307),(1.,0.784027936045077,1.00008178173518),
(1.,0.8109731743871,1.00007157843247),(1.,0.823547380016532,1.00006681698167),
(1.,0.84667338193124,1.00005805990203),(1.,0.857225420695959,1.00005406418136),
(1.,0.876131519789516,1.00004690504439),(1.,0.884485731030333,1.00004374157093),
(1.,0.898864213201865,1.00003829689813),(1.,0.904888575770995,1.00003601566409),
(1.,0.914515552682844,1.00003237023486),(1.,0.91811821889335,1.00003100602002),
(1.,0.922848120955148,1.0000292149569),(1.,0.923975956543124,1.00002878788152),
(1.,0.923856620627319,1.00002883307023)))
REPRESENTATION_ITEM('')
SURFACE()
);
#164=(
BOUNDED_SURFACE()
B_SPLINE_SURFACE(3,2,((#43550,#43551,#43552),(#43553,#43554,#43555),(#43556,
#43557,#43558),(#43559,#43560,#43561),(#43562,#43563,#43564),(#43565,#43566,
#43567),(#43568,#43569,#43570),(#43571,#43572,#43573),(#43574,#43575,#43576),
(#43577,#43578,#43579),(#43580,#43581,#43582),(#43583,#43584,#43585),(#43586,
#43587,#43588),(#43589,#43590,#43591),(#43592,#43593,#43594),(#43595,#43596,
#43597),(#43598,#43599,#43600),(#43601,#43602,#43603),(#43604,#43605,#43606),
(#43607,#43608,#43609),(#43610,#43611,#43612),(#43613,#43614,#43615),(#43616,
#43617,#43618),(#43619,#43620,#43621),(#43622,#43623,#43624),(#43625,#43626,
#43627),(#43628,#43629,#43630),(#43631,#43632,#43633),(#43634,#43635,#43636),
(#43637,#43638,#43639),(#43640,#43641,#43642),(#43643,#43644,#43645),(#43646,
#43647,#43648),(#43649,#43650,#43651),(#43652,#43653,#43654),(#43655,#43656,
#43657),(#43658,#43659,#43660),(#43661,#43662,#43663),(#43664,#43665,#43666),
(#43667,#43668,#43669),(#43670,#43671,#43672),(#43673,#43674,#43675),(#43676,
#43677,#43678),(#43679,#43680,#43681),(#43682,#43683,#43684),(#43685,#43686,
#43687),(#43688,#43689,#43690),(#43691,#43692,#43693),(#43694,#43695,#43696),
(#43697,#43698,#43699),(#43700,#43701,#43702),(#43703,#43704,#43705),(#43706,
#43707,#43708),(#43709,#43710,#43711),(#43712,#43713,#43714),(#43715,#43716,
#43717),(#43718,#43719,#43720),(#43721,#43722,#43723),(#43724,#43725,#43726),
(#43727,#43728,#43729)),.UNSPECIFIED.,.F.,.F.,.F.)
B_SPLINE_SURFACE_WITH_KNOTS((4,2,2,2,2,2,2,2,2,2,2,2,2,2,2,2,2,2,2,2,2,
2,2,2,2,2,2,2,2,4),(3,3),(0.00356026658290825,0.00370761548845134,0.00385496439399443,
0.00400231329953753,0.0040391505259233,0.00407598775230907,0.00414966220508062,
0.00429701111062371,0.0044443600161668,0.00451803446893835,0.00455487169532412,
0.00459170892170989,0.00473905782725299,0.00488640673279608,0.00492324395918185,
0.00496008118556762,0.00503375563833917,0.00510743009111072,0.00514426731749649,
0.00516268593068938,0.00518110454388226,0.00532845344942535,0.0054021279021969,
0.00543896512858267,0.00547580235496845,0.00562315126051154,0.00565998848689731,
0.00569682571328309,0.00577050016605463,0.00591784907159772),(0.,1.),
 .UNSPECIFIED.)
GEOMETRIC_REPRESENTATION_ITEM()
RATIONAL_B_SPLINE_SURFACE(((1.,0.707106781186547,1.),(1.,0.714899530141188,
1.),(1.,0.722851116139554,1.),(1.,0.738965796907419,1.),(1.,0.747128767269762,
1.),(1.,0.763573562645999,1.),(1.,0.771855539406454,1.),(1.,0.782231613637912,
1.),(1.,0.784308029863662,1.),(1.,0.788462064530618,1.),(1.,0.790542242277229,
1.),(1.,0.796763962116366,1.),(1.,0.800876179008829,1.),(1.,0.813095262016546,
1.),(1.,0.821084755433325,1.),(1.,0.836691228945864,1.),(1.,0.844308581612572,
1.),(1.,0.855403320496569,1.),(1.,0.859046240981785,1.),(1.,0.864419493162934,
1.),(1.,0.86619721499557,1.),(1.,0.869701088492385,1.),(1.,0.871429334319563,
1.),(1.,0.879949489101844,1.),(1.,0.886380304852135,1.),(1.,0.898373764602034,
1.),(1.,0.903938066040975,1.),(1.,0.910243055457683,1.),(1.,0.911466373703979,
1.),(1.,0.913826788251488,1.),(1.,0.914965304917439,1.),(1.,0.918252475084136,
1.),(1.,0.920272999106784,1.),(1.,0.92394925395352,1.),(1.,0.925605070562256,
1.),(1.,0.927791488596373,1.),(1.,0.928470669980879,1.),(1.,0.929411224851904,
1.),(1.,0.929711916737623,1.),(1.,0.930283108179015,1.),(1.,0.930554076458367,
1.),(1.,0.932861253750851,1.),(1.,0.933980898903266,1.),(1.,0.934229809753535,
1.),(1.,0.934073575444518,1.),(1.,0.933468573302636,1.),(1.,0.933204148039385,
1.),(1.,0.932559198561778,1.),(1.,0.932178256466784,1.),(1.,0.929991263320291,
1.),(1.,0.927343365860572,1.),(1.,0.923016139346013,1.),(1.,0.922097237767011,
1.),(1.,0.920176288887714,1.),(1.,0.919173225434103,1.),(1.,0.91604297106036,
1.),(1.,0.913794973536961,1.),(1.,0.906609692179916,1.),(1.,0.901232273200219,
1.),(1.,0.895342042385736,1.)))
REPRESENTATION_ITEM('')
SURFACE()
);
#165=(
BOUNDED_SURFACE()
B_SPLINE_SURFACE(3,2,((#43985,#43986,#43987),(#43988,#43989,#43990),(#43991,
#43992,#43993),(#43994,#43995,#43996),(#43997,#43998,#43999),(#44000,#44001,
#44002),(#44003,#44004,#44005),(#44006,#44007,#44008),(#44009,#44010,#44011),
(#44012,#44013,#44014),(#44015,#44016,#44017),(#44018,#44019,#44020),(#44021,
#44022,#44023),(#44024,#44025,#44026),(#44027,#44028,#44029),(#44030,#44031,
#44032),(#44033,#44034,#44035),(#44036,#44037,#44038),(#44039,#44040,#44041),
(#44042,#44043,#44044),(#44045,#44046,#44047),(#44048,#44049,#44050),(#44051,
#44052,#44053),(#44054,#44055,#44056),(#44057,#44058,#44059),(#44060,#44061,
#44062),(#44063,#44064,#44065),(#44066,#44067,#44068),(#44069,#44070,#44071),
(#44072,#44073,#44074),(#44075,#44076,#44077),(#44078,#44079,#44080),(#44081,
#44082,#44083),(#44084,#44085,#44086),(#44087,#44088,#44089),(#44090,#44091,
#44092),(#44093,#44094,#44095),(#44096,#44097,#44098),(#44099,#44100,#44101),
(#44102,#44103,#44104),(#44105,#44106,#44107),(#44108,#44109,#44110),(#44111,
#44112,#44113),(#44114,#44115,#44116),(#44117,#44118,#44119),(#44120,#44121,
#44122),(#44123,#44124,#44125),(#44126,#44127,#44128)),.UNSPECIFIED.,.F.,
 .F.,.F.)
B_SPLINE_SURFACE_WITH_KNOTS((4,2,2,2,2,2,2,2,2,2,2,2,2,2,2,2,2,2,2,2,2,
2,2,4),(3,3),(-2.69186893279756E-5,0.000147491368261441,0.000294982736522876,
0.00044247410478431,0.000479346946849669,0.000516219788915028,0.000589965473045745,
0.00073745684130718,0.000884948209568615,0.000958693893699332,0.000995566735764691,
0.00103243957783005,0.00117993094609148,0.00132742231435292,0.00147491368261435,
0.00154865936674507,0.00162240505087579,0.00176989641913722,0.00191738778739866,
0.00199113347152937,0.00202800631359473,0.00206487915566009,0.00221237052392153,
0.00235986189218296),(0.,1.00002691868933),.UNSPECIFIED.)
GEOMETRIC_REPRESENTATION_ITEM()
RATIONAL_B_SPLINE_SURFACE(((1.,0.706934185382307,1.00001577789523),(1.,
0.707289966495766,1.00001575874091),(1.,0.707645413657456,1.00001573960457),
(1.,0.708300892599077,1.0000157043153),(1.,0.708601012305713,1.00001568815764),
(1.,0.709200732421921,1.00001565587028),(1.,0.709500333423245,1.00001563974055),
(1.,0.709874355785092,1.00001561960417),(1.,0.709949135907864,1.0000156155782),
(1.,0.710098641866628,1.00001560752919),(1.,0.710173473062381,1.00001560350048),
(1.,0.710396928789648,1.0000155914702),(1.,0.710544516885821,1.00001558352445),
(1.,0.710983142239652,1.00001555991001),(1.,0.711270053741346,1.00001554446345),
(1.,0.711832583115565,1.00001551417834),(1.,0.712108201699971,1.00001549933976),
(1.,0.712512623814919,1.00001547756673),(1.,0.712645926822463,1.00001547039005),
(1.,0.712843524542374,1.0000154597519),(1.,0.71290899741735,1.00001545622701),
(1.,0.713039137297051,1.00001544922063),(1.,0.713103803366072,1.00001544573917),
(1.,0.713423270431812,1.0000154285399),(1.,0.713667991894455,1.00001541536474),
(1.,0.714135658414077,1.0000153901868),(1.,0.714358602875164,1.00001537818406),
(1.,0.714781991002754,1.00001535538995),(1.,0.714982437280183,1.00001534459845),
(1.,0.715265182582933,1.00001532937618),(1.,0.715356610594333,1.00001532445394),
(1.,0.715531426705098,1.0000153150423),(1.,0.715615029916155,1.00001531054132),
(1.,0.715854496794294,1.00001529764905),(1.,0.715999041792887,1.00001528986713),
(1.,0.716257713229434,1.00001527594093),(1.,0.71637184060172,1.00001526979661),
(1.,0.716519464132329,1.00001526184895),(1.,0.716564737889815,1.00001525941153),
(1.,0.716626593197021,1.0000152560814),(1.,0.716646227239996,1.00001525502436),
(1.,0.716683289956507,1.000015253029),(1.,0.71670072325815,1.00001525209044),
(1.,0.716782447076519,1.00001524769064),(1.,0.716830443772986,1.00001524510662),
(1.,0.716892320380967,1.00001524177535),(1.,0.716906185847933,1.00001524102887),
(1.,0.71690292040473,1.00001524120467)))
REPRESENTATION_ITEM('')
SURFACE()
);
#166=(
BOUNDED_SURFACE()
B_SPLINE_SURFACE(3,2,((#44129,#44130,#44131),(#44132,#44133,#44134),(#44135,
#44136,#44137),(#44138,#44139,#44140),(#44141,#44142,#44143),(#44144,#44145,
#44146),(#44147,#44148,#44149),(#44150,#44151,#44152),(#44153,#44154,#44155),
(#44156,#44157,#44158),(#44159,#44160,#44161),(#44162,#44163,#44164),(#44165,
#44166,#44167),(#44168,#44169,#44170),(#44171,#44172,#44173),(#44174,#44175,
#44176),(#44177,#44178,#44179),(#44180,#44181,#44182),(#44183,#44184,#44185),
(#44186,#44187,#44188),(#44189,#44190,#44191),(#44192,#44193,#44194),(#44195,
#44196,#44197),(#44198,#44199,#44200),(#44201,#44202,#44203),(#44204,#44205,
#44206),(#44207,#44208,#44209),(#44210,#44211,#44212)),.UNSPECIFIED.,.F.,
 .F.,.F.)
B_SPLINE_SURFACE_WITH_KNOTS((4,2,2,2,2,2,2,2,2,2,2,2,2,4),(3,3),(0.00102826841024056,
0.00108136671720793,0.00113446502417531,0.00124066163811006,0.00134685825204482,
0.00145305486597957,0.00166544809384908,0.00187784132171859,0.00209023454958809,
0.0023026277774576,0.00251502100532711,0.00262121761926186,0.00267431592622924,
0.00272741423319662),(-0.00283459110010449,1.),.UNSPECIFIED.)
GEOMETRIC_REPRESENTATION_ITEM()
RATIONAL_B_SPLINE_SURFACE(((1.00166517176203,0.706276548675112,1.),(1.00163220101093,
0.712092334787547,1.),(1.00159961546054,0.717840174463587,1.),(1.00153520684576,
0.729201357172828,1.),(1.00150334087126,0.734822269214763,1.),(1.0014092038008,
0.751427322137522,1.),(1.00134853122035,0.762129497213199,1.),(1.00123109470163,
0.782844393043764,1.),(1.00117433210629,0.79285687691495,1.),(1.00106457774187,
0.812216699997259,1.),(1.00101158686358,0.821563882080632,1.),(1.00085819617163,
0.848620816667832,1.),(1.00076335541889,0.865349993715338,1.),(1.00058884175311,
0.896132857911678,1.),(1.00050918219483,0.910184189386343,1.),(1.00036597350955,
0.9354450965539,1.),(1.00030277669818,0.94659252649063,1.),(1.00019375601416,
0.96582293401015,1.),(1.00014793806965,0.97390486591732,1.),(1.00007430095644,
0.986893884547261,1.),(1.0000464877762,0.991799914951515,1.),(1.00001862499585,
0.996714694431725,1.),(1.00001164514357,0.997945886521746,1.),(1.00000466137374,
0.999177769636466,1.),(1.00000291429973,0.999485940011998,1.),(1.00000058402726,
0.999896982096644,1.),(1.00000000076916,0.999999864326373,1.),(1.,1.,1.)))
REPRESENTATION_ITEM('')
SURFACE()
);
#167=(
BOUNDED_SURFACE()
B_SPLINE_SURFACE(3,2,((#44276,#44277,#44278),(#44279,#44280,#44281),(#44282,
#44283,#44284),(#44285,#44286,#44287),(#44288,#44289,#44290),(#44291,#44292,
#44293),(#44294,#44295,#44296),(#44297,#44298,#44299),(#44300,#44301,#44302),
(#44303,#44304,#44305),(#44306,#44307,#44308),(#44309,#44310,#44311),(#44312,
#44313,#44314),(#44315,#44316,#44317),(#44318,#44319,#44320),(#44321,#44322,
#44323),(#44324,#44325,#44326),(#44327,#44328,#44329),(#44330,#44331,#44332),
(#44333,#44334,#44335),(#44336,#44337,#44338),(#44339,#44340,#44341),(#44342,
#44343,#44344),(#44345,#44346,#44347),(#44348,#44349,#44350),(#44351,#44352,
#44353),(#44354,#44355,#44356),(#44357,#44358,#44359)),.UNSPECIFIED.,.F.,
 .F.,.F.)
B_SPLINE_SURFACE_WITH_KNOTS((4,2,2,2,2,2,2,2,2,2,2,2,2,4),(3,3),(0.00102826841024098,
0.00108136671720835,0.00113446502417572,0.00124066163811045,0.00134685825204519,
0.00145305486597993,0.00166544809384941,0.00187784132171888,0.00209023454958836,
0.00230262777745784,0.00251502100532731,0.00262121761926205,0.00267431592622942,
0.00272741423319679),(0.,1.00283459127414),.UNSPECIFIED.)
GEOMETRIC_REPRESENTATION_ITEM()
RATIONAL_B_SPLINE_SURFACE(((1.,0.706276548624223,1.00166517186456),(1.,
0.712092334737677,1.00163220111142),(1.,0.717840174414683,1.00159961555903),
(1.,0.729201357125934,1.00153520694028),(1.,0.734822269168861,1.00150334096382),
(1.,0.75142732209438,1.00140920388756),(1.,0.762129497171982,1.00134853130338),
(1.,0.78284439300614,1.00123109477743),(1.,0.792856876879042,1.00117433217859),
(1.,0.812216699964743,1.00106457780742),(1.,0.821563882049743,1.00101158692587),
(1.,0.848620816641558,1.00085819622447),(1.,0.865349993692116,1.00076335546589),
(1.,0.89613285789359,1.00058884178937),(1.,0.9101841893708,1.00050918222618),
(1.,0.935445096542706,1.00036597353209),(1.,0.946592526481339,1.00030277671682),
(1.,0.965822934004271,1.00019375602609),(1.,0.973904865912868,1.00014793807876),
(1.,0.98689388454492,1.00007430096101),(1.,0.991799914950075,1.00004648777906),
(1.,0.996714694431167,1.000018624997),(1.,0.99794588652139,1.00001164514429),
(1.,0.999177769636325,1.00000466137403),(1.,0.999485940011916,1.00000291429991),
(1.,0.999896982096622,1.0000005840273),(1.,0.999999864326377,1.00000000076916),
(1.,1.,1.)))
REPRESENTATION_ITEM('')
SURFACE()
);
#168=(
BOUNDED_SURFACE()
B_SPLINE_SURFACE(3,2,((#50715,#50716,#50717),(#50718,#50719,#50720),(#50721,
#50722,#50723),(#50724,#50725,#50726),(#50727,#50728,#50729),(#50730,#50731,
#50732),(#50733,#50734,#50735),(#50736,#50737,#50738),(#50739,#50740,#50741),
(#50742,#50743,#50744),(#50745,#50746,#50747),(#50748,#50749,#50750),(#50751,
#50752,#50753),(#50754,#50755,#50756),(#50757,#50758,#50759),(#50760,#50761,
#50762),(#50763,#50764,#50765),(#50766,#50767,#50768),(#50769,#50770,#50771),
(#50772,#50773,#50774),(#50775,#50776,#50777),(#50778,#50779,#50780),(#50781,
#50782,#50783),(#50784,#50785,#50786),(#50787,#50788,#50789),(#50790,#50791,
#50792),(#50793,#50794,#50795),(#50796,#50797,#50798),(#50799,#50800,#50801),
(#50802,#50803,#50804),(#50805,#50806,#50807),(#50808,#50809,#50810),(#50811,
#50812,#50813),(#50814,#50815,#50816),(#50817,#50818,#50819),(#50820,#50821,
#50822),(#50823,#50824,#50825),(#50826,#50827,#50828),(#50829,#50830,#50831),
(#50832,#50833,#50834),(#50835,#50836,#50837),(#50838,#50839,#50840),(#50841,
#50842,#50843),(#50844,#50845,#50846),(#50847,#50848,#50849),(#50850,#50851,
#50852),(#50853,#50854,#50855),(#50856,#50857,#50858),(#50859,#50860,#50861),
(#50862,#50863,#50864),(#50865,#50866,#50867),(#50868,#50869,#50870),(#50871,
#50872,#50873),(#50874,#50875,#50876),(#50877,#50878,#50879),(#50880,#50881,
#50882),(#50883,#50884,#50885),(#50886,#50887,#50888),(#50889,#50890,#50891),
(#50892,#50893,#50894),(#50895,#50896,#50897),(#50898,#50899,#50900),(#50901,
#50902,#50903),(#50904,#50905,#50906),(#50907,#50908,#50909),(#50910,#50911,
#50912),(#50913,#50914,#50915),(#50916,#50917,#50918),(#50919,#50920,#50921),
(#50922,#50923,#50924),(#50925,#50926,#50927),(#50928,#50929,#50930),(#50931,
#50932,#50933),(#50934,#50935,#50936),(#50937,#50938,#50939),(#50940,#50941,
#50942),(#50943,#50944,#50945),(#50946,#50947,#50948),(#50949,#50950,#50951),
(#50952,#50953,#50954),(#50955,#50956,#50957),(#50958,#50959,#50960),(#50961,
#50962,#50963),(#50964,#50965,#50966),(#50967,#50968,#50969),(#50970,#50971,
#50972),(#50973,#50974,#50975),(#50976,#50977,#50978),(#50979,#50980,#50981),
(#50982,#50983,#50984),(#50985,#50986,#50987),(#50988,#50989,#50990),(#50991,
#50992,#50993),(#50994,#50995,#50996),(#50997,#50998,#50999),(#51000,#51001,
#51002),(#51003,#51004,#51005),(#51006,#51007,#51008),(#51009,#51010,#51011),
(#51012,#51013,#51014),(#51015,#51016,#51017),(#51018,#51019,#51020),(#51021,
#51022,#51023),(#51024,#51025,#51026),(#51027,#51028,#51029),(#51030,#51031,
#51032),(#51033,#51034,#51035),(#51036,#51037,#51038),(#51039,#51040,#51041),
(#51042,#51043,#51044),(#51045,#51046,#51047),(#51048,#51049,#51050),(#51051,
#51052,#51053),(#51054,#51055,#51056),(#51057,#51058,#51059),(#51060,#51061,
#51062),(#51063,#51064,#51065),(#51066,#51067,#51068),(#51069,#51070,#51071),
(#51072,#51073,#51074),(#51075,#51076,#51077),(#51078,#51079,#51080),(#51081,
#51082,#51083),(#51084,#51085,#51086),(#51087,#51088,#51089),(#51090,#51091,
#51092),(#51093,#51094,#51095),(#51096,#51097,#51098),(#51099,#51100,#51101),
(#51102,#51103,#51104),(#51105,#51106,#51107),(#51108,#51109,#51110),(#51111,
#51112,#51113),(#51114,#51115,#51116),(#51117,#51118,#51119),(#51120,#51121,
#51122),(#51123,#51124,#51125),(#51126,#51127,#51128),(#51129,#51130,#51131),
(#51132,#51133,#51134),(#51135,#51136,#51137),(#51138,#51139,#51140),(#51141,
#51142,#51143),(#51144,#51145,#51146),(#51147,#51148,#51149),(#51150,#51151,
#51152),(#51153,#51154,#51155),(#51156,#51157,#51158),(#51159,#51160,#51161),
(#51162,#51163,#51164),(#51165,#51166,#51167),(#51168,#51169,#51170),(#51171,
#51172,#51173),(#51174,#51175,#51176),(#51177,#51178,#51179),(#51180,#51181,
#51182),(#51183,#51184,#51185),(#51186,#51187,#51188),(#51189,#51190,#51191),
(#51192,#51193,#51194),(#51195,#51196,#51197),(#51198,#51199,#51200),(#51201,
#51202,#51203),(#51204,#51205,#51206),(#51207,#51208,#51209),(#51210,#51211,
#51212),(#51213,#51214,#51215),(#51216,#51217,#51218),(#51219,#51220,#51221),
(#51222,#51223,#51224),(#51225,#51226,#51227),(#51228,#51229,#51230),(#51231,
#51232,#51233),(#51234,#51235,#51236),(#51237,#51238,#51239),(#51240,#51241,
#51242),(#51243,#51244,#51245),(#51246,#51247,#51248),(#51249,#51250,#51251),
(#51252,#51253,#51254),(#51255,#51256,#51257),(#51258,#51259,#51260),(#51261,
#51262,#51263),(#51264,#51265,#51266),(#51267,#51268,#51269),(#51270,#51271,
#51272),(#51273,#51274,#51275),(#51276,#51277,#51278),(#51279,#51280,#51281),
(#51282,#51283,#51284),(#51285,#51286,#51287),(#51288,#51289,#51290),(#51291,
#51292,#51293),(#51294,#51295,#51296),(#51297,#51298,#51299),(#51300,#51301,
#51302),(#51303,#51304,#51305),(#51306,#51307,#51308),(#51309,#51310,#51311),
(#51312,#51313,#51314),(#51315,#51316,#51317),(#51318,#51319,#51320),(#51321,
#51322,#51323),(#51324,#51325,#51326),(#51327,#51328,#51329),(#51330,#51331,
#51332),(#51333,#51334,#51335),(#51336,#51337,#51338),(#51339,#51340,#51341),
(#51342,#51343,#51344),(#51345,#51346,#51347),(#51348,#51349,#51350),(#51351,
#51352,#51353),(#51354,#51355,#51356),(#51357,#51358,#51359),(#51360,#51361,
#51362),(#51363,#51364,#51365),(#51366,#51367,#51368),(#51369,#51370,#51371),
(#51372,#51373,#51374),(#51375,#51376,#51377),(#51378,#51379,#51380),(#51381,
#51382,#51383),(#51384,#51385,#51386),(#51387,#51388,#51389),(#51390,#51391,
#51392),(#51393,#51394,#51395),(#51396,#51397,#51398),(#51399,#51400,#51401),
(#51402,#51403,#51404),(#51405,#51406,#51407),(#51408,#51409,#51410),(#51411,
#51412,#51413),(#51414,#51415,#51416),(#51417,#51418,#51419),(#51420,#51421,
#51422),(#51423,#51424,#51425),(#51426,#51427,#51428),(#51429,#51430,#51431),
(#51432,#51433,#51434),(#51435,#51436,#51437),(#51438,#51439,#51440),(#51441,
#51442,#51443),(#51444,#51445,#51446),(#51447,#51448,#51449),(#51450,#51451,
#51452),(#51453,#51454,#51455),(#51456,#51457,#51458),(#51459,#51460,#51461),
(#51462,#51463,#51464),(#51465,#51466,#51467),(#51468,#51469,#51470),(#51471,
#51472,#51473),(#51474,#51475,#51476),(#51477,#51478,#51479),(#51480,#51481,
#51482),(#51483,#51484,#51485),(#51486,#51487,#51488),(#51489,#51490,#51491),
(#51492,#51493,#51494),(#51495,#51496,#51497),(#51498,#51499,#51500)),
 .UNSPECIFIED.,.T.,.F.,.F.)
B_SPLINE_SURFACE_WITH_KNOTS((4,2,2,2,2,2,2,2,2,2,2,2,2,2,2,2,2,2,2,2,2,
2,2,2,2,2,2,2,2,2,2,2,2,2,2,2,2,2,2,2,2,2,2,2,2,2,2,2,2,2,2,2,2,2,2,2,2,
2,2,2,2,2,2,2,2,2,2,2,2,2,2,2,2,2,2,2,2,2,2,2,2,2,2,2,2,2,2,2,2,2,2,2,2,
2,2,2,2,2,2,2,2,2,2,2,2,2,2,2,2,2,2,2,2,2,2,2,2,2,2,2,2,2,2,2,2,2,2,2,2,
2,4),(3,3),(0.,5.58974039156775E-5,0.000111794807831355,0.00022358961566271,
0.00044717923132542,0.000894358462650841,0.00178871692530168,0.00268307538795252,
0.00279487019578388,0.00290666500361523,0.00313025461927794,0.00357743385060336,
0.0044717923132542,0.00536615077590504,0.0054779455837364,0.00558974039156775,
0.00581333000723046,0.00626050923855589,0.00715486770120673,0.00804922616385757,
0.00827281577952028,0.00838461058735163,0.00849640539518299,0.00894358462650841,
0.00983794308915925,0.0107323015518101,0.0111794807831355,0.0114030703987982,
0.0115148652066296,0.0116266600144609,0.0125210184771118,0.0134153769397626,
0.013862556171088,0.0143097354024135,0.0145333250180762,0.0146451198259075,
0.0147569146337389,0.0152040938650643,0.0160984523277151,0.016992810790366,
0.0172164004060287,0.01732819521386,0.0174399900216914,0.0178871692530168,
0.0187815277156677,0.0196758861783185,0.0198994757939812,0.0201230654096439,
0.0205702446409693,0.0214646031036202,0.022358961566271,0.0228061407975964,
0.0230297304132591,0.0232533200289219,0.0241476784915727,0.0250420369542235,
0.0259363954168744,0.0261599850325371,0.0262717798403685,0.0263835746481998,
0.0268307538795252,0.0277251123421761,0.0286194708048269,0.0290666500361523,
0.029290239651815,0.0294020344596464,0.0295138292674777,0.0299610084988032,
0.0301845981144659,0.0302963929222972,0.0304081877301286,0.0313025461927794,
0.0321969046554303,0.0330912631180811,0.0332030579259125,0.0333148527337438,
0.0335384423494065,0.0339856215807319,0.0348799800433828,0.0357743385060336,
0.0359979281216963,0.0361097229295277,0.036221517737359,0.0366686969686845,
0.0375630554313353,0.0384574138939862,0.0389045931253116,0.0391281827409743,
0.0392399775488056,0.039351772356637,0.0402461308192878,0.0411404892819387,
0.0420348477445895,0.0424820269759149,0.0425938217837463,0.0427056165915777,
0.0429292062072404,0.0433763854385658,0.0438235646698912,0.044717923132542,
0.0451651023638675,0.0452768971716988,0.0453886919795302,0.0456122815951929,
0.0465066400578437,0.0474009985204946,0.04784817775182,0.0479599725596513,
0.0480717673674827,0.0482953569831454,0.0491897154457962,0.0500840739084471,
0.0505312531397725,0.0507548427554352,0.0508666375632666,0.0509784323710979,
0.0518727908337488,0.0527671492963996,0.0536615077590504,0.0538850973747132,
0.0539968921825445,0.0541086869903759,0.0545558662217013,0.0554502246843521,
0.056344583147003,0.0567917623783284,0.0570153519939911,0.0571271468018225,
0.0571830442057381,0.057210992907696,0.0572389416096538),(0.,1.),
 .UNSPECIFIED.)
GEOMETRIC_REPRESENTATION_ITEM()
RATIONAL_B_SPLINE_SURFACE(((1.,0.869037098890924,1.),(1.,0.869090662160833,
1.),(1.,0.869142132128297,1.),(1.,0.869241273997536,1.),(1.,0.869288882663707,
1.),(1.,0.869425835273797,1.),(1.,0.869509305917427,1.),(1.,0.869736328335375,
1.),(1.,0.869856492063896,1.),(1.,0.870124205131434,1.),(1.,0.870178998389397,
1.),(1.,0.869977707911342,1.),(1.,0.869356264735848,1.),(1.,0.867159523791841,
1.),(1.,0.865584183970151,1.),(1.,0.863281618119441,1.),(1.,0.86301835474559,
1.),(1.,0.862477312320675,1.),(1.,0.862200065545979,1.),(1.,0.861348450829986,
1.),(1.,0.860754210958995,1.),(1.,0.858894323573958,1.),(1.,0.857551540639133,
1.),(1.,0.853231873120265,1.),(1.,0.849963976579328,1.),(1.,0.8427337476379,
1.),(1.,0.838771159914112,1.),(1.,0.833964492549446,1.),(1.,0.83342564158097,
1.),(1.,0.832341102831786,1.),(1.,0.831795088875303,1.),(1.,0.83014615568217,
1.),(1.,0.829032346207458,1.),(1.,0.825650047625046,1.),(1.,0.823340697393356,
1.),(1.,0.816270214875414,1.),(1.,0.811366531889991,1.),(1.,0.801290493401484,
1.),(1.,0.796117786007922,1.),(1.,0.789558114002489,1.),(1.,0.788241524410975,
1.),(1.,0.786261176106014,1.),(1.,0.785600666410631,1.),(1.,0.784281253478811,
1.),(1.,0.783622032027989,1.),(1.,0.780329023537139,1.),(1.,0.777704514650253,
1.),(1.,0.76988692542286,1.),(1.,0.764749330047637,1.),(1.,0.75477051537079,
1.),(1.,0.749929030998746,1.),(1.,0.743012971461713,1.),(1.,0.740765474239869,
1.),(1.,0.73749827976927,1.),(1.,0.736426570328376,1.),(1.,0.734847329496033,
1.),(1.,0.734325595116705,1.),(1.,0.733292134556225,1.),(1.,0.732781563072735,
1.),(1.,0.728242967029025,1.),(1.,0.724610876621003,1.),(1.,0.718276943716503,
1.),(1.,0.715575135642169,1.),(1.,0.712312229125148,1.),(1.,0.711356200483893,
1.),(1.,0.709722323386846,1.),(1.,0.709044475655852,1.),(1.,0.708247344579823,
1.),(1.,0.708018238565296,1.),(1.,0.707730840005604,1.),(1.,0.707644376240716,
1.),(1.,0.707490608795043,1.),(1.,0.707423402545753,1.),(1.,0.707135559015692,
1.),(1.,0.707059523314824,1.),(1.,0.707285549205988,1.),(1.,0.708042221657254,
1.),(1.,0.710710092253751,1.),(1.,0.712621237041365,1.),(1.,0.715686665981657,
1.),(1.,0.716333543550958,1.),(1.,0.717353607349392,1.),(1.,0.717701919486094,
1.),(1.,0.718414964313171,1.),(1.,0.718779962361759,1.),(1.,0.720642167884513,
1.),(1.,0.722248110686464,1.),(1.,0.727379897082438,1.),(1.,0.731219242886661,
1.),(1.,0.739562059134817,1.),(1.,0.744065650037015,1.),(1.,0.750011006364496,
1.),(1.,0.751215898212902,1.),(1.,0.753654939425893,1.),(1.,0.754889413958793,
1.),(1.,0.758631191877784,1.),(1.,0.761160349547001,1.),(1.,0.768820010203822,
1.),(1.,0.774022074432147,1.),(1.,0.784467204631247,1.),(1.,0.789710609506525,
1.),(1.,0.797506397811445,1.),(1.,0.800093535602747,1.),(1.,0.803945021596591,
1.),(1.,0.805223982229172,1.),(1.,0.807770172561434,1.),(1.,0.80903292134295,
1.),(1.,0.815288089794111,1.),(1.,0.820107499923359,1.),(1.,0.829279685729609,
1.),(1.,0.833632779776828,1.),(1.,0.841777168809211,1.),(1.,0.845568802174027,
1.),(1.,0.849892563199079,1.),(1.,0.850736491533872,1.),(1.,0.851969804909359,
1.),(1.,0.852375793676684,1.),(1.,0.853174988795519,1.),(1.,0.853568068159912,
1.),(1.,0.855500704900974,1.),(1.,0.856941996550435,1.),(1.,0.860944601199298,
1.),(1.,0.863184927882986,1.),(1.,0.866767461005655,1.),(1.,0.868109793594765,
1.),(1.,0.869410481594525,1.),(1.,0.869725148569242,1.),(1.,0.870012890040282,
1.),(1.,0.870078086396283,1.),(1.,0.870128990964309,1.),(1.,0.870138141570321,
1.),(1.,0.870140676091054,1.),(1.,0.870134072965078,1.),(1.,0.870061808448095,
1.),(1.,0.869878426760649,1.),(1.,0.869416656440071,1.),(1.,0.869231611413219,
1.),(1.,0.868907522254946,1.),(1.,0.868791738615037,1.),(1.,0.868544686539316,
1.),(1.,0.868413337134317,1.),(1.,0.867163505604549,1.),(1.,0.865575442228637,
1.),(1.,0.861527724393334,1.),(1.,0.859067845844723,1.),(1.,0.853343564886148,
1.),(1.,0.850078971827717,1.),(1.,0.84598647975218,1.),(1.,0.845525923915504,
1.),(1.,0.844593252383724,1.),(1.,0.84412081177775,1.),(1.,0.842688930644052,
1.),(1.,0.841715504172781,1.),(1.,0.83874140215334,1.),(1.,0.836686926299113,
1.),(1.,0.830328826430023,1.),(1.,0.825830615536545,1.),(1.,0.816419106847222,
1.),(1.,0.81150547118942,1.),(1.,0.805169234170547,1.),(1.,0.803892294076685,
1.),(1.,0.801963643202623,1.),(1.,0.801318553163188,1.),(1.,0.800024181787751,
1.),(1.,0.799374551464301,1.),(1.,0.796123838581708,1.),(1.,0.793511112507122,
1.),(1.,0.785661232785625,1.),(1.,0.780412024366977,1.),(1.,0.770019050951368,
1.),(1.,0.76487497595969,1.),(1.,0.757351702086758,1.),(1.,0.754876228736365,
1.),(1.,0.751227350622943,1.),(1.,0.750021792912108,1.),(1.,0.748231675946372,
1.),(1.,0.747638007827609,1.),(1.,0.746457111568753,1.),(1.,0.745869506104255,
1.),(1.,0.740620037686994,1.),(1.,0.736256100649653,1.),(1.,0.728276221758877,
1.),(1.,0.724660242842317,1.),(1.,0.718324000111086,1.),(1.,0.715603718055959,
1.),(1.,0.712309706535428,1.),(1.,0.711342812014489,1.),(1.,0.710310353740139,
1.),(1.,0.710112755568336,1.),(1.,0.709736703375217,1.),(1.,0.709558069154282,
1.),(1.,0.709050371012769,1.),(1.,0.708749513760786,1.),(1.,0.70795992094024,
1.),(1.,0.707584199551303,1.),(1.,0.707134092959367,1.),(1.,0.70705970821773,
1.),(1.,0.707286843642986,1.),(1.,0.70803921126881,1.),(1.,0.710052147725902,
1.),(1.,0.710870383211632,1.),(1.,0.71207445357331,1.),(1.,0.712324328892365,
1.),(1.,0.712842122035176,1.),(1.,0.713110243316174,1.),(1.,0.713939993830723,
1.),(1.,0.714526359388936,1.),(1.,0.717617638747993,1.),(1.,0.720600584023788,
1.),(1.,0.727424242013839,1.),(1.,0.731264995819141,1.),(1.,0.737553652730096,
1.),(1.,0.739737848764794,1.),(1.,0.742566372039795,1.),(1.,0.74313699147918,
1.),(1.,0.744287770846871,1.),(1.,0.744868257643384,1.),(1.,0.746621209706891,
1.),(1.,0.747803690023989,1.),(1.,0.753778025133493,1.),(1.,0.758754654573864,
1.),(1.,0.768933369155768,1.),(1.,0.774135775395061,1.),(1.,0.781997810487323,
1.),(1.,0.784628358204622,1.),(1.,0.788575987637978,1.),(1.,0.789892170142193,
1.),(1.,0.791865311260895,1.),(1.,0.792522836387841,1.),(1.,0.793837245909085,
1.),(1.,0.794493861510745,1.),(1.,0.800385048001281,1.),(1.,0.80551453306944,
1.),(1.,0.815446188856963,1.),(1.,0.820248709446964,1.),(1.,0.829421742411055,
1.),(1.,0.833792601959078,1.),(1.,0.838919085477355,1.),(1.,0.839927506491091,
1.),(1.,0.841413476855047,1.),(1.,0.841904356336916,1.),(1.,0.842876996646255,
1.),(1.,0.843358860518912,1.),(1.,0.845737639832195,1.),(1.,0.847548776311049,
1.),(1.,0.852696372188048,1.),(1.,0.855747262756165,1.),(1.,0.861029201702321,
1.),(1.,0.863260436478246,1.),(1.,0.865941546711405,1.),(1.,0.86672419811369,
1.),(1.,0.867724144067475,1.),(1.,0.868028445735918,1.),(1.,0.868440362182281,
1.),(1.,0.868570244374482,1.),(1.,0.868753799883508,1.),(1.,0.868813107052922,
1.),(1.,0.868899233803952,1.),(1.,0.868927470387005,1.),(1.,0.868982996012711,
1.),(1.,0.86901031725597,1.),(1.,0.869037098890924,1.)))
REPRESENTATION_ITEM('')
SURFACE()
);
#169=(
BOUNDED_SURFACE()
B_SPLINE_SURFACE(3,2,((#52221,#52222,#52223),(#52224,#52225,#52226),(#52227,
#52228,#52229),(#52230,#52231,#52232),(#52233,#52234,#52235),(#52236,#52237,
#52238),(#52239,#52240,#52241),(#52242,#52243,#52244),(#52245,#52246,#52247),
(#52248,#52249,#52250),(#52251,#52252,#52253),(#52254,#52255,#52256),(#52257,
#52258,#52259),(#52260,#52261,#52262),(#52263,#52264,#52265),(#52266,#52267,
#52268),(#52269,#52270,#52271),(#52272,#52273,#52274),(#52275,#52276,#52277),
(#52278,#52279,#52280),(#52281,#52282,#52283),(#52284,#52285,#52286),(#52287,
#52288,#52289),(#52290,#52291,#52292),(#52293,#52294,#52295),(#52296,#52297,
#52298),(#52299,#52300,#52301),(#52302,#52303,#52304),(#52305,#52306,#52307),
(#52308,#52309,#52310),(#52311,#52312,#52313),(#52314,#52315,#52316),(#52317,
#52318,#52319),(#52320,#52321,#52322),(#52323,#52324,#52325),(#52326,#52327,
#52328),(#52329,#52330,#52331),(#52332,#52333,#52334),(#52335,#52336,#52337),
(#52338,#52339,#52340),(#52341,#52342,#52343),(#52344,#52345,#52346),(#52347,
#52348,#52349),(#52350,#52351,#52352),(#52353,#52354,#52355),(#52356,#52357,
#52358),(#52359,#52360,#52361),(#52362,#52363,#52364),(#52365,#52366,#52367),
(#52368,#52369,#52370),(#52371,#52372,#52373),(#52374,#52375,#52376),(#52377,
#52378,#52379),(#52380,#52381,#52382),(#52383,#52384,#52385),(#52386,#52387,
#52388),(#52389,#52390,#52391),(#52392,#52393,#52394),(#52395,#52396,#52397),
(#52398,#52399,#52400),(#52401,#52402,#52403),(#52404,#52405,#52406),(#52407,
#52408,#52409),(#52410,#52411,#52412),(#52413,#52414,#52415),(#52416,#52417,
#52418),(#52419,#52420,#52421),(#52422,#52423,#52424),(#52425,#52426,#52427),
(#52428,#52429,#52430),(#52431,#52432,#52433),(#52434,#52435,#52436),(#52437,
#52438,#52439),(#52440,#52441,#52442),(#52443,#52444,#52445),(#52446,#52447,
#52448),(#52449,#52450,#52451),(#52452,#52453,#52454),(#52455,#52456,#52457),
(#52458,#52459,#52460),(#52461,#52462,#52463),(#52464,#52465,#52466),(#52467,
#52468,#52469),(#52470,#52471,#52472),(#52473,#52474,#52475),(#52476,#52477,
#52478),(#52479,#52480,#52481),(#52482,#52483,#52484),(#52485,#52486,#52487),
(#52488,#52489,#52490),(#52491,#52492,#52493),(#52494,#52495,#52496),(#52497,
#52498,#52499),(#52500,#52501,#52502),(#52503,#52504,#52505),(#52506,#52507,
#52508),(#52509,#52510,#52511),(#52512,#52513,#52514),(#52515,#52516,#52517),
(#52518,#52519,#52520),(#52521,#52522,#52523),(#52524,#52525,#52526),(#52527,
#52528,#52529),(#52530,#52531,#52532),(#52533,#52534,#52535),(#52536,#52537,
#52538),(#52539,#52540,#52541),(#52542,#52543,#52544),(#52545,#52546,#52547),
(#52548,#52549,#52550),(#52551,#52552,#52553),(#52554,#52555,#52556),(#52557,
#52558,#52559),(#52560,#52561,#52562),(#52563,#52564,#52565),(#52566,#52567,
#52568),(#52569,#52570,#52571),(#52572,#52573,#52574),(#52575,#52576,#52577),
(#52578,#52579,#52580),(#52581,#52582,#52583),(#52584,#52585,#52586),(#52587,
#52588,#52589),(#52590,#52591,#52592),(#52593,#52594,#52595),(#52596,#52597,
#52598),(#52599,#52600,#52601),(#52602,#52603,#52604),(#52605,#52606,#52607),
(#52608,#52609,#52610),(#52611,#52612,#52613),(#52614,#52615,#52616),(#52617,
#52618,#52619),(#52620,#52621,#52622),(#52623,#52624,#52625),(#52626,#52627,
#52628),(#52629,#52630,#52631),(#52632,#52633,#52634),(#52635,#52636,#52637),
(#52638,#52639,#52640),(#52641,#52642,#52643),(#52644,#52645,#52646),(#52647,
#52648,#52649),(#52650,#52651,#52652),(#52653,#52654,#52655),(#52656,#52657,
#52658),(#52659,#52660,#52661),(#52662,#52663,#52664),(#52665,#52666,#52667),
(#52668,#52669,#52670),(#52671,#52672,#52673),(#52674,#52675,#52676),(#52677,
#52678,#52679),(#52680,#52681,#52682),(#52683,#52684,#52685),(#52686,#52687,
#52688),(#52689,#52690,#52691),(#52692,#52693,#52694),(#52695,#52696,#52697),
(#52698,#52699,#52700),(#52701,#52702,#52703),(#52704,#52705,#52706),(#52707,
#52708,#52709),(#52710,#52711,#52712),(#52713,#52714,#52715),(#52716,#52717,
#52718),(#52719,#52720,#52721),(#52722,#52723,#52724),(#52725,#52726,#52727),
(#52728,#52729,#52730),(#52731,#52732,#52733),(#52734,#52735,#52736),(#52737,
#52738,#52739),(#52740,#52741,#52742),(#52743,#52744,#52745),(#52746,#52747,
#52748),(#52749,#52750,#52751),(#52752,#52753,#52754),(#52755,#52756,#52757),
(#52758,#52759,#52760),(#52761,#52762,#52763),(#52764,#52765,#52766),(#52767,
#52768,#52769),(#52770,#52771,#52772),(#52773,#52774,#52775),(#52776,#52777,
#52778),(#52779,#52780,#52781),(#52782,#52783,#52784),(#52785,#52786,#52787),
(#52788,#52789,#52790),(#52791,#52792,#52793),(#52794,#52795,#52796),(#52797,
#52798,#52799),(#52800,#52801,#52802),(#52803,#52804,#52805),(#52806,#52807,
#52808),(#52809,#52810,#52811),(#52812,#52813,#52814),(#52815,#52816,#52817),
(#52818,#52819,#52820),(#52821,#52822,#52823),(#52824,#52825,#52826),(#52827,
#52828,#52829),(#52830,#52831,#52832),(#52833,#52834,#52835),(#52836,#52837,
#52838),(#52839,#52840,#52841),(#52842,#52843,#52844),(#52845,#52846,#52847),
(#52848,#52849,#52850),(#52851,#52852,#52853),(#52854,#52855,#52856),(#52857,
#52858,#52859),(#52860,#52861,#52862),(#52863,#52864,#52865),(#52866,#52867,
#52868),(#52869,#52870,#52871),(#52872,#52873,#52874),(#52875,#52876,#52877),
(#52878,#52879,#52880),(#52881,#52882,#52883),(#52884,#52885,#52886),(#52887,
#52888,#52889),(#52890,#52891,#52892),(#52893,#52894,#52895),(#52896,#52897,
#52898),(#52899,#52900,#52901),(#52902,#52903,#52904),(#52905,#52906,#52907),
(#52908,#52909,#52910),(#52911,#52912,#52913),(#52914,#52915,#52916),(#52917,
#52918,#52919),(#52920,#52921,#52922),(#52923,#52924,#52925),(#52926,#52927,
#52928),(#52929,#52930,#52931),(#52932,#52933,#52934),(#52935,#52936,#52937),
(#52938,#52939,#52940),(#52941,#52942,#52943),(#52944,#52945,#52946),(#52947,
#52948,#52949),(#52950,#52951,#52952),(#52953,#52954,#52955),(#52956,#52957,
#52958),(#52959,#52960,#52961),(#52962,#52963,#52964),(#52965,#52966,#52967),
(#52968,#52969,#52970),(#52971,#52972,#52973),(#52974,#52975,#52976),(#52977,
#52978,#52979),(#52980,#52981,#52982),(#52983,#52984,#52985),(#52986,#52987,
#52988),(#52989,#52990,#52991),(#52992,#52993,#52994),(#52995,#52996,#52997),
(#52998,#52999,#53000),(#53001,#53002,#53003),(#53004,#53005,#53006),(#53007,
#53008,#53009),(#53010,#53011,#53012),(#53013,#53014,#53015),(#53016,#53017,
#53018)),.UNSPECIFIED.,.T.,.F.,.F.)
B_SPLINE_SURFACE_WITH_KNOTS((4,2,2,2,2,2,2,2,2,2,2,2,2,2,2,2,2,2,2,2,2,
2,2,2,2,2,2,2,2,2,2,2,2,2,2,2,2,2,2,2,2,2,2,2,2,2,2,2,2,2,2,2,2,2,2,2,2,
2,2,2,2,2,2,2,2,2,2,2,2,2,2,2,2,2,2,2,2,2,2,2,2,2,2,2,2,2,2,2,2,2,2,2,2,
2,2,2,2,2,2,2,2,2,2,2,2,2,2,2,2,2,2,2,2,2,2,2,2,2,2,2,2,2,2,2,2,2,2,2,2,
2,2,2,4),(3,3),(0.,4.12881615541384E-5,8.25763231082768E-5,0.000165152646216554,
0.000330305292433107,0.000660610584866214,0.000990915877299321,0.00132122116973243,
0.00148637381594898,0.00156895013905726,0.00165152646216554,0.00198183175459864,
0.00264244233946486,0.00297274763189796,0.00313790027811452,0.00322047660122279,
0.00330305292433107,0.00396366350919728,0.0046242740940635,0.00495457938649661,
0.00503715570960488,0.00511973203271316,0.00528488467892971,0.00594549526379593,
0.00660610584866214,0.00693641114109525,0.00701898746420353,0.0071015637873118,
0.00726671643352836,0.00792732701839457,0.00858793760326078,0.009248548188127,
0.00990915877299321,0.0100743114192098,0.0102394640654263,0.0105697693578594,
0.0112303799427256,0.0118909905275919,0.0125516011124581,0.0132122116973243,
0.0138728222821905,0.0139553986052988,0.0140379749284071,0.0142031275746236,
0.0145334328670567,0.0151940434519229,0.0158546540367891,0.0165152646216554,
0.0166804172678719,0.0168455699140885,0.0171758752065216,0.0175061804989547,
0.0178364857913878,0.0181667910838209,0.0183319437300374,0.0184145200531457,
0.018497096376254,0.0188274016686871,0.0191577069611202,0.0194880122535533,
0.0196531648997699,0.0197357412228781,0.0198183175459864,0.0201486228384195,
0.0204789281308526,0.0208092334232857,0.020891809746394,0.0209743860695023,
0.0211395387157189,0.021469844008152,0.0215524203312602,0.0216349966543685,
0.0218001493005851,0.0221304545930182,0.0224607598854513,0.0227910651778844,
0.0231213704703175,0.0232039467934258,0.023286523116534,0.0234516757627506,
0.0237819810551837,0.0241122863476168,0.0244425916400499,0.0251032022249161,
0.0252683548711327,0.0254335075173492,0.0257638128097823,0.0264244233946486,
0.0270850339795148,0.027745644564381,0.0284062551492472,0.0285714077954638,
0.0287365604416803,0.0290668657341134,0.0297274763189796,0.0303880869038458,
0.0310486974887121,0.0317093080735783,0.0320396133660114,0.0322047660122279,
0.0323699186584445,0.0330305292433107,0.0336911398281769,0.0343517504130431,
0.0346820557054762,0.0348472083516928,0.0349297846748011,0.0350123609979093,
0.0356729715827756,0.0363335821676418,0.036994192752508,0.0370767690756163,
0.0371593453987245,0.0373244980449411,0.0376548033373742,0.0383154139222404,
0.0386457192146735,0.0388108718608901,0.0389760245071066,0.0396366350919728,
0.039966940384406,0.0402972456768391,0.0404623983230556,0.0405449746461639,
0.0406275509692722,0.0409578562617053,0.0412881615541384,0.0416184668465715,
0.0419487721390046,0.0421139247852211,0.0421965011083294,0.0422377892698836,
0.0422790774314377),(0.,1.),.UNSPECIFIED.)
GEOMETRIC_REPRESENTATION_ITEM()
RATIONAL_B_SPLINE_SURFACE(((1.,0.923590675042016,1.),(1.,0.923572320945391,
1.),(1.,0.923553587090577,1.),(1.,0.923515495478205,1.),(1.,0.923496115237016,
1.),(1.,0.923436971524286,1.),(1.,0.923396205307423,1.),(1.,0.923269889059141,
1.),(1.,0.923180325181551,1.),(1.,0.922895385428438,1.),(1.,0.922683818431749,
1.),(1.,0.922215055006499,1.),(1.,0.921957857869856,1.),(1.,0.921393597668949,
1.),(1.,0.921086537396165,1.),(1.,0.920583987620736,1.),(1.,0.920409463147971,
1.),(1.,0.920136456599823,1.),(1.,0.920043583473226,1.),(1.,0.919853965179493,
1.),(1.,0.919757130552995,1.),(1.,0.919264385051497,1.),(1.,0.918842556687909,
1.),(1.,0.917485342839882,1.),(1.,0.916458802712932,1.),(1.,0.914690614339645,
1.),(1.,0.914063012700798,1.),(1.,0.913057237216573,1.),(1.,0.912711240257362,
1.),(1.,0.912175163335873,1.),(1.,0.911993623483323,1.),(1.,0.911624678363091,
1.),(1.,0.911437120441042,1.),(1.,0.909726149783902,1.),(1.,0.908041888239718,
1.),(1.,0.904290424256204,1.),(1.,0.90222325436422,1.),(1.,0.898787650803265,
1.),(1.,0.897586580689637,1.),(1.,0.896009931734525,1.),(1.,0.895690686714278,
1.),(1.,0.895045201490737,1.),(1.,0.894719248531258,1.),(1.,0.893731649644609,
1.),(1.,0.893060263975502,1.),(1.,0.889636937842127,1.),(1.,0.886685904879282,
1.),(1.,0.880320125821774,1.),(1.,0.876905428959452,1.),(1.,0.871403913130991,
1.),(1.,0.869506798646649,1.),(1.,0.867052723787093,1.),(1.,0.866557553196408,
1.),(1.,0.865560870035344,1.),(1.,0.865059173595903,1.),(1.,0.863543964995002,
1.),(1.,0.862520333878055,1.),(1.,0.857333970909859,1.),(1.,0.852966736393177,
1.),(1.,0.843775067927313,1.),(1.,0.838950667880686,1.),(1.,0.828820205567495,
1.),(1.,0.823514183332928,1.),(1.,0.812391307349727,1.),(1.,0.806574504385483,
1.),(1.,0.798962220591142,1.),(1.,0.797421706068384,1.),(1.,0.794315888151595,
1.),(1.,0.792749600433445,1.),(1.,0.788010186024153,1.),(1.,0.784796515809518,
1.),(1.,0.77498973461648,1.),(1.,0.768230990620621,1.),(1.,0.754249477539376,
1.),(1.,0.7470267311596,1.),(1.,0.732090338555257,1.),(1.,0.724376719977163,
1.),(1.,0.708426290764442,1.),(1.,0.700189512530531,1.),(1.,0.683154153538125,
1.),(1.,0.674355607127678,1.),(1.,0.664115385685685,1.),(1.,0.66297302996927,
1.),(1.,0.660682162177284,1.),(1.,0.659533241882799,1.),(1.,0.65607598168352,
1.),(1.,0.653757142047767,1.),(1.,0.646758317475323,1.),(1.,0.642036016956393,
1.),(1.,0.627697700195677,1.),(1.,0.61790996153014,1.),(1.,0.597870566155991,
1.),(1.,0.58761854570598,1.),(1.,0.566657940545553,1.),(1.,0.555948596069607,
1.),(1.,0.542299741359184,1.),(1.,0.539556972501121,1.),(1.,0.53404656747395,
1.),(1.,0.531276245933983,1.),(1.,0.522962675372791,1.),(1.,0.517409973114278,
1.),(1.,0.506307878837006,1.),(1.,0.500758405674242,1.),(1.,0.489694670444622,
1.),(1.,0.484180295137749,1.),(1.,0.473229585826254,1.),(1.,0.467793092024575,
1.),(1.,0.459740217505025,1.),(1.,0.457073035061414,1.),(1.,0.453104759629238,
1.),(1.,0.451787428134069,1.),(1.,0.449164897866363,1.),(1.,0.447859036145478,
1.),(1.,0.441385443166445,1.),(1.,0.436368154024372,1.),(1.,0.426750681610345,
1.),(1.,0.422150388759125,1.),(1.,0.413481583263519,1.),(1.,0.409412966405537,
1.),(1.,0.403813005360145,1.),(1.,0.402030377100019,1.),(1.,0.399497383040528,
1.),(1.,0.398676556272897,1.),(1.,0.397084562446663,1.),(1.,0.396315545546773,
1.),(1.,0.392617462025358,1.),(1.,0.390121311666049,1.),(1.,0.386146893571918,
1.),(1.,0.384668848565874,1.),(1.,0.382812549250897,1.),(1.,0.382434470212711,
1.),(1.,0.38268919558194,1.),(1.,0.382776371338327,1.),(1.,0.383022089646797,
1.),(1.,0.383180660969252,1.),(1.,0.383762017423613,1.),(1.,0.384290482158863,
1.),(1.,0.386285206501931,1.),(1.,0.388161225874796,1.),(1.,0.391136736543832,
1.),(1.,0.391763914323658,1.),(1.,0.393077192923473,1.),(1.,0.393761818570545,
1.),(1.,0.395895524715283,1.),(1.,0.397424386821021,1.),(1.,0.402298884562898,
1.),(1.,0.405931683845182,1.),(1.,0.413815239487506,1.),(1.,0.418066059410145,
1.),(1.,0.42706069079461,1.),(1.,0.431804585246568,1.),(1.,0.441681473676376,
1.),(1.,0.446814558722576,1.),(1.,0.453420699181124,1.),(1.,0.454748719848507,
1.),(1.,0.457413317151073,1.),(1.,0.458750495400507,1.),(1.,0.462774945482169,
1.),(1.,0.465475093536882,1.),(1.,0.473614842385458,1.),(1.,0.479093267976819,
1.),(1.,0.490102288950609,1.),(1.,0.495633034030675,1.),(1.,0.506709011958283,
1.),(1.,0.512254349645873,1.),(1.,0.528870329213323,1.),(1.,0.539918495566728,
1.),(1.,0.553602176080216,1.),(1.,0.556334955909364,1.),(1.,0.561765821980307,
1.),(1.,0.564466028627623,1.),(1.,0.572520418051971,1.),(1.,0.577828317778608,
1.),(1.,0.593564847150334,1.),(1.,0.603805896926842,1.),(1.,0.623792543125198,
1.),(1.,0.633538444526384,1.),(1.,0.652550041804049,1.),(1.,0.661815883466955,
1.),(1.,0.679885915223711,1.),(1.,0.6886901762844,1.),(1.,0.699418770951675,
1.),(1.,0.701551513084995,1.),(1.,0.705785767125964,1.),(1.,0.707884945612412,
1.),(1.,0.714129661070711,1.),(1.,0.718222393457039,1.),(1.,0.730296979845767,
1.),(1.,0.738075438054285,1.),(1.,0.753124875298064,1.),(1.,0.760395819580576,
1.),(1.,0.774458730322372,1.),(1.,0.781250671280861,1.),(1.,0.794378512232147,
1.),(1.,0.800714394746321,1.),(1.,0.809889696081597,1.),(1.,0.81289333920085,
1.),(1.,0.817317988310256,1.),(1.,0.81877983910783,1.),(1.,0.821667696260936,
1.),(1.,0.823094832962587,1.),(1.,0.830147792104091,1.),(1.,0.835525690411864,
1.),(1.,0.845780003457637,1.),(1.,0.85065638391852,1.),(1.,0.859929290650844,
1.),(1.,0.864325793621342,1.),(1.,0.870573221979968,1.),(1.,0.872597774409058,
1.),(1.,0.875548982801159,1.),(1.,0.876518446809548,1.),(1.,0.877951374397237,
1.),(1.,0.878425435719338,1.),(1.,0.879364277600825,1.),(1.,0.87982934145049,
1.),(1.,0.883976089465827,1.),(1.,0.887386226523438,1.),(1.,0.893695391832222,
1.),(1.,0.896594377182112,1.),(1.,0.901916757914401,1.),(1.,0.904340130964184,
1.),(1.,0.906816643976781,1.),(1.,0.907088077234898,1.),(1.,0.907622483818774,
1.),(1.,0.907885627787149,1.),(1.,0.908663109051759,1.),(1.,0.909165497176662,
1.),(1.,0.910626625009093,1.),(1.,0.911539350769517,1.),(1.,0.91410668701056,
1.),(1.,0.915590785243887,1.),(1.,0.917522428376818,1.),(1.,0.918117142015421,
1.),(1.,0.918940550747601,1.),(1.,0.919203618073144,1.),(1.,0.919707451070459,
1.),(1.,0.919946845560599,1.),(1.,0.921084971631206,1.),(1.,0.921808216030194,
1.),(1.,0.922671204445732,1.),(1.,0.922921678056867,1.),(1.,0.923355716047376,
1.),(1.,0.923539280063381,1.),(1.,0.923768924823362,1.),(1.,0.923837844568734,
1.),(1.,0.923930235120147,1.),(1.,0.923959199701402,1.),(1.,0.924013530789645,
1.),(1.,0.924038911854136,1.),(1.,0.924156810216913,1.),(1.,0.924221785724258,
1.),(1.,0.924299796558392,1.),(1.,0.924312823752853,1.),(1.,0.924291460660933,
1.),(1.,0.924257066663858,1.),(1.,0.924143360666746,1.),(1.,0.924064049018983,
1.),(1.,0.923911786837651,1.),(1.,0.923855468182103,1.),(1.,0.923762549501941,
1.),(1.,0.923730168815134,1.),(1.,0.923679465051457,1.),(1.,0.923662208277328,
1.),(1.,0.923626979380171,1.),(1.,0.923609029138641,1.),(1.,0.923590675042016,
1.)))
REPRESENTATION_ITEM('')
SURFACE()
);
#170=(
BOUNDED_SURFACE()
B_SPLINE_SURFACE(3,2,((#55159,#55160,#55161),(#55162,#55163,#55164),(#55165,
#55166,#55167),(#55168,#55169,#55170),(#55171,#55172,#55173),(#55174,#55175,
#55176),(#55177,#55178,#55179),(#55180,#55181,#55182),(#55183,#55184,#55185),
(#55186,#55187,#55188),(#55189,#55190,#55191),(#55192,#55193,#55194),(#55195,
#55196,#55197),(#55198,#55199,#55200),(#55201,#55202,#55203),(#55204,#55205,
#55206),(#55207,#55208,#55209),(#55210,#55211,#55212),(#55213,#55214,#55215),
(#55216,#55217,#55218),(#55219,#55220,#55221),(#55222,#55223,#55224),(#55225,
#55226,#55227),(#55228,#55229,#55230),(#55231,#55232,#55233),(#55234,#55235,
#55236),(#55237,#55238,#55239),(#55240,#55241,#55242)),.UNSPECIFIED.,.F.,
 .F.,.F.)
B_SPLINE_SURFACE_WITH_KNOTS((4,2,2,2,2,2,2,2,2,2,2,2,2,4),(3,3),(0.00343304549842295,
0.00356923072896442,0.00370541595950589,0.00373946226714126,0.00377350857477663,
0.00384160119004736,0.00397778642058883,0.00404587903585957,0.00407992534349494,
0.00411397165113031,0.00425015688167178,0.00438634211221325,0.00445443472748398,
0.00452252734275472),(0.,1.),.UNSPECIFIED.)
GEOMETRIC_REPRESENTATION_ITEM()
RATIONAL_B_SPLINE_SURFACE(((1.,0.625459232033944,1.),(1.,0.624403554488493,
1.),(1.,0.624295083285682,1.),(1.,0.625831833978692,1.),(1.,0.627477973201858,
1.),(1.,0.630511098040852,1.),(1.,0.631166352850721,1.),(1.,0.632570492553873,
1.),(1.,0.633320984647136,1.),(1.,0.635690804695334,1.),(1.,0.637429575912633,
1.),(1.,0.643040864092948,1.),(1.,0.647308049492937,1.),(1.,0.654182879861181,
1.),(1.,0.656553630245541,1.),(1.,0.660189296321541,1.),(1.,0.661414443264157,
1.),(1.,0.663884637649682,1.),(1.,0.665127312746621,1.),(1.,0.671327551077645,
1.),(1.,0.676275464921448,1.),(1.,0.68573549857353,1.),(1.,0.69024936841657,
1.),(1.,0.696399354422299,1.),(1.,0.698350363530641,1.),(1.,0.70194011110859,
1.),(1.,0.703586217954793,1.),(1.,0.705067492006796,1.)))
REPRESENTATION_ITEM('')
SURFACE()
);
#171=(
BOUNDED_SURFACE()
B_SPLINE_SURFACE(3,2,((#55329,#55330,#55331),(#55332,#55333,#55334),(#55335,
#55336,#55337),(#55338,#55339,#55340)),.UNSPECIFIED.,.F.,.F.,.F.)
B_SPLINE_SURFACE_WITH_KNOTS((4,4),(3,3),(0.0261617207655415,0.0383020860576645),
(-4.27038486529046E-6,1.),.UNSPECIFIED.)
GEOMETRIC_REPRESENTATION_ITEM()
RATIONAL_B_SPLINE_SURFACE(((1.00000160860429,0.811655818092484,1.),(1.0000016253793,
0.809691707667514,1.),(1.00000164120802,0.80783839465713,1.),(1.00000165623531,
0.806078918112741,1.)))
REPRESENTATION_ITEM('')
SURFACE()
);
#172=(
BOUNDED_SURFACE()
B_SPLINE_SURFACE(3,2,((#55354,#55355,#55356),(#55357,#55358,#55359),(#55360,
#55361,#55362),(#55363,#55364,#55365),(#55366,#55367,#55368),(#55369,#55370,
#55371),(#55372,#55373,#55374),(#55375,#55376,#55377),(#55378,#55379,#55380),
(#55381,#55382,#55383),(#55384,#55385,#55386),(#55387,#55388,#55389),(#55390,
#55391,#55392),(#55393,#55394,#55395),(#55396,#55397,#55398),(#55399,#55400,
#55401),(#55402,#55403,#55404),(#55405,#55406,#55407),(#55408,#55409,#55410),
(#55411,#55412,#55413),(#55414,#55415,#55416),(#55417,#55418,#55419),(#55420,
#55421,#55422),(#55423,#55424,#55425),(#55426,#55427,#55428),(#55429,#55430,
#55431),(#55432,#55433,#55434),(#55435,#55436,#55437),(#55438,#55439,#55440),
(#55441,#55442,#55443),(#55444,#55445,#55446),(#55447,#55448,#55449),(#55450,
#55451,#55452),(#55453,#55454,#55455),(#55456,#55457,#55458),(#55459,#55460,
#55461),(#55462,#55463,#55464),(#55465,#55466,#55467),(#55468,#55469,#55470),
(#55471,#55472,#55473),(#55474,#55475,#55476),(#55477,#55478,#55479),(#55480,
#55481,#55482),(#55483,#55484,#55485),(#55486,#55487,#55488),(#55489,#55490,
#55491),(#55492,#55493,#55494),(#55495,#55496,#55497),(#55498,#55499,#55500),
(#55501,#55502,#55503),(#55504,#55505,#55506),(#55507,#55508,#55509),(#55510,
#55511,#55512),(#55513,#55514,#55515),(#55516,#55517,#55518),(#55519,#55520,
#55521),(#55522,#55523,#55524),(#55525,#55526,#55527),(#55528,#55529,#55530),
(#55531,#55532,#55533),(#55534,#55535,#55536),(#55537,#55538,#55539),(#55540,
#55541,#55542),(#55543,#55544,#55545),(#55546,#55547,#55548),(#55549,#55550,
#55551),(#55552,#55553,#55554),(#55555,#55556,#55557),(#55558,#55559,#55560),
(#55561,#55562,#55563),(#55564,#55565,#55566),(#55567,#55568,#55569),(#55570,
#55571,#55572),(#55573,#55574,#55575),(#55576,#55577,#55578),(#55579,#55580,
#55581),(#55582,#55583,#55584),(#55585,#55586,#55587),(#55588,#55589,#55590),
(#55591,#55592,#55593),(#55594,#55595,#55596),(#55597,#55598,#55599),(#55600,
#55601,#55602),(#55603,#55604,#55605),(#55606,#55607,#55608),(#55609,#55610,
#55611),(#55612,#55613,#55614),(#55615,#55616,#55617)),.UNSPECIFIED.,.F.,
 .F.,.F.)
B_SPLINE_SURFACE_WITH_KNOTS((4,2,2,2,2,2,2,2,2,2,2,2,2,2,2,2,2,2,2,2,2,
2,2,2,2,2,2,2,2,2,2,2,2,2,2,2,2,2,2,2,2,2,2,4),(3,3),(0.00330261648339416,
0.00340081661298013,0.0034990167425661,0.00359721687215207,0.00364631693694505,
0.00369541700173804,0.003793617131324,0.00389181726090997,0.00394091732570296,
0.00396546735809945,0.00399001739049594,0.00408821752008191,0.00418641764966788,
0.00428461777925385,0.00438281790883982,0.00448101803842579,0.00457921816801176,
0.00462831823280474,0.00467741829759773,0.0047756184271837,0.00487381855676967,
0.00492291862156265,0.00494746865395914,0.00497201868635564,0.00507021881594161,
0.00516841894552758,0.00526661907511355,0.00531571913990653,0.00536481920469952,
0.00546301933428548,0.00556121946387145,0.00561031952866444,0.00565941959345742,
0.00575761972304339,0.00585581985262936,0.00590491991742235,0.00595401998221533,
0.0060522201118013,0.00615042024138727,0.00624862037097324,0.00627317040336973,
0.00629772043576622,0.00634682050055921,0.00644502063014518),(0.,1.),
 .UNSPECIFIED.)
GEOMETRIC_REPRESENTATION_ITEM()
RATIONAL_B_SPLINE_SURFACE(((1.,0.811656622391199,1.),(1.,0.811832571892841,
1.),(1.,0.811683313300623,1.),(1.,0.810765075561372,1.),(1.,0.809996124532223,
1.),(1.,0.807864448627461,1.),(1.,0.806501656926263,1.),(1.,0.804028901809539,
1.),(1.,0.803130322510617,1.),(1.,0.801211698750432,1.),(1.,0.800191446782092,
1.),(1.,0.796961352096929,1.),(1.,0.794582241729763,1.),(1.,0.789440647694272,
1.),(1.,0.786677989170548,1.),(1.,0.782296748929349,1.),(1.,0.780796800906642,
1.),(1.,0.77849415738182,1.),(1.,0.777717216045269,1.),(1.,0.776155137355144,
1.),(1.,0.77536909367214,1.),(1.,0.771417467466651,1.),(1.,0.768187639991458,
1.),(1.,0.761682357768366,1.),(1.,0.758406710407249,1.),(1.,0.751903933721366,
1.),(1.,0.748676603631679,1.),(1.,0.742373233767419,1.),(1.,0.739347411643543,
1.),(1.,0.733646267736223,1.),(1.,0.730969295702006,1.),(1.,0.726052823770446,
1.),(1.,0.723813234691965,1.),(1.,0.720852062565936,1.),(1.,0.719931403475167,
1.),(1.,0.718235111366214,1.),(1.,0.717466660341387,1.),(1.,0.715409033219939,
1.),(1.,0.714366635072083,1.),(1.,0.712967965168178,1.),(1.,0.712611690057782,
1.),(1.,0.712607635738503,1.),(1.,0.712694626675192,1.),(1.,0.71295915503469,
1.),(1.,0.713069668154168,1.),(1.,0.713335587614801,1.),(1.,0.713491283850726,
1.),(1.,0.714377922232085,1.),(1.,0.715432840757552,1.),(1.,0.718169210541053,
1.),(1.,0.719850696145383,1.),(1.,0.723773857278612,1.),(1.,0.726015568252412,
1.),(1.,0.72974661827765,1.),(1.,0.731052887236837,1.),(1.,0.733748031839737,
1.),(1.,0.735140203148474,1.),(1.,0.739430403187765,1.),(1.,0.742441933617721,
1.),(1.,0.748666868677604,1.),(1.,0.751880423473639,1.),(1.,0.756780279406297,
1.),(1.,0.758426889889258,1.),(1.,0.761734578028716,1.),(1.,0.763382933672718,
1.),(1.,0.768291653115061,1.),(1.,0.7715165857284,1.),(1.,0.777785013497246,
1.),(1.,0.780828707268701,1.),(1.,0.785196484807998,1.),(1.,0.786619464822865,
1.),(1.,0.78938908710468,1.),(1.,0.790737454081499,1.),(1.,0.794640861183113,
1.),(1.,0.797024425496887,1.),(1.,0.801307056342078,1.),(1.,0.803206253057746,
1.),(1.,0.806472900192383,1.),(1.,0.807840481551189,1.),(1.,0.809185497223154,
1.),(1.,0.809436262730181,1.),(1.,0.809900438192552,1.),(1.,0.810114130417425,
1.),(1.,0.810695487125602,1.),(1.,0.811003336720787,1.),(1.,0.811689316099667,
1.),(1.,0.811829944488298,1.),(1.,0.811656622391197,1.)))
REPRESENTATION_ITEM('')
SURFACE()
);
#173=(
BOUNDED_SURFACE()
B_SPLINE_SURFACE(3,2,((#55619,#55620,#55621),(#55622,#55623,#55624),(#55625,
#55626,#55627),(#55628,#55629,#55630)),.UNSPECIFIED.,.F.,.F.,.F.)
B_SPLINE_SURFACE_WITH_KNOTS((4,4),(3,3),(-7.97972798949331E-17,0.0113332794371223),
(0.,1.),.UNSPECIFIED.)
GEOMETRIC_REPRESENTATION_ITEM()
RATIONAL_B_SPLINE_SURFACE(((1.,0.806431892643699,1.),(1.,0.808086137640199,
1.),(1.,0.809823081379547,1.),(1.,0.811656622391199,1.)))
REPRESENTATION_ITEM('')
SURFACE()
);
#174=(
BOUNDED_SURFACE()
B_SPLINE_SURFACE(3,2,((#55637,#55638,#55639),(#55640,#55641,#55642),(#55643,
#55644,#55645),(#55646,#55647,#55648),(#55649,#55650,#55651),(#55652,#55653,
#55654),(#55655,#55656,#55657),(#55658,#55659,#55660),(#55661,#55662,#55663),
(#55664,#55665,#55666),(#55667,#55668,#55669),(#55670,#55671,#55672),(#55673,
#55674,#55675),(#55676,#55677,#55678),(#55679,#55680,#55681),(#55682,#55683,
#55684),(#55685,#55686,#55687),(#55688,#55689,#55690),(#55691,#55692,#55693),
(#55694,#55695,#55696),(#55697,#55698,#55699),(#55700,#55701,#55702),(#55703,
#55704,#55705),(#55706,#55707,#55708),(#55709,#55710,#55711),(#55712,#55713,
#55714),(#55715,#55716,#55717),(#55718,#55719,#55720),(#55721,#55722,#55723),
(#55724,#55725,#55726),(#55727,#55728,#55729),(#55730,#55731,#55732),(#55733,
#55734,#55735),(#55736,#55737,#55738),(#55739,#55740,#55741),(#55742,#55743,
#55744),(#55745,#55746,#55747),(#55748,#55749,#55750),(#55751,#55752,#55753),
(#55754,#55755,#55756),(#55757,#55758,#55759),(#55760,#55761,#55762),(#55763,
#55764,#55765),(#55766,#55767,#55768),(#55769,#55770,#55771),(#55772,#55773,
#55774)),.UNSPECIFIED.,.F.,.F.,.F.)
B_SPLINE_SURFACE_WITH_KNOTS((4,2,2,2,2,2,2,2,2,2,2,2,2,2,2,2,2,2,2,2,2,
2,4),(3,3),(-4.82469966756049E-18,5.50518151362045E-5,0.000110103630272414,
0.000165155445408623,0.000192681352976728,0.000220207260544833,0.000275259075681042,
0.000330310890817251,0.000357836798385356,0.000371599752169408,0.000385362705953461,
0.00044041452108967,0.000495466336225879,0.000522992243793984,0.000550518151362089,
0.000605569966498298,0.000660621781634507,0.000688147689202612,0.000701910642986664,
0.000715673596770717,0.000770725411906926,0.000825777227043135,0.000880829042179345),
(0.,1.),.UNSPECIFIED.)
GEOMETRIC_REPRESENTATION_ITEM()
RATIONAL_B_SPLINE_SURFACE(((1.,0.707106781185485,1.),(1.,0.710477894989039,
1.),(1.,0.713841886492236,1.),(1.,0.720556846901308,1.),(1.,0.723907847252579,
1.),(1.,0.730596240721846,1.),(1.,0.733933644391114,1.),(1.,0.738927431407798,
1.),(1.,0.740594246210395,1.),(1.,0.743888192923081,1.),(1.,0.745518215666872,
1.),(1.,0.750357382687748,1.),(1.,0.753515818763767,1.),(1.,0.75969242534585,
1.),(1.,0.76271062408444,1.),(1.,0.76712420463012,1.),(1.,0.76857639446933,
1.),(1.,0.770724569363179,1.),(1.,0.771434643119713,1.),(1.,0.772836027726094,
1.),(1.,0.773528322117743,1.),(1.,0.776947799211149,1.),(1.,0.779549385320001,
1.),(1.,0.784478174057131,1.),(1.,0.78680540757744,1.),(1.,0.790078083140807,
1.),(1.,0.791132534016176,1.),(1.,0.793165396446497,1.),(1.,0.794146568495307,
1.),(1.,0.796938387532037,1.),(1.,0.79860524372839,1.),(1.,0.801549647651601,
1.),(1.,0.802827202148284,1.),(1.,0.804441694539674,1.),(1.,0.80492945694585,
1.),(1.,0.805583313651139,1.),(1.,0.805788296097707,1.),(1.,0.806171865231364,
1.),(1.,0.806350694157879,1.),(1.,0.807172777122824,1.),(1.,0.807603802187835,
1.),(1.,0.808025829002193,1.),(1.,0.808016790860372,1.),(1.,0.807558204302794,
1.),(1.,0.807108474283634,1.),(1.,0.806431892643561,1.)))
REPRESENTATION_ITEM('')
SURFACE()
);
#175=(
BOUNDED_SURFACE()
B_SPLINE_SURFACE(3,2,((#55886,#55887,#55888),(#55889,#55890,#55891),(#55892,
#55893,#55894),(#55895,#55896,#55897),(#55898,#55899,#55900),(#55901,#55902,
#55903),(#55904,#55905,#55906),(#55907,#55908,#55909),(#55910,#55911,#55912),
(#55913,#55914,#55915),(#55916,#55917,#55918),(#55919,#55920,#55921),(#55922,
#55923,#55924),(#55925,#55926,#55927),(#55928,#55929,#55930),(#55931,#55932,
#55933),(#55934,#55935,#55936),(#55937,#55938,#55939),(#55940,#55941,#55942),
(#55943,#55944,#55945),(#55946,#55947,#55948),(#55949,#55950,#55951),(#55952,
#55953,#55954),(#55955,#55956,#55957),(#55958,#55959,#55960),(#55961,#55962,
#55963),(#55964,#55965,#55966),(#55967,#55968,#55969),(#55970,#55971,#55972),
(#55973,#55974,#55975),(#55976,#55977,#55978),(#55979,#55980,#55981),(#55982,
#55983,#55984),(#55985,#55986,#55987),(#55988,#55989,#55990),(#55991,#55992,
#55993),(#55994,#55995,#55996),(#55997,#55998,#55999),(#56000,#56001,#56002),
(#56003,#56004,#56005),(#56006,#56007,#56008),(#56009,#56010,#56011),(#56012,
#56013,#56014),(#56015,#56016,#56017),(#56018,#56019,#56020),(#56021,#56022,
#56023),(#56024,#56025,#56026),(#56027,#56028,#56029),(#56030,#56031,#56032),
(#56033,#56034,#56035),(#56036,#56037,#56038),(#56039,#56040,#56041),(#56042,
#56043,#56044),(#56045,#56046,#56047),(#56048,#56049,#56050),(#56051,#56052,
#56053)),.UNSPECIFIED.,.F.,.F.,.F.)
B_SPLINE_SURFACE_WITH_KNOTS((4,2,2,2,2,2,2,2,2,2,2,2,2,2,2,2,2,2,2,2,2,
2,2,2,2,2,2,4),(3,3),(0.0032383527045278,0.00336554775906757,0.00349274281360733,
0.00355634034087722,0.00358813910451216,0.0036199378681471,0.00374713292268687,
0.00387432797722664,0.00390612674086158,0.00393792550449652,0.0040015230317664,
0.00412871808630617,0.00419231561357605,0.00422411437721099,0.00425591314084594,
0.0043831081953857,0.00451030324992547,0.00457390077719535,0.0046056995408303,
0.00463749830446524,0.004764693359005,0.00489188841354477,0.00492368717717971,
0.00495548594081465,0.00501908346808454,0.0051462785226243,0.00520987604989419,
0.00527347357716407),(0.,1.),.UNSPECIFIED.)
GEOMETRIC_REPRESENTATION_ITEM()
RATIONAL_B_SPLINE_SURFACE(((1.,0.70710678118655,1.),(1.,0.706213957993281,
1.),(1.,0.705443938786405,1.),(1.,0.704136988709561,1.),(1.,0.703600079667857,
1.),(1.,0.702960418588502,1.),(1.,0.70277481545753,1.),(1.,0.702536660935443,
1.),(1.,0.702463890650407,1.),(1.,0.702332362486225,1.),(1.,0.702273501931224,
1.),(1.,0.70201213439835,1.),(1.,0.701908295200086,1.),(1.,0.701873429093663,
1.),(1.,0.701942493739908,1.),(1.,0.702114701888608,1.),(1.,0.70215343927011,
1.),(1.,0.702238949474263,1.),(1.,0.702285595803191,1.),(1.,0.702435575186992,
1.),(1.,0.702549116540971,1.),(1.,0.702921418342714,1.),(1.,0.703211731033178,
1.),(1.,0.703677757909964,1.),(1.,0.703838232332125,1.),(1.,0.704082806712229,
1.),(1.,0.704164976900933,1.),(1.,0.704329977699004,1.),(1.,0.704412960144125,
1.),(1.,0.704825691362464,1.),(1.,0.705148590086159,1.),(1.,0.705745128898862,
1.),(1.,0.706018867880871,1.),(1.,0.706371078301196,1.),(1.,0.706478786100633,
1.),(1.,0.706623371663295,1.),(1.,0.706668657551497,1.),(1.,0.706752667613401,
1.),(1.,0.706791471875649,1.),(1.,0.706969088136416,1.),(1.,0.7070584672857,
1.),(1.,0.707125223844347,1.),(1.,0.707102609206611,1.),(1.,0.70700357459,
1.),(1.,0.706980197085667,1.),(1.,0.706926650254296,1.),(1.,0.706896532893769,
1.),(1.,0.706796567062846,1.),(1.,0.70671709597817,1.),(1.,0.706443815084179,
1.),(1.,0.706214968750598,1.),(1.,0.705818771778775,1.),(1.,0.705677922813091,
1.),(1.,0.70538206823473,1.),(1.,0.705226726837797,1.),(1.,0.705067492006796,
1.)))
REPRESENTATION_ITEM('')
SURFACE()
);
#176=(
BOUNDED_SURFACE()
B_SPLINE_SURFACE(3,2,((#56268,#56269,#56270),(#56271,#56272,#56273),(#56274,
#56275,#56276),(#56277,#56278,#56279),(#56280,#56281,#56282),(#56283,#56284,
#56285),(#56286,#56287,#56288),(#56289,#56290,#56291),(#56292,#56293,#56294),
(#56295,#56296,#56297),(#56298,#56299,#56300),(#56301,#56302,#56303),(#56304,
#56305,#56306),(#56307,#56308,#56309),(#56310,#56311,#56312),(#56313,#56314,
#56315),(#56316,#56317,#56318),(#56319,#56320,#56321),(#56322,#56323,#56324),
(#56325,#56326,#56327),(#56328,#56329,#56330),(#56331,#56332,#56333),(#56334,
#56335,#56336),(#56337,#56338,#56339),(#56340,#56341,#56342),(#56343,#56344,
#56345),(#56346,#56347,#56348),(#56349,#56350,#56351)),.UNSPECIFIED.,.F.,
 .F.,.F.)
B_SPLINE_SURFACE_WITH_KNOTS((4,2,2,2,2,2,2,2,2,2,2,2,2,4),(3,3),(0.0012120764411892,
0.0013497499377862,0.00148742343438319,0.00162509693098018,0.00176277042757717,
0.00203811742077116,0.00231346441396515,0.00258881140715913,0.00286415840035312,
0.0031395053935471,0.0032771788901441,0.00334601563844259,0.00338043401259184,
0.00341485238674109),(0.,1.),.UNSPECIFIED.)
GEOMETRIC_REPRESENTATION_ITEM()
RATIONAL_B_SPLINE_SURFACE(((1.,0.707106781186468,1.),(1.,0.72002470605839,
1.),(1.,0.732433086825891,1.),(1.,0.756294061054311,1.),(1.,0.767746781874307,
1.),(1.,0.789743409782971,1.),(1.,0.800289212024087,1.),(1.,0.820486268600631,
1.),(1.,0.830140018061829,1.),(1.,0.857814961348585,1.),(1.,0.874552353369404,
1.),(1.,0.904768093055729,1.),(1.,0.918244574153276,1.),(1.,0.942040431761282,
1.),(1.,0.952358767872154,1.),(1.,0.969924448818458,1.),(1.,0.977171377622921,
1.),(1.,0.988685707102147,1.),(1.,0.992953212410708,1.),(1.,0.997195607349612,
1.),(1.,0.998249987789548,1.),(1.,0.999301490798357,1.),(1.,0.999563645238205,
1.),(1.,0.999825517691477,1.),(1.,0.999890914840196,1.),(1.,0.999978110425983,
1.),(1.,0.999999927945283,1.),(1.,1.,1.)))
REPRESENTATION_ITEM('')
SURFACE()
);
#177=(
BOUNDED_SURFACE()
B_SPLINE_SURFACE(3,2,((#56602,#56603,#56604),(#56605,#56606,#56607),(#56608,
#56609,#56610),(#56611,#56612,#56613),(#56614,#56615,#56616),(#56617,#56618,
#56619),(#56620,#56621,#56622),(#56623,#56624,#56625),(#56626,#56627,#56628),
(#56629,#56630,#56631),(#56632,#56633,#56634),(#56635,#56636,#56637),(#56638,
#56639,#56640),(#56641,#56642,#56643),(#56644,#56645,#56646),(#56647,#56648,
#56649),(#56650,#56651,#56652),(#56653,#56654,#56655),(#56656,#56657,#56658),
(#56659,#56660,#56661),(#56662,#56663,#56664),(#56665,#56666,#56667),(#56668,
#56669,#56670),(#56671,#56672,#56673),(#56674,#56675,#56676),(#56677,#56678,
#56679),(#56680,#56681,#56682),(#56683,#56684,#56685)),.UNSPECIFIED.,.F.,
 .F.,.F.)
B_SPLINE_SURFACE_WITH_KNOTS((4,2,2,2,2,2,2,2,2,2,2,2,2,4),(3,3),(0.00121207644118946,
0.00134974993778644,0.00148742343438341,0.00162509693098039,0.00176277042757736,
0.00203811742077132,0.00231346441396527,0.00258881140715922,0.00286415840035317,
0.00313950539354712,0.0032771788901441,0.00334601563844259,0.00338043401259183,
0.00341485238674108),(0.,1.),.UNSPECIFIED.)
GEOMETRIC_REPRESENTATION_ITEM()
RATIONAL_B_SPLINE_SURFACE(((1.,0.707106781186544,1.),(1.,0.720024706058528,
1.),(1.,0.732433086825873,1.),(1.,0.756294061054466,1.),(1.,0.767746781874374,
1.),(1.,0.78974340978302,1.),(1.,0.800289212024211,1.),(1.,0.820486268600606,
1.),(1.,0.830140018061826,1.),(1.,0.857814961348716,1.),(1.,0.87455235336949,
1.),(1.,0.90476809305572,1.),(1.,0.918244574153158,1.),(1.,0.942040431761433,
1.),(1.,0.952358767872266,1.),(1.,0.969924448818365,1.),(1.,0.977171377622992,
1.),(1.,0.988685707102086,1.),(1.,0.99295321241071,1.),(1.,0.997195607349613,
1.),(1.,0.998249987789543,1.),(1.,0.99930149079836,1.),(1.,0.999563645238205,
1.),(1.,0.999825517691477,1.),(1.,0.999890914840191,1.),(1.,0.999978110425987,
1.),(1.,0.999999927945279,1.),(1.,1.,1.)))
REPRESENTATION_ITEM('')
SURFACE()
);
#178=(
BOUNDED_SURFACE()
B_SPLINE_SURFACE(3,2,((#56792,#56793,#56794),(#56795,#56796,#56797),(#56798,
#56799,#56800),(#56801,#56802,#56803),(#56804,#56805,#56806),(#56807,#56808,
#56809),(#56810,#56811,#56812),(#56813,#56814,#56815),(#56816,#56817,#56818),
(#56819,#56820,#56821),(#56822,#56823,#56824),(#56825,#56826,#56827),(#56828,
#56829,#56830),(#56831,#56832,#56833),(#56834,#56835,#56836),(#56837,#56838,
#56839),(#56840,#56841,#56842),(#56843,#56844,#56845),(#56846,#56847,#56848),
(#56849,#56850,#56851),(#56852,#56853,#56854),(#56855,#56856,#56857),(#56858,
#56859,#56860),(#56861,#56862,#56863),(#56864,#56865,#56866),(#56867,#56868,
#56869),(#56870,#56871,#56872),(#56873,#56874,#56875)),.UNSPECIFIED.,.F.,
 .F.,.F.)
B_SPLINE_SURFACE_WITH_KNOTS((4,2,2,2,2,2,2,2,2,2,2,2,2,4),(3,3),(-1.34164157599756E-5,
2.06868368462185E-5,5.47900894524126E-5,0.000122996594664801,0.000259409605089577,
0.00053223562593913,0.000805061646788683,0.00107788766763824,0.00135071368848779,
0.00162353970933734,0.00175995271976212,0.0018963657301869,0.00203277874061167,
0.00216919175103645),(0.,1.),.UNSPECIFIED.)
GEOMETRIC_REPRESENTATION_ITEM()
RATIONAL_B_SPLINE_SURFACE(((1.,1.,1.),(1.,1.00000001507238,1.),(1.,0.999978441292673,
1.),(1.,0.999891806781135,1.),(1.,0.9998267650581,1.),(1.,0.999566166629267,
1.),(1.,0.999305138400123,1.),(1.,0.99825771444247,1.),(1.,0.997206984918604,
1.),(1.,0.992977382403944,1.),(1.,0.988720812320532,1.),(1.,0.977229079290884,
1.),(1.,0.969993795445904,1.),(1.,0.952449695699923,1.),(1.,0.942140526220492,
1.),(1.,0.918365194495103,1.),(1.,0.90490049697849,1.),(1.,0.874707837529653,
1.),(1.,0.85798179866746,1.),(1.,0.830317205299946,1.),(1.,0.820664626400707,
1.),(1.,0.80047208844851,1.),(1.,0.789932732031198,1.),(1.,0.767926390428376,
1.),(1.,0.756459594779169,1.),(1.,0.732541332877355,1.),(1.,0.720089718170756,
1.),(1.,0.707106781186543,1.)))
REPRESENTATION_ITEM('')
SURFACE()
);
#179=(
BOUNDED_SURFACE()
B_SPLINE_SURFACE(3,2,((#56962,#56963,#56964),(#56965,#56966,#56967),(#56968,
#56969,#56970),(#56971,#56972,#56973),(#56974,#56975,#56976),(#56977,#56978,
#56979),(#56980,#56981,#56982),(#56983,#56984,#56985),(#56986,#56987,#56988),
(#56989,#56990,#56991),(#56992,#56993,#56994),(#56995,#56996,#56997),(#56998,
#56999,#57000),(#57001,#57002,#57003),(#57004,#57005,#57006),(#57007,#57008,
#57009),(#57010,#57011,#57012),(#57013,#57014,#57015),(#57016,#57017,#57018),
(#57019,#57020,#57021),(#57022,#57023,#57024),(#57025,#57026,#57027),(#57028,
#57029,#57030),(#57031,#57032,#57033),(#57034,#57035,#57036),(#57037,#57038,
#57039),(#57040,#57041,#57042),(#57043,#57044,#57045)),.UNSPECIFIED.,.F.,
 .F.,.F.)
B_SPLINE_SURFACE_WITH_KNOTS((4,2,2,2,2,2,2,2,2,2,2,2,2,4),(3,3),(-1.34164157599273E-5,
2.06868368462668E-5,5.47900894524609E-5,0.000122996594664849,0.000259409605089626,
0.000532235625939179,0.000805061646788732,0.00107788766763828,0.00135071368848784,
0.00162353970933739,0.00175995271976217,0.00189636573018694,0.00203277874061172,
0.0021691917510365),(0.,1.),.UNSPECIFIED.)
GEOMETRIC_REPRESENTATION_ITEM()
RATIONAL_B_SPLINE_SURFACE(((1.,1.,1.),(1.,1.00000001507238,1.),(1.,0.999978441292673,
1.),(1.,0.999891806781135,1.),(1.,0.9998267650581,1.),(1.,0.999566166629267,
1.),(1.,0.999305138400118,1.),(1.,0.998257714442481,1.),(1.,0.997206984918586,
1.),(1.,0.992977382403979,1.),(1.,0.988720812320531,1.),(1.,0.977229079290883,
1.),(1.,0.969993795445918,1.),(1.,0.952449695699907,1.),(1.,0.942140526220349,
1.),(1.,0.918365194495244,1.),(1.,0.904900496979517,1.),(1.,0.874707837530609,
1.),(1.,0.857981798667344,1.),(1.,0.830317205300004,1.),(1.,0.82066462640065,
1.),(1.,0.800472088448564,1.),(1.,0.789932732031166,1.),(1.,0.767926390428401,
1.),(1.,0.756459594779094,1.),(1.,0.732541332877426,1.),(1.,0.720089718170704,
1.),(1.,0.707106781186544,1.)))
REPRESENTATION_ITEM('')
SURFACE()
);
#180=(
BOUNDED_SURFACE()
B_SPLINE_SURFACE(3,2,((#57341,#57342,#57343),(#57344,#57345,#57346),(#57347,
#57348,#57349),(#57350,#57351,#57352),(#57353,#57354,#57355),(#57356,#57357,
#57358),(#57359,#57360,#57361),(#57362,#57363,#57364),(#57365,#57366,#57367),
(#57368,#57369,#57370),(#57371,#57372,#57373),(#57374,#57375,#57376),(#57377,
#57378,#57379),(#57380,#57381,#57382),(#57383,#57384,#57385),(#57386,#57387,
#57388),(#57389,#57390,#57391),(#57392,#57393,#57394),(#57395,#57396,#57397),
(#57398,#57399,#57400),(#57401,#57402,#57403),(#57404,#57405,#57406),(#57407,
#57408,#57409),(#57410,#57411,#57412),(#57413,#57414,#57415),(#57416,#57417,
#57418),(#57419,#57420,#57421),(#57422,#57423,#57424),(#57425,#57426,#57427),
(#57428,#57429,#57430),(#57431,#57432,#57433),(#57434,#57435,#57436),(#57437,
#57438,#57439),(#57440,#57441,#57442),(#57443,#57444,#57445),(#57446,#57447,
#57448),(#57449,#57450,#57451),(#57452,#57453,#57454),(#57455,#57456,#57457),
(#57458,#57459,#57460),(#57461,#57462,#57463),(#57464,#57465,#57466),(#57467,
#57468,#57469),(#57470,#57471,#57472),(#57473,#57474,#57475),(#57476,#57477,
#57478),(#57479,#57480,#57481),(#57482,#57483,#57484),(#57485,#57486,#57487),
(#57488,#57489,#57490),(#57491,#57492,#57493),(#57494,#57495,#57496),(#57497,
#57498,#57499),(#57500,#57501,#57502),(#57503,#57504,#57505),(#57506,#57507,
#57508),(#57509,#57510,#57511),(#57512,#57513,#57514),(#57515,#57516,#57517),
(#57518,#57519,#57520),(#57521,#57522,#57523),(#57524,#57525,#57526),(#57527,
#57528,#57529),(#57530,#57531,#57532),(#57533,#57534,#57535),(#57536,#57537,
#57538),(#57539,#57540,#57541),(#57542,#57543,#57544),(#57545,#57546,#57547),
(#57548,#57549,#57550),(#57551,#57552,#57553),(#57554,#57555,#57556),(#57557,
#57558,#57559),(#57560,#57561,#57562),(#57563,#57564,#57565),(#57566,#57567,
#57568),(#57569,#57570,#57571),(#57572,#57573,#57574),(#57575,#57576,#57577),
(#57578,#57579,#57580),(#57581,#57582,#57583),(#57584,#57585,#57586),(#57587,
#57588,#57589),(#57590,#57591,#57592),(#57593,#57594,#57595),(#57596,#57597,
#57598),(#57599,#57600,#57601),(#57602,#57603,#57604),(#57605,#57606,#57607),
(#57608,#57609,#57610),(#57611,#57612,#57613),(#57614,#57615,#57616),(#57617,
#57618,#57619),(#57620,#57621,#57622),(#57623,#57624,#57625),(#57626,#57627,
#57628),(#57629,#57630,#57631),(#57632,#57633,#57634),(#57635,#57636,#57637),
(#57638,#57639,#57640),(#57641,#57642,#57643),(#57644,#57645,#57646),(#57647,
#57648,#57649),(#57650,#57651,#57652),(#57653,#57654,#57655),(#57656,#57657,
#57658),(#57659,#57660,#57661),(#57662,#57663,#57664),(#57665,#57666,#57667),
(#57668,#57669,#57670),(#57671,#57672,#57673),(#57674,#57675,#57676),(#57677,
#57678,#57679),(#57680,#57681,#57682),(#57683,#57684,#57685),(#57686,#57687,
#57688),(#57689,#57690,#57691),(#57692,#57693,#57694),(#57695,#57696,#57697),
(#57698,#57699,#57700),(#57701,#57702,#57703),(#57704,#57705,#57706),(#57707,
#57708,#57709),(#57710,#57711,#57712),(#57713,#57714,#57715),(#57716,#57717,
#57718),(#57719,#57720,#57721),(#57722,#57723,#57724),(#57725,#57726,#57727),
(#57728,#57729,#57730),(#57731,#57732,#57733),(#57734,#57735,#57736),(#57737,
#57738,#57739),(#57740,#57741,#57742),(#57743,#57744,#57745),(#57746,#57747,
#57748),(#57749,#57750,#57751),(#57752,#57753,#57754),(#57755,#57756,#57757),
(#57758,#57759,#57760),(#57761,#57762,#57763),(#57764,#57765,#57766),(#57767,
#57768,#57769),(#57770,#57771,#57772),(#57773,#57774,#57775),(#57776,#57777,
#57778),(#57779,#57780,#57781),(#57782,#57783,#57784),(#57785,#57786,#57787),
(#57788,#57789,#57790),(#57791,#57792,#57793),(#57794,#57795,#57796),(#57797,
#57798,#57799),(#57800,#57801,#57802),(#57803,#57804,#57805),(#57806,#57807,
#57808),(#57809,#57810,#57811),(#57812,#57813,#57814),(#57815,#57816,#57817),
(#57818,#57819,#57820),(#57821,#57822,#57823),(#57824,#57825,#57826),(#57827,
#57828,#57829),(#57830,#57831,#57832),(#57833,#57834,#57835),(#57836,#57837,
#57838),(#57839,#57840,#57841),(#57842,#57843,#57844),(#57845,#57846,#57847),
(#57848,#57849,#57850),(#57851,#57852,#57853),(#57854,#57855,#57856),(#57857,
#57858,#57859),(#57860,#57861,#57862),(#57863,#57864,#57865),(#57866,#57867,
#57868),(#57869,#57870,#57871),(#57872,#57873,#57874),(#57875,#57876,#57877),
(#57878,#57879,#57880),(#57881,#57882,#57883),(#57884,#57885,#57886),(#57887,
#57888,#57889),(#57890,#57891,#57892),(#57893,#57894,#57895),(#57896,#57897,
#57898),(#57899,#57900,#57901),(#57902,#57903,#57904),(#57905,#57906,#57907),
(#57908,#57909,#57910),(#57911,#57912,#57913),(#57914,#57915,#57916),(#57917,
#57918,#57919),(#57920,#57921,#57922),(#57923,#57924,#57925),(#57926,#57927,
#57928),(#57929,#57930,#57931),(#57932,#57933,#57934),(#57935,#57936,#57937),
(#57938,#57939,#57940),(#57941,#57942,#57943),(#57944,#57945,#57946),(#57947,
#57948,#57949),(#57950,#57951,#57952),(#57953,#57954,#57955),(#57956,#57957,
#57958),(#57959,#57960,#57961),(#57962,#57963,#57964),(#57965,#57966,#57967),
(#57968,#57969,#57970),(#57971,#57972,#57973),(#57974,#57975,#57976),(#57977,
#57978,#57979),(#57980,#57981,#57982),(#57983,#57984,#57985),(#57986,#57987,
#57988),(#57989,#57990,#57991),(#57992,#57993,#57994),(#57995,#57996,#57997),
(#57998,#57999,#58000),(#58001,#58002,#58003),(#58004,#58005,#58006),(#58007,
#58008,#58009),(#58010,#58011,#58012),(#58013,#58014,#58015),(#58016,#58017,
#58018),(#58019,#58020,#58021),(#58022,#58023,#58024),(#58025,#58026,#58027),
(#58028,#58029,#58030),(#58031,#58032,#58033),(#58034,#58035,#58036),(#58037,
#58038,#58039),(#58040,#58041,#58042),(#58043,#58044,#58045),(#58046,#58047,
#58048),(#58049,#58050,#58051),(#58052,#58053,#58054),(#58055,#58056,#58057),
(#58058,#58059,#58060),(#58061,#58062,#58063),(#58064,#58065,#58066),(#58067,
#58068,#58069),(#58070,#58071,#58072),(#58073,#58074,#58075),(#58076,#58077,
#58078),(#58079,#58080,#58081),(#58082,#58083,#58084),(#58085,#58086,#58087),
(#58088,#58089,#58090),(#58091,#58092,#58093),(#58094,#58095,#58096),(#58097,
#58098,#58099),(#58100,#58101,#58102),(#58103,#58104,#58105),(#58106,#58107,
#58108),(#58109,#58110,#58111),(#58112,#58113,#58114),(#58115,#58116,#58117),
(#58118,#58119,#58120),(#58121,#58122,#58123),(#58124,#58125,#58126),(#58127,
#58128,#58129),(#58130,#58131,#58132),(#58133,#58134,#58135),(#58136,#58137,
#58138)),.UNSPECIFIED.,.T.,.F.,.F.)
B_SPLINE_SURFACE_WITH_KNOTS((4,2,2,2,2,2,2,2,2,2,2,2,2,2,2,2,2,2,2,2,2,
2,2,2,2,2,2,2,2,2,2,2,2,2,2,2,2,2,2,2,2,2,2,2,2,2,2,2,2,2,2,2,2,2,2,2,2,
2,2,2,2,2,2,2,2,2,2,2,2,2,2,2,2,2,2,2,2,2,2,2,2,2,2,2,2,2,2,2,2,2,2,2,2,
2,2,2,2,2,2,2,2,2,2,2,2,2,2,2,2,2,2,2,2,2,2,2,2,2,2,2,2,2,2,2,2,2,2,2,2,
2,2,2,4),(3,3),(0.,4.12881615541384E-5,8.25763231082768E-5,0.000165152646216554,
0.000330305292433107,0.000660610584866214,0.000990915877299321,0.00132122116973243,
0.00148637381594898,0.00156895013905726,0.00165152646216554,0.00198183175459864,
0.00264244233946486,0.00297274763189796,0.00313790027811452,0.00322047660122279,
0.00330305292433107,0.00396366350919728,0.0046242740940635,0.00495457938649661,
0.00503715570960488,0.00511973203271316,0.00528488467892971,0.00594549526379593,
0.00660610584866214,0.00693641114109525,0.00701898746420353,0.0071015637873118,
0.00726671643352836,0.00792732701839457,0.00858793760326078,0.009248548188127,
0.00990915877299321,0.0100743114192098,0.0102394640654263,0.0105697693578594,
0.0112303799427256,0.0118909905275919,0.0125516011124581,0.0132122116973243,
0.0138728222821905,0.0139553986052988,0.0140379749284071,0.0142031275746236,
0.0145334328670567,0.0151940434519229,0.0158546540367891,0.0165152646216554,
0.0166804172678719,0.0168455699140885,0.0171758752065216,0.0175061804989547,
0.0178364857913878,0.0181667910838209,0.0183319437300374,0.0184145200531457,
0.018497096376254,0.0188274016686871,0.0191577069611202,0.0194880122535533,
0.0196531648997699,0.0197357412228781,0.0198183175459864,0.0201486228384195,
0.0204789281308526,0.0208092334232857,0.020891809746394,0.0209743860695023,
0.0211395387157189,0.021469844008152,0.0215524203312602,0.0216349966543685,
0.0218001493005851,0.0221304545930182,0.0224607598854513,0.0227910651778844,
0.0231213704703175,0.0232039467934258,0.023286523116534,0.0234516757627506,
0.0237819810551837,0.0241122863476168,0.0244425916400499,0.0251032022249161,
0.0252683548711327,0.0254335075173492,0.0257638128097823,0.0264244233946486,
0.0270850339795148,0.027745644564381,0.0284062551492472,0.0285714077954638,
0.0287365604416803,0.0290668657341134,0.0297274763189796,0.0303880869038458,
0.0310486974887121,0.0317093080735783,0.0320396133660114,0.0322047660122279,
0.0323699186584445,0.0330305292433107,0.0336911398281769,0.0343517504130431,
0.0346820557054762,0.0348472083516928,0.0349297846748011,0.0350123609979093,
0.0356729715827756,0.0363335821676418,0.036994192752508,0.0370767690756163,
0.0371593453987245,0.0373244980449411,0.0376548033373742,0.0383154139222404,
0.0386457192146735,0.0388108718608901,0.0389760245071066,0.0396366350919728,
0.039966940384406,0.0402972456768391,0.0404623983230556,0.0405449746461639,
0.0406275509692722,0.0409578562617053,0.0412881615541384,0.0416184668465715,
0.0419487721390046,0.0421139247852211,0.0421965011083294,0.0422377892698836,
0.0422790774314377),(0.,1.),.UNSPECIFIED.)
GEOMETRIC_REPRESENTATION_ITEM()
RATIONAL_B_SPLINE_SURFACE(((1.,0.923590675042016,1.),(1.,0.923572320945391,
1.),(1.,0.923553587090577,1.),(1.,0.923515495478205,1.),(1.,0.923496115237016,
1.),(1.,0.923436971524286,1.),(1.,0.923396205307423,1.),(1.,0.923269889059141,
1.),(1.,0.923180325181551,1.),(1.,0.922895385428438,1.),(1.,0.922683818431749,
1.),(1.,0.922215055006499,1.),(1.,0.921957857869856,1.),(1.,0.921393597668949,
1.),(1.,0.921086537396165,1.),(1.,0.920583987620736,1.),(1.,0.920409463147971,
1.),(1.,0.920136456599823,1.),(1.,0.920043583473226,1.),(1.,0.919853965179493,
1.),(1.,0.919757130552995,1.),(1.,0.919264385051497,1.),(1.,0.918842556687909,
1.),(1.,0.917485342839882,1.),(1.,0.916458802712932,1.),(1.,0.914690614339645,
1.),(1.,0.914063012700798,1.),(1.,0.913057237216573,1.),(1.,0.912711240257362,
1.),(1.,0.912175163335873,1.),(1.,0.911993623483323,1.),(1.,0.911624678363091,
1.),(1.,0.911437120441042,1.),(1.,0.909726149783902,1.),(1.,0.908041888239718,
1.),(1.,0.904290424256204,1.),(1.,0.90222325436422,1.),(1.,0.898787650803265,
1.),(1.,0.897586580689637,1.),(1.,0.896009931734525,1.),(1.,0.895690686714278,
1.),(1.,0.895045201490737,1.),(1.,0.894719248531258,1.),(1.,0.893731649644609,
1.),(1.,0.893060263975502,1.),(1.,0.889636937842127,1.),(1.,0.886685904879282,
1.),(1.,0.880320125821774,1.),(1.,0.876905428959452,1.),(1.,0.871403913130991,
1.),(1.,0.869506798646649,1.),(1.,0.867052723787093,1.),(1.,0.866557553196408,
1.),(1.,0.865560870035344,1.),(1.,0.865059173595903,1.),(1.,0.863543964995002,
1.),(1.,0.862520333878055,1.),(1.,0.857333970909859,1.),(1.,0.852966736393177,
1.),(1.,0.843775067927313,1.),(1.,0.838950667880686,1.),(1.,0.828820205567495,
1.),(1.,0.823514183332928,1.),(1.,0.812391307349727,1.),(1.,0.806574504385483,
1.),(1.,0.798962220591142,1.),(1.,0.797421706068384,1.),(1.,0.794315888151595,
1.),(1.,0.792749600433445,1.),(1.,0.788010186024153,1.),(1.,0.784796515809518,
1.),(1.,0.77498973461648,1.),(1.,0.768230990620621,1.),(1.,0.754249477539376,
1.),(1.,0.7470267311596,1.),(1.,0.732090338555257,1.),(1.,0.724376719977163,
1.),(1.,0.708426290764442,1.),(1.,0.700189512530531,1.),(1.,0.683154153538125,
1.),(1.,0.674355607127678,1.),(1.,0.664115385685685,1.),(1.,0.66297302996927,
1.),(1.,0.660682162177284,1.),(1.,0.659533241882799,1.),(1.,0.65607598168352,
1.),(1.,0.653757142047767,1.),(1.,0.646758317475323,1.),(1.,0.642036016956393,
1.),(1.,0.627697700195677,1.),(1.,0.61790996153014,1.),(1.,0.597870566155991,
1.),(1.,0.58761854570598,1.),(1.,0.566657940545553,1.),(1.,0.555948596069607,
1.),(1.,0.542299741359184,1.),(1.,0.539556972501121,1.),(1.,0.53404656747395,
1.),(1.,0.531276245933983,1.),(1.,0.522962675372791,1.),(1.,0.517409973114278,
1.),(1.,0.506307878837006,1.),(1.,0.500758405674242,1.),(1.,0.489694670444622,
1.),(1.,0.484180295137749,1.),(1.,0.473229585826254,1.),(1.,0.467793092024575,
1.),(1.,0.459740217505025,1.),(1.,0.457073035061414,1.),(1.,0.453104759629238,
1.),(1.,0.451787428134069,1.),(1.,0.449164897866363,1.),(1.,0.447859036145478,
1.),(1.,0.441385443166445,1.),(1.,0.436368154024372,1.),(1.,0.426750681610345,
1.),(1.,0.422150388759125,1.),(1.,0.413481583263519,1.),(1.,0.409412966405537,
1.),(1.,0.403813005360145,1.),(1.,0.402030377100019,1.),(1.,0.399497383040528,
1.),(1.,0.398676556272897,1.),(1.,0.397084562446663,1.),(1.,0.396315545546773,
1.),(1.,0.392617462025358,1.),(1.,0.390121311666049,1.),(1.,0.386146893571918,
1.),(1.,0.384668848565874,1.),(1.,0.382812549250897,1.),(1.,0.382434470212711,
1.),(1.,0.38268919558194,1.),(1.,0.382776371338327,1.),(1.,0.383022089646797,
1.),(1.,0.383180660969252,1.),(1.,0.383762017423613,1.),(1.,0.384290482158863,
1.),(1.,0.386285206501931,1.),(1.,0.388161225874796,1.),(1.,0.391136736543832,
1.),(1.,0.391763914323658,1.),(1.,0.393077192923473,1.),(1.,0.393761818570545,
1.),(1.,0.395895524715283,1.),(1.,0.397424386821021,1.),(1.,0.402298884562898,
1.),(1.,0.405931683845182,1.),(1.,0.413815239487506,1.),(1.,0.418066059410145,
1.),(1.,0.42706069079461,1.),(1.,0.431804585246568,1.),(1.,0.441681473676376,
1.),(1.,0.446814558722576,1.),(1.,0.453420699181124,1.),(1.,0.454748719848507,
1.),(1.,0.457413317151073,1.),(1.,0.458750495400507,1.),(1.,0.462774945482169,
1.),(1.,0.465475093536882,1.),(1.,0.473614842385458,1.),(1.,0.479093267976819,
1.),(1.,0.490102288950609,1.),(1.,0.495633034030675,1.),(1.,0.506709011958283,
1.),(1.,0.512254349645873,1.),(1.,0.528870329213323,1.),(1.,0.539918495566728,
1.),(1.,0.553602176080216,1.),(1.,0.556334955909364,1.),(1.,0.561765821980307,
1.),(1.,0.564466028627623,1.),(1.,0.572520418051971,1.),(1.,0.577828317778608,
1.),(1.,0.593564847150334,1.),(1.,0.603805896926842,1.),(1.,0.623792543125198,
1.),(1.,0.633538444526384,1.),(1.,0.652550041804049,1.),(1.,0.661815883466955,
1.),(1.,0.679885915223711,1.),(1.,0.6886901762844,1.),(1.,0.699418770951675,
1.),(1.,0.701551513084995,1.),(1.,0.705785767125964,1.),(1.,0.707884945612412,
1.),(1.,0.714129661070711,1.),(1.,0.718222393457039,1.),(1.,0.730296979845767,
1.),(1.,0.738075438054285,1.),(1.,0.753124875298064,1.),(1.,0.760395819580576,
1.),(1.,0.774458730322372,1.),(1.,0.781250671280861,1.),(1.,0.794378512232147,
1.),(1.,0.800714394746321,1.),(1.,0.809889696081597,1.),(1.,0.81289333920085,
1.),(1.,0.817317988310256,1.),(1.,0.81877983910783,1.),(1.,0.821667696260936,
1.),(1.,0.823094832962587,1.),(1.,0.830147792104091,1.),(1.,0.835525690411864,
1.),(1.,0.845780003457637,1.),(1.,0.85065638391852,1.),(1.,0.859929290650844,
1.),(1.,0.864325793621342,1.),(1.,0.870573221979968,1.),(1.,0.872597774409058,
1.),(1.,0.875548982801159,1.),(1.,0.876518446809548,1.),(1.,0.877951374397237,
1.),(1.,0.878425435719338,1.),(1.,0.879364277600825,1.),(1.,0.87982934145049,
1.),(1.,0.883976089465827,1.),(1.,0.887386226523438,1.),(1.,0.893695391832222,
1.),(1.,0.896594377182112,1.),(1.,0.901916757914401,1.),(1.,0.904340130964184,
1.),(1.,0.906816643976781,1.),(1.,0.907088077234898,1.),(1.,0.907622483818774,
1.),(1.,0.907885627787149,1.),(1.,0.908663109051759,1.),(1.,0.909165497176662,
1.),(1.,0.910626625009093,1.),(1.,0.911539350769517,1.),(1.,0.91410668701056,
1.),(1.,0.915590785243887,1.),(1.,0.917522428376818,1.),(1.,0.918117142015421,
1.),(1.,0.918940550747601,1.),(1.,0.919203618073144,1.),(1.,0.919707451070459,
1.),(1.,0.919946845560599,1.),(1.,0.921084971631206,1.),(1.,0.921808216030194,
1.),(1.,0.922671204445732,1.),(1.,0.922921678056867,1.),(1.,0.923355716047376,
1.),(1.,0.923539280063381,1.),(1.,0.923768924823362,1.),(1.,0.923837844568734,
1.),(1.,0.923930235120147,1.),(1.,0.923959199701402,1.),(1.,0.924013530789645,
1.),(1.,0.924038911854136,1.),(1.,0.924156810216913,1.),(1.,0.924221785724258,
1.),(1.,0.924299796558392,1.),(1.,0.924312823752853,1.),(1.,0.924291460660933,
1.),(1.,0.924257066663858,1.),(1.,0.924143360666746,1.),(1.,0.924064049018983,
1.),(1.,0.923911786837651,1.),(1.,0.923855468182103,1.),(1.,0.923762549501941,
1.),(1.,0.923730168815134,1.),(1.,0.923679465051457,1.),(1.,0.923662208277328,
1.),(1.,0.923626979380171,1.),(1.,0.923609029138641,1.),(1.,0.923590675042016,
1.)))
REPRESENTATION_ITEM('')
SURFACE()
);
#181=(
BOUNDED_SURFACE()
B_SPLINE_SURFACE(3,2,((#58139,#58140,#58141),(#58142,#58143,#58144),(#58145,
#58146,#58147),(#58148,#58149,#58150),(#58151,#58152,#58153),(#58154,#58155,
#58156),(#58157,#58158,#58159),(#58160,#58161,#58162),(#58163,#58164,#58165),
(#58166,#58167,#58168),(#58169,#58170,#58171),(#58172,#58173,#58174),(#58175,
#58176,#58177),(#58178,#58179,#58180),(#58181,#58182,#58183),(#58184,#58185,
#58186),(#58187,#58188,#58189),(#58190,#58191,#58192),(#58193,#58194,#58195),
(#58196,#58197,#58198),(#58199,#58200,#58201),(#58202,#58203,#58204),(#58205,
#58206,#58207),(#58208,#58209,#58210),(#58211,#58212,#58213),(#58214,#58215,
#58216),(#58217,#58218,#58219),(#58220,#58221,#58222),(#58223,#58224,#58225),
(#58226,#58227,#58228),(#58229,#58230,#58231),(#58232,#58233,#58234),(#58235,
#58236,#58237),(#58238,#58239,#58240),(#58241,#58242,#58243),(#58244,#58245,
#58246),(#58247,#58248,#58249),(#58250,#58251,#58252),(#58253,#58254,#58255),
(#58256,#58257,#58258),(#58259,#58260,#58261),(#58262,#58263,#58264),(#58265,
#58266,#58267),(#58268,#58269,#58270),(#58271,#58272,#58273),(#58274,#58275,
#58276),(#58277,#58278,#58279),(#58280,#58281,#58282),(#58283,#58284,#58285),
(#58286,#58287,#58288),(#58289,#58290,#58291),(#58292,#58293,#58294),(#58295,
#58296,#58297),(#58298,#58299,#58300),(#58301,#58302,#58303),(#58304,#58305,
#58306),(#58307,#58308,#58309),(#58310,#58311,#58312),(#58313,#58314,#58315),
(#58316,#58317,#58318),(#58319,#58320,#58321),(#58322,#58323,#58324),(#58325,
#58326,#58327),(#58328,#58329,#58330),(#58331,#58332,#58333),(#58334,#58335,
#58336),(#58337,#58338,#58339),(#58340,#58341,#58342),(#58343,#58344,#58345),
(#58346,#58347,#58348),(#58349,#58350,#58351),(#58352,#58353,#58354),(#58355,
#58356,#58357),(#58358,#58359,#58360),(#58361,#58362,#58363),(#58364,#58365,
#58366),(#58367,#58368,#58369),(#58370,#58371,#58372),(#58373,#58374,#58375),
(#58376,#58377,#58378),(#58379,#58380,#58381),(#58382,#58383,#58384),(#58385,
#58386,#58387),(#58388,#58389,#58390),(#58391,#58392,#58393),(#58394,#58395,
#58396),(#58397,#58398,#58399),(#58400,#58401,#58402),(#58403,#58404,#58405),
(#58406,#58407,#58408),(#58409,#58410,#58411),(#58412,#58413,#58414),(#58415,
#58416,#58417),(#58418,#58419,#58420),(#58421,#58422,#58423),(#58424,#58425,
#58426),(#58427,#58428,#58429),(#58430,#58431,#58432),(#58433,#58434,#58435),
(#58436,#58437,#58438),(#58439,#58440,#58441),(#58442,#58443,#58444),(#58445,
#58446,#58447),(#58448,#58449,#58450),(#58451,#58452,#58453),(#58454,#58455,
#58456),(#58457,#58458,#58459),(#58460,#58461,#58462),(#58463,#58464,#58465),
(#58466,#58467,#58468),(#58469,#58470,#58471),(#58472,#58473,#58474),(#58475,
#58476,#58477),(#58478,#58479,#58480),(#58481,#58482,#58483),(#58484,#58485,
#58486),(#58487,#58488,#58489),(#58490,#58491,#58492),(#58493,#58494,#58495),
(#58496,#58497,#58498),(#58499,#58500,#58501),(#58502,#58503,#58504),(#58505,
#58506,#58507),(#58508,#58509,#58510),(#58511,#58512,#58513),(#58514,#58515,
#58516),(#58517,#58518,#58519),(#58520,#58521,#58522),(#58523,#58524,#58525),
(#58526,#58527,#58528),(#58529,#58530,#58531),(#58532,#58533,#58534),(#58535,
#58536,#58537),(#58538,#58539,#58540),(#58541,#58542,#58543),(#58544,#58545,
#58546),(#58547,#58548,#58549),(#58550,#58551,#58552),(#58553,#58554,#58555),
(#58556,#58557,#58558),(#58559,#58560,#58561),(#58562,#58563,#58564),(#58565,
#58566,#58567),(#58568,#58569,#58570),(#58571,#58572,#58573),(#58574,#58575,
#58576),(#58577,#58578,#58579),(#58580,#58581,#58582),(#58583,#58584,#58585),
(#58586,#58587,#58588),(#58589,#58590,#58591),(#58592,#58593,#58594),(#58595,
#58596,#58597),(#58598,#58599,#58600),(#58601,#58602,#58603),(#58604,#58605,
#58606),(#58607,#58608,#58609),(#58610,#58611,#58612),(#58613,#58614,#58615),
(#58616,#58617,#58618),(#58619,#58620,#58621),(#58622,#58623,#58624),(#58625,
#58626,#58627),(#58628,#58629,#58630),(#58631,#58632,#58633),(#58634,#58635,
#58636),(#58637,#58638,#58639),(#58640,#58641,#58642),(#58643,#58644,#58645),
(#58646,#58647,#58648),(#58649,#58650,#58651),(#58652,#58653,#58654),(#58655,
#58656,#58657),(#58658,#58659,#58660),(#58661,#58662,#58663),(#58664,#58665,
#58666),(#58667,#58668,#58669),(#58670,#58671,#58672),(#58673,#58674,#58675),
(#58676,#58677,#58678),(#58679,#58680,#58681),(#58682,#58683,#58684),(#58685,
#58686,#58687),(#58688,#58689,#58690),(#58691,#58692,#58693),(#58694,#58695,
#58696),(#58697,#58698,#58699),(#58700,#58701,#58702),(#58703,#58704,#58705),
(#58706,#58707,#58708),(#58709,#58710,#58711),(#58712,#58713,#58714),(#58715,
#58716,#58717),(#58718,#58719,#58720),(#58721,#58722,#58723),(#58724,#58725,
#58726),(#58727,#58728,#58729),(#58730,#58731,#58732),(#58733,#58734,#58735),
(#58736,#58737,#58738),(#58739,#58740,#58741),(#58742,#58743,#58744),(#58745,
#58746,#58747),(#58748,#58749,#58750),(#58751,#58752,#58753),(#58754,#58755,
#58756),(#58757,#58758,#58759),(#58760,#58761,#58762),(#58763,#58764,#58765),
(#58766,#58767,#58768),(#58769,#58770,#58771),(#58772,#58773,#58774),(#58775,
#58776,#58777),(#58778,#58779,#58780),(#58781,#58782,#58783),(#58784,#58785,
#58786),(#58787,#58788,#58789),(#58790,#58791,#58792),(#58793,#58794,#58795),
(#58796,#58797,#58798),(#58799,#58800,#58801),(#58802,#58803,#58804),(#58805,
#58806,#58807),(#58808,#58809,#58810),(#58811,#58812,#58813),(#58814,#58815,
#58816),(#58817,#58818,#58819),(#58820,#58821,#58822),(#58823,#58824,#58825),
(#58826,#58827,#58828),(#58829,#58830,#58831),(#58832,#58833,#58834),(#58835,
#58836,#58837),(#58838,#58839,#58840)),.UNSPECIFIED.,.F.,.F.,.F.)
B_SPLINE_SURFACE_WITH_KNOTS((4,2,2,2,2,2,2,2,2,2,2,2,2,2,2,2,2,2,2,2,2,
2,2,2,2,2,2,2,2,2,2,2,2,2,2,2,2,2,2,2,2,2,2,2,2,2,2,2,2,2,2,2,2,2,2,2,2,
2,2,2,2,2,2,2,2,2,2,2,2,2,2,2,2,2,2,2,2,2,2,2,2,2,2,2,2,2,2,2,2,2,2,2,2,
2,2,2,2,2,2,2,2,2,2,2,2,2,2,2,2,2,2,2,2,2,2,2,4),(3,3),(0.0290103847129019,
0.0295538338054091,0.0298255583516626,0.029893489488226,0.0299614206247894,
0.0300972828979162,0.0306407319904233,0.0311841810829305,0.031455905629184,
0.0315917679023108,0.0316596990388742,0.0317276301754376,0.0322710792679447,
0.0328145283604518,0.033357977452959,0.0334938397260857,0.0335617708626491,
0.0336297019992125,0.0339014265454661,0.0344448756379732,0.0349883247304803,
0.0352600492767339,0.0353279804132973,0.0353959115498607,0.0355317738229875,
0.0360752229154946,0.0366186720080017,0.0368903965542553,0.0370262588273821,
0.0371621211005088,0.037705570193016,0.0382490192855231,0.0387924683780302,
0.038928330651157,0.0389962617877204,0.0390641929242838,0.0393359174705374,
0.0398793665630445,0.0404228156555516,0.0406945402018052,0.0408304024749319,
0.0409662647480587,0.0415097138405659,0.042053162933073,0.0425966120255801,
0.0428683365718337,0.0430041988449605,0.0431400611180872,0.0436835102105944,
0.0442269593031015,0.0447704083956086,0.044838339532172,0.0449062706687354,
0.0450421329418622,0.0453138574881158,0.0458573065806229,0.04640075567313,
0.0465366179462568,0.0466045490828202,0.0466724802193836,0.0469442047656371,
0.0474876538581443,0.0480311029506514,0.0480990340872148,0.0481669652237782,
0.0483028274969049,0.0485745520431585,0.0491180011356656,0.0493897256819192,
0.049525587955046,0.0496614502281728,0.0502048993206799,0.050748348413187,
0.0512917975056942,0.0514276597788209,0.0515635220519477,0.0518352465982013,
0.0523786956907084,0.0529221447832155,0.0534655938757227,0.0536014561488494,
0.0537373184219762,0.0540090429682298,0.0541449052413566,0.0542807675144833,
0.0545524920607369,0.055095941153244,0.0556393902457512,0.0559111147920047,
0.0560469770651315,0.0561149082016949,0.0561828393382583,0.0567262884307654,
0.0572697375232725,0.0578131866157797,0.0579490488889065,0.0580849111620332,
0.0583566357082868,0.0589000848007939,0.0594435338933011,0.0597152584395546,
0.059783189576118,0.0598511207126814,0.0599869829858082,0.0605304320783153,
0.0610738811708224,0.061345605717076,0.0614814679902028,0.0615493991267662,
0.0616173302633296,0.0621607793558367,0.0627042284483438,0.0632476775408509,
0.0633156086774143,0.0633835398139777,0.0635194020871045,0.0637911266333581),
(-1.72788130968728E-6,1.),.UNSPECIFIED.)
GEOMETRIC_REPRESENTATION_ITEM()
RATIONAL_B_SPLINE_SURFACE(((1.00000094197663,0.727418595914212,1.),(1.00000094277455,
0.727187698108613,1.),(1.00000094430839,0.726743850528363,1.),(1.00000094768065,
0.725768013810579,1.),(1.00000094898323,0.725391083151896,1.),(1.0000009508298,
0.724856736725869,1.),(1.0000009512101,0.72474668983897,1.),(1.00000095199009,
0.724520983240094,1.),(1.00000095239004,0.724405249820312,1.),(1.00000095361912,
0.72404958662569,1.),(1.00000095447751,0.72380119340961,1.),(1.00000095895618,
0.72250519314825,1.),(1.00000096313739,0.721295268540489,1.),(1.00000097247495,
0.718593243085756,1.),(1.00000097763181,0.717100995140168,1.),(1.00000098591273,
0.714704729614825,1.),(1.00000098876372,0.713879733273474,1.),(1.00000099314999,
0.712610471336212,1.),(1.00000099463035,0.712182096269172,1.),(1.00000099687479,
0.711532620097953,1.),(1.00000099762691,0.711314976265769,1.),(1.00000099913852,
0.710877561277227,1.),(1.00000099989841,0.710657670723553,1.),(1.00000100674924,
0.708675232626428,1.),(1.00000101294924,0.706881126980666,1.),(1.00000102520803,
0.703333782029864,1.),(1.00000103126738,0.701580377140293,1.),(1.00000104286114,
0.698225469884114,1.),(1.00000104839618,0.696623786464909,1.),(1.00000105472174,
0.694793346516954,1.),(1.00000105595707,0.694435878132859,1.),(1.00000105775998,
0.693914167092214,1.),(1.00000105835303,0.693742555644265,1.),(1.00000105951902,
0.693405150014371,1.),(1.00000106009194,0.693239364605067,1.),(1.00000106290441,
0.692425515296011,1.),(1.00000106498762,0.69182269211634,1.),(1.0000010706726,
0.690177620996682,1.),(1.00000107370956,0.689298810815767,1.),(1.00000107793992,
0.688074663091584,1.),(1.00000107913354,0.687729261620368,1.),(1.00000107928995,
0.687684002572033,1.),(1.00000107906974,0.68774772463205,1.),(1.0000010784276,
0.687933540851868,1.),(1.00000107828083,0.687976012571821,1.),(1.00000107794993,
0.688071765808802,1.),(1.00000107776568,0.688125082395367,1.),(1.00000107715803,
0.688300919176998,1.),(1.0000010766791,0.688439508022508,1.),(1.00000107391216,
0.689240182223478,1.),(1.00000107050605,0.690225813636976,1.),(1.0000010612487,
0.692904628638751,1.),(1.00000105539763,0.694597763995586,1.),(1.00000104476396,
0.697674847330772,1.),(1.0000010409101,0.69879004455908,1.),(1.00000103466414,
0.700597449749866,1.),(1.00000103250463,0.70122234989242,1.),(1.0000010280305,
0.702517037582702,1.),(1.00000102571495,0.703187092703321,1.),(1.000001013759,
0.706646805799464,1.),(1.00000100311034,0.709728226570205,1.),(1.00000097986549,
0.716454630491264,1.),(1.00000096726932,0.720099604613224,1.),(1.0000009403451,
0.727890713049425,1.),(1.00000092601706,0.732036842434526,1.),(1.00000090715593,
0.73749472092308,1.),(1.00000090333614,0.738600061506044,1.),(1.00000089753751,
0.74027801909495,1.),(1.00000089559232,0.740840901529955,1.),(1.00000089168822,
0.741970640142475,1.),(1.00000088972839,0.742537758394899,1.),(1.00000087989184,
0.745384178455298,1.),(1.00000087190293,0.74769594190517,1.),(1.00000084763024,
0.754719772705337,1.),(1.00000083104128,0.75952014802879,1.),(1.00000079730879,
0.769281378915179,1.),(1.0000007801649,0.774242333982382,1.),(1.00000075421114,
0.781752620154195,1.),(1.00000074552009,0.784267564565214,1.),(1.00000073244522,
0.788051059686649,1.),(1.00000072808055,0.789314072476293,1.),(1.00000071934197,
0.791842771982262,1.),(1.00000071496481,0.793109396640888,1.),(1.00000069316053,
0.799418938941215,1.),(1.00000067591145,0.804410334492118,1.),(1.00000064200496,
0.81422191448303,1.),(1.00000062534704,0.819042245139272,1.),(1.00000059281998,
0.828454657464615,1.),(1.00000057695027,0.833046904849106,1.),(1.00000055389332,
0.839718934283668,1.),(1.00000054633241,0.841906847587564,1.),(1.00000053519969,
0.845128341016523,1.),(1.00000053152358,0.846192104502361,1.),(1.00000052424476,
0.848298387636058,1.),(1.00000052065556,0.849337000883416,1.),(1.00000050297139,
0.854454300511256,1.),(1.00000048965526,0.858307611902219,1.),(1.00000046484844,
0.865486003998872,1.),(1.00000045335714,0.868811260812436,1.),(1.00000043240277,
0.874874863226948,1.),(1.00000042293878,0.87761347324732,1.),(1.00000041358206,
0.880321043280489,1.),(1.00000041256186,0.880616260389349,1.),(1.000000410564,
0.881194384595568,1.),(1.00000040958579,0.88147745358052,1.),(1.00000040671335,
0.882308655927517,1.),(1.00000040488134,0.882838786291053,1.),(1.00000039963509,
0.884356904421394,1.),(1.0000003964705,0.885272645328228,1.),(1.00000038798589,
0.887727851822622,1.),(1.00000038367343,0.888975755802617,1.),(1.00000037782766,
0.890667356064376,1.),(1.00000037629401,0.891111152415122,1.),(1.00000037620463,
0.891137016136596,1.),(1.00000037627829,0.891115701568441,1.),(1.00000037652826,
0.891043367082923,1.),(1.00000037663496,0.891012491709624,1.),(1.00000037689415,
0.890937487212343,1.),(1.00000037704668,0.890893349204927,1.),(1.000000377923,
0.890639767831579,1.),(1.00000037898762,0.890331698329217,1.),(1.00000038323813,
0.889101720659685,1.),(1.00000038747899,0.887874535749084,1.),(1.00000039863949,
0.884645001760937,1.),(1.00000040555943,0.882642567397013,1.),(1.00000041480412,
0.879967413714825,1.),(1.00000041585162,0.879664298847342,1.),(1.0000004179871,
0.879046350923129,1.),(1.00000041907386,0.878731873543084,1.),(1.00000042238551,
0.877773573685649,1.),(1.00000042466376,0.877114313314577,1.),(1.00000043170345,
0.875077226776075,1.),(1.0000004366697,0.873640133605505,1.),(1.00000045234131,
0.869105213673524,1.),(1.00000046381801,0.865784181073996,1.),(1.00000048242379,
0.860400193058436,1.),(1.00000048885792,0.858538338109017,1.),(1.00000049884142,
0.855649395902143,1.),(1.00000050222466,0.854670383221197,1.),(1.00000050909947,
0.852681008046092,1.),(1.00000051259291,0.85167010350086,1.),(1.00000053030494,
0.846544742360046,1.),(1.00000054512528,0.842256156889833,1.),(1.00000057583858,
0.833368594516816,1.),(1.00000059173227,0.828769411125496,1.),(1.00000062439208,
0.81931858601259,1.),(1.00000064115875,0.814466783467411,1.),(1.00000066254231,
0.808278986583686,1.),(1.00000066684028,0.807035275537529,1.),(1.00000067547568,
0.804536435116907,1.),(1.00000067980235,0.803284419130001,1.),(1.00000069278865,
0.799526552678708,1.),(1.00000070146116,0.797016971575482,1.),(1.00000072748197,
0.789487284521765,1.),(1.00000074483388,0.784466133705224,1.),(1.00000077932073,
0.77448661498812,1.),(1.00000079645607,0.76952813210456,1.),(1.00000083026845,
0.759743783371996,1.),(1.00000084694591,0.754917798013528,1.),(1.00000086733813,
0.749016865533183,1.),(1.00000087139383,0.74784326137115,1.),(1.00000087942808,
0.745518375589863,1.),(1.00000088341008,0.744366098414126,1.),(1.00000089524472,
0.74094148805281,1.),(1.00000090298606,0.738701364424776,1.),(1.00000091435093,
0.735412692841522,1.),(1.00000091809802,0.734328390689723,1.),(1.0000009255056,
0.732184846770628,1.),(1.00000092916803,0.73112504109884,1.),(1.00000093998345,
0.727995364774212,1.),(1.00000094697548,0.725972070020501,1.),(1.00000096726284,
0.720101479727836,1.),(1.00000097986941,0.7164534949861,1.),(1.00000100306537,
0.709741240019853,1.),(1.00000101365467,0.706676997713043,1.),(1.00000102789253,
0.702556963714663,1.),(1.00000103236417,0.70126299759053,1.),(1.00000103864392,
0.69944581371337,1.),(1.00000104066589,0.698860712318966,1.),(1.00000104358993,
0.698014577829412,1.),(1.0000010445468,0.697737688580098,1.),(1.00000104641865,
0.697196027550747,1.),(1.0000010473343,0.696931065246606,1.),(1.00000105539338,
0.69459899336011,1.),(1.00000106126382,0.692900253988097,1.),(1.00000107051798,
0.690222363085288,1.),(1.00000107390152,0.689243262016709,1.),(1.00000107830538,
0.687968908792342,1.),(1.00000107932556,0.687673698960344,1.),(1.00000107921905,
0.687704517724663,1.),(1.00000107912874,0.687730650887494,1.),(1.00000107881281,
0.687822073848177,1.),(1.00000107858785,0.687887170866826,1.),(1.00000107772176,
0.688137791537803,1.),(1.00000107688939,0.688378656929289,1.),(1.00000107370219,
0.689300942103724,1.),(1.00000107065772,0.690181924746401,1.),(1.0000010631148,
0.692364632289744,1.),(1.00000105861603,0.693666449756497,1.),(1.00000105105817,
0.695853481128863,1.),(1.00000104840388,0.696621557639583,1.),(1.00000104494645,
0.697622039003881,1.),(1.00000104424769,0.69782424123167,1.),(1.00000104284087,
0.698231334628583,1.),(1.00000104213239,0.698436349669935,1.),(1.00000103999302,
0.699055423277568,1.),(1.00000103854822,0.699473508202277,1.),(1.00000103124828,
0.701585903182804,1.),(1.0000010251674,0.703345538833113,1.),(1.00000101291955,
0.706889718420206,1.),(1.00000100675193,0.708674454447466,1.),(1.00000099770163,
0.711293356482619,1.),(1.00000099471813,0.712156696596124,1.),(1.00000099032442,
0.713428111831309,1.),(1.00000098887343,0.713847987019327,1.),(1.00000098672121,
0.71447077836442,1.),(1.00000098600749,0.714677308358767,1.),(1.00000098459043,
0.715087365979716,1.),(1.00000098388775,0.715290702390871,1.),(1.00000097761853,
0.717104837900671,1.),(1.00000097243836,0.718603831103779,1.),(1.00000096309419,
0.721307768765821,1.),(1.00000095892963,0.722512874625052,1.),(1.00000095181024,
0.724573025448519,1.),(1.00000094885502,0.72542818325312,1.),(1.00000094630728,
0.72616542721051,1.),(1.00000094603498,0.726244223849717,1.),(1.00000094551225,
0.726395485734667,1.),(1.0000009452617,0.726467988945064,1.),(1.00000094454426,
0.726675594380443,1.),(1.00000094411234,0.726800580220694,1.),(1.00000094295592,
0.727135216917278,1.),(1.00000094237078,0.727304540475937,1.),(1.00000094197156,
0.72742006218996,1.)))
REPRESENTATION_ITEM('')
SURFACE()
);
#182=(
BOUNDED_SURFACE()
B_SPLINE_SURFACE(3,2,((#58863,#58864,#58865),(#58866,#58867,#58868),(#58869,
#58870,#58871),(#58872,#58873,#58874),(#58875,#58876,#58877),(#58878,#58879,
#58880),(#58881,#58882,#58883),(#58884,#58885,#58886),(#58887,#58888,#58889),
(#58890,#58891,#58892),(#58893,#58894,#58895),(#58896,#58897,#58898),(#58899,
#58900,#58901),(#58902,#58903,#58904),(#58905,#58906,#58907),(#58908,#58909,
#58910),(#58911,#58912,#58913),(#58914,#58915,#58916),(#58917,#58918,#58919),
(#58920,#58921,#58922),(#58923,#58924,#58925),(#58926,#58927,#58928),(#58929,
#58930,#58931),(#58932,#58933,#58934),(#58935,#58936,#58937),(#58938,#58939,
#58940),(#58941,#58942,#58943),(#58944,#58945,#58946),(#58947,#58948,#58949),
(#58950,#58951,#58952),(#58953,#58954,#58955),(#58956,#58957,#58958),(#58959,
#58960,#58961),(#58962,#58963,#58964)),.UNSPECIFIED.,.F.,.F.,.F.)
B_SPLINE_SURFACE_WITH_KNOTS((4,2,2,2,2,2,2,2,2,2,2,2,2,2,2,2,4),(3,3),(1.57074065524005,
1.71325309204606,1.85570985729722,1.99816662254838,2.14062338779954,2.28308015305071,
2.42553691830187,2.56799368355303,2.71045044880419,2.85290721405535,2.99536397930651,
3.13782074455768,3.28027750980884,3.42273427506,3.56519104031116,3.70764780556232,
3.85010457081348),(0.,1.00005567155485),.UNSPECIFIED.)
GEOMETRIC_REPRESENTATION_ITEM()
RATIONAL_B_SPLINE_SURFACE(((1.,0.707079920138348,1.00003261463259),(1.,
0.716086689006554,1.00003161179093),(1.,0.724920009118845,1.0000306282616),
(1.,0.742104597504674,1.00002871487609),(1.,0.75045582409158,1.00002778502455),
(1.,0.76656425844358,1.00002599146138),(1.,0.774321529260281,1.00002512774272),
(1.,0.789143223578738,1.00002347744919),(1.,0.796207699042566,1.00002269086852),
(1.,0.809559621853178,1.00002120422392),(1.,0.815847110870319,1.00002050415534),
(1.,0.827574222198235,1.00001919842229),(1.,0.833013877192258,1.00001859275419),
(1.,0.842986797390786,1.00001748233824),(1.,0.847520087651854,1.00001697758761),
(1.,0.855633281940707,1.00001607423933),(1.,0.859213204604135,1.0000156756396),
(1.,0.865383603626224,1.00001498860819),(1.,0.867974093167104,1.00001470017503),
(1.,0.872140077171102,1.00001423632141),(1.,0.873715580073823,1.00001406090002),
(1.,0.875836267380118,1.0000138247761),(1.,0.876381455942513,1.00001376407311),
(1.,0.876436251233421,1.00001375797203),(1.,0.875945858068014,1.00001381257393),
(1.,0.873934231083751,1.00001403655474),(1.,0.872412993324182,1.00001420593408),
(1.,0.868354473220934,1.00001465782233),(1.,0.865817182673778,1.00001494033215),
(1.,0.859751567664865,1.00001561569659),(1.,0.856223230287758,1.00001600855264),
(1.,0.848211026545572,1.00001690065632),(1.,0.843727317065168,1.00001739988648),
(1.,0.838788701080504,1.00001794976734)))
REPRESENTATION_ITEM('')
SURFACE()
);
#183=(
BOUNDED_SURFACE()
B_SPLINE_SURFACE(3,2,((#59053,#59054,#59055),(#59056,#59057,#59058),(#59059,
#59060,#59061),(#59062,#59063,#59064),(#59065,#59066,#59067),(#59068,#59069,
#59070),(#59071,#59072,#59073),(#59074,#59075,#59076),(#59077,#59078,#59079),
(#59080,#59081,#59082),(#59083,#59084,#59085),(#59086,#59087,#59088),(#59089,
#59090,#59091),(#59092,#59093,#59094),(#59095,#59096,#59097),(#59098,#59099,
#59100),(#59101,#59102,#59103),(#59104,#59105,#59106),(#59107,#59108,#59109),
(#59110,#59111,#59112),(#59113,#59114,#59115),(#59116,#59117,#59118),(#59119,
#59120,#59121),(#59122,#59123,#59124),(#59125,#59126,#59127),(#59128,#59129,
#59130),(#59131,#59132,#59133),(#59134,#59135,#59136),(#59137,#59138,#59139),
(#59140,#59141,#59142),(#59143,#59144,#59145),(#59146,#59147,#59148),(#59149,
#59150,#59151),(#59152,#59153,#59154),(#59155,#59156,#59157),(#59158,#59159,
#59160),(#59161,#59162,#59163),(#59164,#59165,#59166),(#59167,#59168,#59169),
(#59170,#59171,#59172),(#59173,#59174,#59175),(#59176,#59177,#59178),(#59179,
#59180,#59181),(#59182,#59183,#59184),(#59185,#59186,#59187),(#59188,#59189,
#59190),(#59191,#59192,#59193),(#59194,#59195,#59196),(#59197,#59198,#59199),
(#59200,#59201,#59202)),.UNSPECIFIED.,.F.,.F.,.F.)
B_SPLINE_SURFACE_WITH_KNOTS((4,2,2,2,2,2,2,2,2,2,2,2,2,2,2,2,2,2,2,2,2,
2,2,2,4),(3,3),(0.0168736397610245,0.0173205003855472,0.0177673610100698,
0.0178790761662005,0.0179907913223312,0.0182142216345925,0.0186610822591151,
0.0191079428836378,0.0195548035081605,0.0197782338204218,0.0198899489765524,
0.0200016641326831,0.0204485247572058,0.0205602399133364,0.0206719550694671,
0.0208953853817284,0.0213422460062511,0.0217891066307737,0.0222359672552964,
0.0224593975675577,0.0225711127236884,0.022682827879819,0.0231296885043417,
0.0235765491288643,0.024023409753387),(0.,1.),.UNSPECIFIED.)
GEOMETRIC_REPRESENTATION_ITEM()
RATIONAL_B_SPLINE_SURFACE(((1.,0.676185655324359,1.),(1.,0.67630322416838,
1.),(1.,0.676584997615303,1.),(1.,0.67743451044132,1.),(1.,0.678002280027087,
1.),(1.,0.678863512103858,1.),(1.,0.679043447440726,1.),(1.,0.679417253471516,
1.),(1.,0.679610743089326,1.),(1.,0.680209528048005,1.),(1.,0.680633128730709,
1.),(1.,0.681966035229257,1.),(1.,0.682937305222825,1.),(1.,0.684989680316945,
1.),(1.,0.686070826789687,1.),(1.,0.688291564262565,1.),(1.,0.689431193575673,
1.),(1.,0.691148055248714,1.),(1.,0.691721597513498,1.),(1.,0.692579366019322,
1.),(1.,0.692864861918766,1.),(1.,0.693432626773667,1.),(1.,0.693715104487649,
1.),(1.,0.695118751522096,1.),(1.,0.696213531941737,1.),(1.,0.697521120294898,
1.),(1.,0.697779622667988,1.),(1.,0.698289874383767,1.),(1.,0.698541099245874,
1.),(1.,0.699282339144899,1.),(1.,0.699759908934221,1.),(1.,0.701137406672921,
1.),(1.,0.701981987768826,1.),(1.,0.703498354563225,1.),(1.,0.704170174913113,
1.),(1.,0.705319738998922,1.),(1.,0.705797505956189,1.),(1.,0.706354933867263,
1.),(1.,0.706514227956655,1.),(1.,0.706711865981927,1.),(1.,0.706770862676804,
1.),(1.,0.70687484959442,1.),(1.,0.706919686161599,1.),(1.,0.707108074228766,
1.),(1.,0.707144248395913,1.),(1.,0.706992159157227,1.),(1.,0.706803894595462,
1.),(1.,0.706210527095295,1.),(1.,0.705805464605862,1.),(1.,0.705297251064667,
1.)))
REPRESENTATION_ITEM('')
SURFACE()
);
#184=(
BOUNDED_SURFACE()
B_SPLINE_SURFACE(3,2,((#59299,#59300,#59301),(#59302,#59303,#59304),(#59305,
#59306,#59307),(#59308,#59309,#59310),(#59311,#59312,#59313),(#59314,#59315,
#59316),(#59317,#59318,#59319),(#59320,#59321,#59322),(#59323,#59324,#59325),
(#59326,#59327,#59328),(#59329,#59330,#59331),(#59332,#59333,#59334),(#59335,
#59336,#59337),(#59338,#59339,#59340),(#59341,#59342,#59343),(#59344,#59345,
#59346),(#59347,#59348,#59349),(#59350,#59351,#59352),(#59353,#59354,#59355),
(#59356,#59357,#59358),(#59359,#59360,#59361),(#59362,#59363,#59364),(#59365,
#59366,#59367),(#59368,#59369,#59370),(#59371,#59372,#59373),(#59374,#59375,
#59376),(#59377,#59378,#59379),(#59380,#59381,#59382),(#59383,#59384,#59385),
(#59386,#59387,#59388),(#59389,#59390,#59391),(#59392,#59393,#59394),(#59395,
#59396,#59397),(#59398,#59399,#59400),(#59401,#59402,#59403),(#59404,#59405,
#59406),(#59407,#59408,#59409),(#59410,#59411,#59412),(#59413,#59414,#59415),
(#59416,#59417,#59418),(#59419,#59420,#59421),(#59422,#59423,#59424),(#59425,
#59426,#59427),(#59428,#59429,#59430),(#59431,#59432,#59433),(#59434,#59435,
#59436),(#59437,#59438,#59439),(#59440,#59441,#59442),(#59443,#59444,#59445),
(#59446,#59447,#59448),(#59449,#59450,#59451),(#59452,#59453,#59454),(#59455,
#59456,#59457),(#59458,#59459,#59460),(#59461,#59462,#59463),(#59464,#59465,
#59466),(#59467,#59468,#59469),(#59470,#59471,#59472),(#59473,#59474,#59475),
(#59476,#59477,#59478),(#59479,#59480,#59481),(#59482,#59483,#59484),(#59485,
#59486,#59487),(#59488,#59489,#59490),(#59491,#59492,#59493),(#59494,#59495,
#59496),(#59497,#59498,#59499),(#59500,#59501,#59502),(#59503,#59504,#59505),
(#59506,#59507,#59508),(#59509,#59510,#59511),(#59512,#59513,#59514),(#59515,
#59516,#59517),(#59518,#59519,#59520),(#59521,#59522,#59523),(#59524,#59525,
#59526),(#59527,#59528,#59529),(#59530,#59531,#59532),(#59533,#59534,#59535),
(#59536,#59537,#59538),(#59539,#59540,#59541),(#59542,#59543,#59544),(#59545,
#59546,#59547),(#59548,#59549,#59550),(#59551,#59552,#59553),(#59554,#59555,
#59556),(#59557,#59558,#59559),(#59560,#59561,#59562),(#59563,#59564,#59565),
(#59566,#59567,#59568),(#59569,#59570,#59571),(#59572,#59573,#59574),(#59575,
#59576,#59577),(#59578,#59579,#59580),(#59581,#59582,#59583),(#59584,#59585,
#59586)),.UNSPECIFIED.,.F.,.F.,.F.)
B_SPLINE_SURFACE_WITH_KNOTS((4,2,2,2,2,2,2,2,2,2,2,2,2,2,2,2,2,2,2,2,2,
2,2,2,2,2,2,2,2,2,2,2,2,2,2,2,2,2,2,2,2,2,2,2,2,2,2,4),(3,3),(0.0133656719252939,
0.0137531204885812,0.0139468447702248,0.0140437069110466,0.0140921379814575,
0.0141405690518684,0.0145280176151557,0.0149154661784429,0.0153029147417302,
0.0154966390233738,0.0155935011641956,0.0156419322346065,0.0156903633050174,
0.0160778118683047,0.0164652604315919,0.0168527089948792,0.0170464332765228,
0.0171432954173446,0.0172401575581664,0.0176276061214537,0.0180150546847409,
0.0184025032480282,0.0187899518113154,0.0191774003746027,0.0192742625154245,
0.0193711246562463,0.0195648489378899,0.0199522975011772,0.020049159641999,
0.0201460217828208,0.0203397460644644,0.0207271946277517,0.0211146431910389,
0.0215020917543262,0.0218895403176134,0.0222769888809007,0.0224707131625443,
0.0225675753033661,0.0226644374441879,0.0234393345707625,0.0238267831340497,
0.024214231697337,0.0246016802606242,0.0249891288239115,0.0250859909647333,
0.0251828531055551,0.0253765773871987,0.025764025950486),(0.,1.),
 .UNSPECIFIED.)
GEOMETRIC_REPRESENTATION_ITEM()
RATIONAL_B_SPLINE_SURFACE(((1.,0.9140223922261,1.),(1.,0.915030492709283,
1.),(1.,0.915858639583001,1.),(1.,0.916817715499207,1.),(1.,0.917090200413126,
1.),(1.,0.917426174788986,1.),(1.,0.917526038338742,1.),(1.,0.917657375959307,
1.),(1.,0.917698072660668,1.),(1.,0.917773091161791,1.),(1.,0.917807443115215,
1.),(1.,0.918088314388304,1.),(1.,0.918136915427419,1.),(1.,0.917843376479416,
1.),(1.,0.917501223822225,1.),(1.,0.916433977111706,1.),(1.,0.915708876551461,
1.),(1.,0.914337422509701,1.),(1.,0.913832945692125,1.),(1.,0.913005446344792,
1.),(1.,0.912717814337712,1.),(1.,0.912268679644456,1.),(1.,0.912115982606894,
1.),(1.,0.911805397365888,1.),(1.,0.911647430343649,1.),(1.,0.910201898284099,
1.),(1.,0.908747768522694,1.),(1.,0.905525061106013,1.),(1.,0.903756442170294,
1.),(1.,0.899923635221016,1.),(1.,0.897859417630057,1.),(1.,0.89455261711194,
1.),(1.,0.893415243056036,1.),(1.,0.891657695042151,1.),(1.,0.891062827486455,
1.),(1.,0.889859964219412,1.),(1.,0.889251636022491,1.),(1.,0.886176395534851,
1.),(1.,0.883608843556552,1.),(1.,0.878278885688577,1.),(1.,0.875516441111426,
1.),(1.,0.869813110038265,1.),(1.,0.86687219535343,1.),(1.,0.860825971449527,
1.),(1.,0.857720640581297,1.),(1.,0.851357997915466,1.),(1.,0.848100668446161,
1.),(1.,0.843941117270504,1.),(1.,0.843104810668739,1.),(1.,0.841423576195933,
1.),(1.,0.840578661667794,1.),(1.,0.838036046535061,1.),(1.,0.83632889783711,
1.),(1.,0.831173872679246,1.),(1.,0.827692420000005,1.),(1.,0.823293277529827,
1.),(1.,0.822411082406562,1.),(1.,0.820642174664206,1.),(1.,0.819755100414045,
1.),(1.,0.817090095259101,1.),(1.,0.815309850858671,1.),(1.,0.809961218322665,
1.),(1.,0.806384920527092,1.),(1.,0.799226404991901,1.),(1.,0.79564417490575,
1.),(1.,0.788489405141087,1.),(1.,0.784916853795515,1.),(1.,0.777797878098423,
1.),(1.,0.774251441980022,1.),(1.,0.767202304821984,1.),(1.,0.763699591208166,
1.),(1.,0.758492675884238,1.),(1.,0.756764909690213,1.),(1.,0.754186996432683,
1.),(1.,0.753329982306773,1.),(1.,0.75162086832093,1.),(1.,0.750768672063171,
1.),(1.,0.743147593559799,1.),(1.,0.736674219140203,1.),(1.,0.727518317868808,
1.),(1.,0.724558786513214,1.),(1.,0.718842636618393,1.),(1.,0.716086018731709,
1.),(1.,0.710794331727339,1.),(1.,0.708259263721099,1.),(1.,0.703429876147357,
1.),(1.,0.701135557954403,1.),(1.,0.698430453857348,1.),(1.,0.697897573909109,
1.),(1.,0.696848408664233,1.),(1.,0.696333170170124,1.),(1.,0.694818010360577,
1.),(1.,0.693847579638783,1.),(1.,0.691055128022452,1.),(1.,0.689351969841444,
1.),(1.,0.687806373745967,1.)))
REPRESENTATION_ITEM('')
SURFACE()
);
#185=(
BOUNDED_SURFACE()
B_SPLINE_SURFACE(3,2,((#59772,#59773,#59774),(#59775,#59776,#59777),(#59778,
#59779,#59780),(#59781,#59782,#59783),(#59784,#59785,#59786),(#59787,#59788,
#59789),(#59790,#59791,#59792),(#59793,#59794,#59795),(#59796,#59797,#59798),
(#59799,#59800,#59801),(#59802,#59803,#59804),(#59805,#59806,#59807),(#59808,
#59809,#59810),(#59811,#59812,#59813),(#59814,#59815,#59816),(#59817,#59818,
#59819),(#59820,#59821,#59822),(#59823,#59824,#59825),(#59826,#59827,#59828),
(#59829,#59830,#59831),(#59832,#59833,#59834),(#59835,#59836,#59837),(#59838,
#59839,#59840),(#59841,#59842,#59843),(#59844,#59845,#59846),(#59847,#59848,
#59849),(#59850,#59851,#59852),(#59853,#59854,#59855),(#59856,#59857,#59858),
(#59859,#59860,#59861),(#59862,#59863,#59864),(#59865,#59866,#59867),(#59868,
#59869,#59870),(#59871,#59872,#59873),(#59874,#59875,#59876),(#59877,#59878,
#59879),(#59880,#59881,#59882),(#59883,#59884,#59885),(#59886,#59887,#59888),
(#59889,#59890,#59891),(#59892,#59893,#59894),(#59895,#59896,#59897),(#59898,
#59899,#59900),(#59901,#59902,#59903),(#59904,#59905,#59906),(#59907,#59908,
#59909),(#59910,#59911,#59912),(#59913,#59914,#59915),(#59916,#59917,#59918),
(#59919,#59920,#59921),(#59922,#59923,#59924),(#59925,#59926,#59927),(#59928,
#59929,#59930),(#59931,#59932,#59933),(#59934,#59935,#59936),(#59937,#59938,
#59939),(#59940,#59941,#59942),(#59943,#59944,#59945),(#59946,#59947,#59948),
(#59949,#59950,#59951),(#59952,#59953,#59954),(#59955,#59956,#59957),(#59958,
#59959,#59960),(#59961,#59962,#59963),(#59964,#59965,#59966),(#59967,#59968,
#59969),(#59970,#59971,#59972),(#59973,#59974,#59975),(#59976,#59977,#59978),
(#59979,#59980,#59981),(#59982,#59983,#59984),(#59985,#59986,#59987),(#59988,
#59989,#59990),(#59991,#59992,#59993),(#59994,#59995,#59996),(#59997,#59998,
#59999),(#60000,#60001,#60002),(#60003,#60004,#60005),(#60006,#60007,#60008),
(#60009,#60010,#60011),(#60012,#60013,#60014),(#60015,#60016,#60017),(#60018,
#60019,#60020),(#60021,#60022,#60023),(#60024,#60025,#60026),(#60027,#60028,
#60029),(#60030,#60031,#60032),(#60033,#60034,#60035),(#60036,#60037,#60038),
(#60039,#60040,#60041),(#60042,#60043,#60044),(#60045,#60046,#60047),(#60048,
#60049,#60050),(#60051,#60052,#60053),(#60054,#60055,#60056),(#60057,#60058,
#60059),(#60060,#60061,#60062),(#60063,#60064,#60065),(#60066,#60067,#60068),
(#60069,#60070,#60071),(#60072,#60073,#60074),(#60075,#60076,#60077),(#60078,
#60079,#60080),(#60081,#60082,#60083),(#60084,#60085,#60086),(#60087,#60088,
#60089),(#60090,#60091,#60092),(#60093,#60094,#60095),(#60096,#60097,#60098),
(#60099,#60100,#60101),(#60102,#60103,#60104),(#60105,#60106,#60107),(#60108,
#60109,#60110),(#60111,#60112,#60113),(#60114,#60115,#60116),(#60117,#60118,
#60119),(#60120,#60121,#60122),(#60123,#60124,#60125),(#60126,#60127,#60128),
(#60129,#60130,#60131),(#60132,#60133,#60134),(#60135,#60136,#60137),(#60138,
#60139,#60140),(#60141,#60142,#60143),(#60144,#60145,#60146),(#60147,#60148,
#60149),(#60150,#60151,#60152),(#60153,#60154,#60155),(#60156,#60157,#60158),
(#60159,#60160,#60161),(#60162,#60163,#60164),(#60165,#60166,#60167),(#60168,
#60169,#60170),(#60171,#60172,#60173),(#60174,#60175,#60176),(#60177,#60178,
#60179),(#60180,#60181,#60182),(#60183,#60184,#60185),(#60186,#60187,#60188),
(#60189,#60190,#60191),(#60192,#60193,#60194),(#60195,#60196,#60197),(#60198,
#60199,#60200),(#60201,#60202,#60203),(#60204,#60205,#60206),(#60207,#60208,
#60209),(#60210,#60211,#60212),(#60213,#60214,#60215),(#60216,#60217,#60218),
(#60219,#60220,#60221),(#60222,#60223,#60224),(#60225,#60226,#60227),(#60228,
#60229,#60230),(#60231,#60232,#60233),(#60234,#60235,#60236),(#60237,#60238,
#60239),(#60240,#60241,#60242),(#60243,#60244,#60245),(#60246,#60247,#60248),
(#60249,#60250,#60251),(#60252,#60253,#60254),(#60255,#60256,#60257),(#60258,
#60259,#60260),(#60261,#60262,#60263),(#60264,#60265,#60266),(#60267,#60268,
#60269),(#60270,#60271,#60272),(#60273,#60274,#60275),(#60276,#60277,#60278),
(#60279,#60280,#60281),(#60282,#60283,#60284),(#60285,#60286,#60287),(#60288,
#60289,#60290),(#60291,#60292,#60293),(#60294,#60295,#60296),(#60297,#60298,
#60299),(#60300,#60301,#60302),(#60303,#60304,#60305),(#60306,#60307,#60308),
(#60309,#60310,#60311),(#60312,#60313,#60314),(#60315,#60316,#60317),(#60318,
#60319,#60320),(#60321,#60322,#60323),(#60324,#60325,#60326),(#60327,#60328,
#60329),(#60330,#60331,#60332),(#60333,#60334,#60335),(#60336,#60337,#60338),
(#60339,#60340,#60341),(#60342,#60343,#60344),(#60345,#60346,#60347),(#60348,
#60349,#60350),(#60351,#60352,#60353),(#60354,#60355,#60356),(#60357,#60358,
#60359),(#60360,#60361,#60362),(#60363,#60364,#60365),(#60366,#60367,#60368),
(#60369,#60370,#60371),(#60372,#60373,#60374),(#60375,#60376,#60377),(#60378,
#60379,#60380),(#60381,#60382,#60383),(#60384,#60385,#60386),(#60387,#60388,
#60389),(#60390,#60391,#60392),(#60393,#60394,#60395),(#60396,#60397,#60398),
(#60399,#60400,#60401),(#60402,#60403,#60404),(#60405,#60406,#60407),(#60408,
#60409,#60410),(#60411,#60412,#60413),(#60414,#60415,#60416),(#60417,#60418,
#60419),(#60420,#60421,#60422),(#60423,#60424,#60425),(#60426,#60427,#60428),
(#60429,#60430,#60431),(#60432,#60433,#60434),(#60435,#60436,#60437),(#60438,
#60439,#60440),(#60441,#60442,#60443),(#60444,#60445,#60446),(#60447,#60448,
#60449),(#60450,#60451,#60452),(#60453,#60454,#60455),(#60456,#60457,#60458),
(#60459,#60460,#60461),(#60462,#60463,#60464),(#60465,#60466,#60467),(#60468,
#60469,#60470),(#60471,#60472,#60473),(#60474,#60475,#60476),(#60477,#60478,
#60479),(#60480,#60481,#60482),(#60483,#60484,#60485),(#60486,#60487,#60488),
(#60489,#60490,#60491),(#60492,#60493,#60494),(#60495,#60496,#60497),(#60498,
#60499,#60500),(#60501,#60502,#60503),(#60504,#60505,#60506),(#60507,#60508,
#60509),(#60510,#60511,#60512),(#60513,#60514,#60515),(#60516,#60517,#60518),
(#60519,#60520,#60521),(#60522,#60523,#60524),(#60525,#60526,#60527),(#60528,
#60529,#60530),(#60531,#60532,#60533),(#60534,#60535,#60536),(#60537,#60538,
#60539),(#60540,#60541,#60542),(#60543,#60544,#60545),(#60546,#60547,#60548),
(#60549,#60550,#60551),(#60552,#60553,#60554),(#60555,#60556,#60557)),
 .UNSPECIFIED.,.T.,.F.,.F.)
B_SPLINE_SURFACE_WITH_KNOTS((4,2,2,2,2,2,2,2,2,2,2,2,2,2,2,2,2,2,2,2,2,
2,2,2,2,2,2,2,2,2,2,2,2,2,2,2,2,2,2,2,2,2,2,2,2,2,2,2,2,2,2,2,2,2,2,2,2,
2,2,2,2,2,2,2,2,2,2,2,2,2,2,2,2,2,2,2,2,2,2,2,2,2,2,2,2,2,2,2,2,2,2,2,2,
2,2,2,2,2,2,2,2,2,2,2,2,2,2,2,2,2,2,2,2,2,2,2,2,2,2,2,2,2,2,2,2,2,2,2,2,
2,4),(3,3),(0.,5.58974039156775E-5,0.000111794807831355,0.00022358961566271,
0.00044717923132542,0.000894358462650841,0.00178871692530168,0.00268307538795252,
0.00279487019578388,0.00290666500361523,0.00313025461927794,0.00357743385060336,
0.0044717923132542,0.00536615077590504,0.0054779455837364,0.00558974039156775,
0.00581333000723046,0.00626050923855589,0.00715486770120673,0.00804922616385757,
0.00827281577952028,0.00838461058735163,0.00849640539518299,0.00894358462650841,
0.00983794308915925,0.0107323015518101,0.0111794807831355,0.0114030703987982,
0.0115148652066296,0.0116266600144609,0.0125210184771118,0.0134153769397626,
0.013862556171088,0.0143097354024135,0.0145333250180762,0.0146451198259075,
0.0147569146337389,0.0152040938650643,0.0160984523277151,0.016992810790366,
0.0172164004060287,0.01732819521386,0.0174399900216914,0.0178871692530168,
0.0187815277156677,0.0196758861783185,0.0198994757939812,0.0201230654096439,
0.0205702446409693,0.0214646031036202,0.022358961566271,0.0228061407975964,
0.0230297304132591,0.0232533200289219,0.0241476784915727,0.0250420369542235,
0.0259363954168744,0.0261599850325371,0.0262717798403685,0.0263835746481998,
0.0268307538795252,0.0277251123421761,0.0286194708048269,0.0290666500361523,
0.029290239651815,0.0294020344596464,0.0295138292674777,0.0299610084988032,
0.0301845981144659,0.0302963929222972,0.0304081877301286,0.0313025461927794,
0.0321969046554303,0.0330912631180811,0.0332030579259125,0.0333148527337438,
0.0335384423494065,0.0339856215807319,0.0348799800433828,0.0357743385060336,
0.0359979281216963,0.0361097229295277,0.036221517737359,0.0366686969686845,
0.0375630554313353,0.0384574138939862,0.0389045931253116,0.0391281827409743,
0.0392399775488056,0.039351772356637,0.0402461308192878,0.0411404892819387,
0.0420348477445895,0.0424820269759149,0.0425938217837463,0.0427056165915777,
0.0429292062072404,0.0433763854385658,0.0438235646698912,0.044717923132542,
0.0451651023638675,0.0452768971716988,0.0453886919795302,0.0456122815951929,
0.0465066400578437,0.0474009985204946,0.04784817775182,0.0479599725596513,
0.0480717673674827,0.0482953569831454,0.0491897154457962,0.0500840739084471,
0.0505312531397725,0.0507548427554352,0.0508666375632666,0.0509784323710979,
0.0518727908337488,0.0527671492963996,0.0536615077590504,0.0538850973747132,
0.0539968921825445,0.0541086869903759,0.0545558662217013,0.0554502246843521,
0.056344583147003,0.0567917623783284,0.0570153519939911,0.0571271468018225,
0.0571830442057381,0.057210992907696,0.0572389416096538),(0.,1.),
 .UNSPECIFIED.)
GEOMETRIC_REPRESENTATION_ITEM()
RATIONAL_B_SPLINE_SURFACE(((1.,0.869037098890924,1.),(1.,0.869090662160833,
1.),(1.,0.869142132128297,1.),(1.,0.869241273997536,1.),(1.,0.869288882663707,
1.),(1.,0.869425835273797,1.),(1.,0.869509305917427,1.),(1.,0.869736328335375,
1.),(1.,0.869856492063896,1.),(1.,0.870124205131434,1.),(1.,0.870178998389397,
1.),(1.,0.869977707911342,1.),(1.,0.869356264735848,1.),(1.,0.867159523791841,
1.),(1.,0.865584183970151,1.),(1.,0.863281618119441,1.),(1.,0.86301835474559,
1.),(1.,0.862477312320675,1.),(1.,0.862200065545979,1.),(1.,0.861348450829986,
1.),(1.,0.860754210958995,1.),(1.,0.858894323573958,1.),(1.,0.857551540639133,
1.),(1.,0.853231873120265,1.),(1.,0.849963976579328,1.),(1.,0.8427337476379,
1.),(1.,0.838771159914112,1.),(1.,0.833964492549446,1.),(1.,0.83342564158097,
1.),(1.,0.832341102831786,1.),(1.,0.831795088875303,1.),(1.,0.83014615568217,
1.),(1.,0.829032346207458,1.),(1.,0.825650047625046,1.),(1.,0.823340697393356,
1.),(1.,0.816270214875414,1.),(1.,0.811366531889991,1.),(1.,0.801290493401484,
1.),(1.,0.796117786007922,1.),(1.,0.789558114002489,1.),(1.,0.788241524410975,
1.),(1.,0.786261176106014,1.),(1.,0.785600666410631,1.),(1.,0.784281253478811,
1.),(1.,0.783622032027989,1.),(1.,0.780329023537139,1.),(1.,0.777704514650253,
1.),(1.,0.76988692542286,1.),(1.,0.764749330047637,1.),(1.,0.75477051537079,
1.),(1.,0.749929030998746,1.),(1.,0.743012971461713,1.),(1.,0.740765474239869,
1.),(1.,0.73749827976927,1.),(1.,0.736426570328376,1.),(1.,0.734847329496033,
1.),(1.,0.734325595116705,1.),(1.,0.733292134556225,1.),(1.,0.732781563072735,
1.),(1.,0.728242967029025,1.),(1.,0.724610876621003,1.),(1.,0.718276943716503,
1.),(1.,0.715575135642169,1.),(1.,0.712312229125148,1.),(1.,0.711356200483893,
1.),(1.,0.709722323386846,1.),(1.,0.709044475655852,1.),(1.,0.708247344579823,
1.),(1.,0.708018238565296,1.),(1.,0.707730840005604,1.),(1.,0.707644376240716,
1.),(1.,0.707490608795043,1.),(1.,0.707423402545753,1.),(1.,0.707135559015692,
1.),(1.,0.707059523314824,1.),(1.,0.707285549205988,1.),(1.,0.708042221657254,
1.),(1.,0.710710092253751,1.),(1.,0.712621237041365,1.),(1.,0.715686665981657,
1.),(1.,0.716333543550958,1.),(1.,0.717353607349392,1.),(1.,0.717701919486094,
1.),(1.,0.718414964313171,1.),(1.,0.718779962361759,1.),(1.,0.720642167884513,
1.),(1.,0.722248110686464,1.),(1.,0.727379897082438,1.),(1.,0.731219242886661,
1.),(1.,0.739562059134817,1.),(1.,0.744065650037015,1.),(1.,0.750011006364496,
1.),(1.,0.751215898212902,1.),(1.,0.753654939425893,1.),(1.,0.754889413958793,
1.),(1.,0.758631191877784,1.),(1.,0.761160349547001,1.),(1.,0.768820010203822,
1.),(1.,0.774022074432147,1.),(1.,0.784467204631247,1.),(1.,0.789710609506525,
1.),(1.,0.797506397811445,1.),(1.,0.800093535602747,1.),(1.,0.803945021596591,
1.),(1.,0.805223982229172,1.),(1.,0.807770172561434,1.),(1.,0.80903292134295,
1.),(1.,0.815288089794111,1.),(1.,0.820107499923359,1.),(1.,0.829279685729609,
1.),(1.,0.833632779776828,1.),(1.,0.841777168809211,1.),(1.,0.845568802174027,
1.),(1.,0.849892563199079,1.),(1.,0.850736491533872,1.),(1.,0.851969804909359,
1.),(1.,0.852375793676684,1.),(1.,0.853174988795519,1.),(1.,0.853568068159912,
1.),(1.,0.855500704900974,1.),(1.,0.856941996550435,1.),(1.,0.860944601199298,
1.),(1.,0.863184927882986,1.),(1.,0.866767461005655,1.),(1.,0.868109793594765,
1.),(1.,0.869410481594525,1.),(1.,0.869725148569242,1.),(1.,0.870012890040282,
1.),(1.,0.870078086396283,1.),(1.,0.870128990964309,1.),(1.,0.870138141570321,
1.),(1.,0.870140676091054,1.),(1.,0.870134072965078,1.),(1.,0.870061808448095,
1.),(1.,0.869878426760649,1.),(1.,0.869416656440071,1.),(1.,0.869231611413219,
1.),(1.,0.868907522254946,1.),(1.,0.868791738615037,1.),(1.,0.868544686539316,
1.),(1.,0.868413337134317,1.),(1.,0.867163505604549,1.),(1.,0.865575442228637,
1.),(1.,0.861527724393334,1.),(1.,0.859067845844723,1.),(1.,0.853343564886148,
1.),(1.,0.850078971827717,1.),(1.,0.84598647975218,1.),(1.,0.845525923915504,
1.),(1.,0.844593252383724,1.),(1.,0.84412081177775,1.),(1.,0.842688930644052,
1.),(1.,0.841715504172781,1.),(1.,0.83874140215334,1.),(1.,0.836686926299113,
1.),(1.,0.830328826430023,1.),(1.,0.825830615536545,1.),(1.,0.816419106847222,
1.),(1.,0.81150547118942,1.),(1.,0.805169234170547,1.),(1.,0.803892294076685,
1.),(1.,0.801963643202623,1.),(1.,0.801318553163188,1.),(1.,0.800024181787751,
1.),(1.,0.799374551464301,1.),(1.,0.796123838581708,1.),(1.,0.793511112507122,
1.),(1.,0.785661232785625,1.),(1.,0.780412024366977,1.),(1.,0.770019050951368,
1.),(1.,0.76487497595969,1.),(1.,0.757351702086758,1.),(1.,0.754876228736365,
1.),(1.,0.751227350622943,1.),(1.,0.750021792912108,1.),(1.,0.748231675946372,
1.),(1.,0.747638007827609,1.),(1.,0.746457111568753,1.),(1.,0.745869506104255,
1.),(1.,0.740620037686994,1.),(1.,0.736256100649653,1.),(1.,0.728276221758877,
1.),(1.,0.724660242842317,1.),(1.,0.718324000111086,1.),(1.,0.715603718055959,
1.),(1.,0.712309706535428,1.),(1.,0.711342812014489,1.),(1.,0.710310353740139,
1.),(1.,0.710112755568336,1.),(1.,0.709736703375217,1.),(1.,0.709558069154282,
1.),(1.,0.709050371012769,1.),(1.,0.708749513760786,1.),(1.,0.70795992094024,
1.),(1.,0.707584199551303,1.),(1.,0.707134092959367,1.),(1.,0.70705970821773,
1.),(1.,0.707286843642986,1.),(1.,0.70803921126881,1.),(1.,0.710052147725902,
1.),(1.,0.710870383211632,1.),(1.,0.71207445357331,1.),(1.,0.712324328892365,
1.),(1.,0.712842122035176,1.),(1.,0.713110243316174,1.),(1.,0.713939993830723,
1.),(1.,0.714526359388936,1.),(1.,0.717617638747993,1.),(1.,0.720600584023788,
1.),(1.,0.727424242013839,1.),(1.,0.731264995819141,1.),(1.,0.737553652730096,
1.),(1.,0.739737848764794,1.),(1.,0.742566372039795,1.),(1.,0.74313699147918,
1.),(1.,0.744287770846871,1.),(1.,0.744868257643384,1.),(1.,0.746621209706891,
1.),(1.,0.747803690023989,1.),(1.,0.753778025133493,1.),(1.,0.758754654573864,
1.),(1.,0.768933369155768,1.),(1.,0.774135775395061,1.),(1.,0.781997810487323,
1.),(1.,0.784628358204622,1.),(1.,0.788575987637978,1.),(1.,0.789892170142193,
1.),(1.,0.791865311260895,1.),(1.,0.792522836387841,1.),(1.,0.793837245909085,
1.),(1.,0.794493861510745,1.),(1.,0.800385048001281,1.),(1.,0.80551453306944,
1.),(1.,0.815446188856963,1.),(1.,0.820248709446964,1.),(1.,0.829421742411055,
1.),(1.,0.833792601959078,1.),(1.,0.838919085477355,1.),(1.,0.839927506491091,
1.),(1.,0.841413476855047,1.),(1.,0.841904356336916,1.),(1.,0.842876996646255,
1.),(1.,0.843358860518912,1.),(1.,0.845737639832195,1.),(1.,0.847548776311049,
1.),(1.,0.852696372188048,1.),(1.,0.855747262756165,1.),(1.,0.861029201702321,
1.),(1.,0.863260436478246,1.),(1.,0.865941546711405,1.),(1.,0.86672419811369,
1.),(1.,0.867724144067475,1.),(1.,0.868028445735918,1.),(1.,0.868440362182281,
1.),(1.,0.868570244374482,1.),(1.,0.868753799883508,1.),(1.,0.868813107052922,
1.),(1.,0.868899233803952,1.),(1.,0.868927470387005,1.),(1.,0.868982996012711,
1.),(1.,0.86901031725597,1.),(1.,0.869037098890924,1.)))
REPRESENTATION_ITEM('')
SURFACE()
);
#186=(
BOUNDED_SURFACE()
B_SPLINE_SURFACE(3,2,((#60558,#60559,#60560),(#60561,#60562,#60563),(#60564,
#60565,#60566),(#60567,#60568,#60569),(#60570,#60571,#60572),(#60573,#60574,
#60575),(#60576,#60577,#60578),(#60579,#60580,#60581),(#60582,#60583,#60584),
(#60585,#60586,#60587),(#60588,#60589,#60590),(#60591,#60592,#60593),(#60594,
#60595,#60596),(#60597,#60598,#60599),(#60600,#60601,#60602),(#60603,#60604,
#60605),(#60606,#60607,#60608),(#60609,#60610,#60611),(#60612,#60613,#60614),
(#60615,#60616,#60617),(#60618,#60619,#60620),(#60621,#60622,#60623),(#60624,
#60625,#60626),(#60627,#60628,#60629),(#60630,#60631,#60632),(#60633,#60634,
#60635),(#60636,#60637,#60638),(#60639,#60640,#60641),(#60642,#60643,#60644),
(#60645,#60646,#60647),(#60648,#60649,#60650),(#60651,#60652,#60653),(#60654,
#60655,#60656),(#60657,#60658,#60659),(#60660,#60661,#60662),(#60663,#60664,
#60665),(#60666,#60667,#60668),(#60669,#60670,#60671),(#60672,#60673,#60674),
(#60675,#60676,#60677),(#60678,#60679,#60680),(#60681,#60682,#60683),(#60684,
#60685,#60686),(#60687,#60688,#60689),(#60690,#60691,#60692),(#60693,#60694,
#60695),(#60696,#60697,#60698),(#60699,#60700,#60701),(#60702,#60703,#60704),
(#60705,#60706,#60707)),.UNSPECIFIED.,.F.,.F.,.F.)
B_SPLINE_SURFACE_WITH_KNOTS((4,2,2,2,2,2,2,2,2,2,2,2,2,2,2,2,2,2,2,2,2,
2,2,2,4),(3,3),(-1.43114686768087E-17,0.000151016387548822,0.000302032775097659,
0.000453049162646496,0.000490803259533705,0.000528557356420914,0.000604065550195332,
0.000755081937744169,0.000906098325293005,0.000943852422180215,0.000981606519067424,
0.00105711471284184,0.00120813110039068,0.00135914748793952,0.00143465568171393,
0.00147240977860114,0.00151016387548835,0.00166118026303719,0.00181219665058603,
0.00196321303813486,0.00200096713502207,0.00203872123190928,0.0021142294256837,
0.00226524581323253,0.00241626220078137),(0.,1.),.UNSPECIFIED.)
GEOMETRIC_REPRESENTATION_ITEM()
RATIONAL_B_SPLINE_SURFACE(((1.,0.597614304667196,1.),(1.,0.597614548659316,
1.),(1.,0.597759141644792,1.),(1.,0.598330594325125,1.),(1.,0.598757253597273,
1.),(1.,0.599899281590871,1.),(1.,0.600614622994012,1.),(1.,0.601702544890616,
1.),(1.,0.601930044560374,1.),(1.,0.602404142171764,1.),(1.,0.602650079607565,
1.),(1.,0.603414616291635,1.),(1.,0.603959917797353,1.),(1.,0.605703947627896,
1.),(1.,0.607010476636725,1.),(1.,0.609926264739714,1.),(1.,0.611535514537476,
1.),(1.,0.613752265337911,1.),(1.,0.614205901208812,1.),(1.,0.615134253798264,
1.),(1.,0.61560958725321,1.),(1.,0.617063403759804,1.),(1.,0.618067502552084,
1.),(1.,0.621185868361561,1.),(1.,0.623406027602217,1.),(1.,0.628140854568891,
1.),(1.,0.63065552053793,1.),(1.,0.634661693683576,1.),(1.,0.636036157866121,
1.),(1.,0.638158552325295,1.),(1.,0.638876846031255,1.),(1.,0.640330763885221,
1.),(1.,0.641065138363023,1.),(1.,0.644774107930351,1.),(1.,0.647859895490701,
1.),(1.,0.654270816871591,1.),(1.,0.65759594902533,1.),(1.,0.664490189617747,
1.),(1.,0.668059281341528,1.),(1.,0.672677743668185,1.),(1.,0.673609777828573,
1.),(1.,0.675481455951091,1.),(1.,0.676422055868733,1.),(1.,0.679258012829202,
1.),(1.,0.681167525351118,1.),(1.,0.686951752951439,1.),(1.,0.690882126194853,
1.),(1.,0.698887084712717,1.),(1.,0.702961683112489,1.),(1.,0.707106781186548,
1.)))
REPRESENTATION_ITEM('')
SURFACE()
);
#187=(
BOUNDED_SURFACE()
B_SPLINE_SURFACE(3,2,((#60738,#60739,#60740),(#60741,#60742,#60743),(#60744,
#60745,#60746),(#60747,#60748,#60749),(#60750,#60751,#60752),(#60753,#60754,
#60755),(#60756,#60757,#60758),(#60759,#60760,#60761),(#60762,#60763,#60764),
(#60765,#60766,#60767),(#60768,#60769,#60770),(#60771,#60772,#60773),(#60774,
#60775,#60776),(#60777,#60778,#60779),(#60780,#60781,#60782),(#60783,#60784,
#60785),(#60786,#60787,#60788),(#60789,#60790,#60791),(#60792,#60793,#60794),
(#60795,#60796,#60797),(#60798,#60799,#60800),(#60801,#60802,#60803),(#60804,
#60805,#60806),(#60807,#60808,#60809),(#60810,#60811,#60812),(#60813,#60814,
#60815),(#60816,#60817,#60818),(#60819,#60820,#60821),(#60822,#60823,#60824),
(#60825,#60826,#60827),(#60828,#60829,#60830),(#60831,#60832,#60833),(#60834,
#60835,#60836),(#60837,#60838,#60839),(#60840,#60841,#60842),(#60843,#60844,
#60845),(#60846,#60847,#60848),(#60849,#60850,#60851),(#60852,#60853,#60854),
(#60855,#60856,#60857),(#60858,#60859,#60860),(#60861,#60862,#60863),(#60864,
#60865,#60866),(#60867,#60868,#60869),(#60870,#60871,#60872),(#60873,#60874,
#60875),(#60876,#60877,#60878),(#60879,#60880,#60881),(#60882,#60883,#60884),
(#60885,#60886,#60887),(#60888,#60889,#60890),(#60891,#60892,#60893),(#60894,
#60895,#60896),(#60897,#60898,#60899),(#60900,#60901,#60902),(#60903,#60904,
#60905),(#60906,#60907,#60908),(#60909,#60910,#60911),(#60912,#60913,#60914),
(#60915,#60916,#60917),(#60918,#60919,#60920),(#60921,#60922,#60923),(#60924,
#60925,#60926),(#60927,#60928,#60929),(#60930,#60931,#60932),(#60933,#60934,
#60935),(#60936,#60937,#60938),(#60939,#60940,#60941),(#60942,#60943,#60944),
(#60945,#60946,#60947),(#60948,#60949,#60950),(#60951,#60952,#60953),(#60954,
#60955,#60956),(#60957,#60958,#60959),(#60960,#60961,#60962),(#60963,#60964,
#60965),(#60966,#60967,#60968),(#60969,#60970,#60971),(#60972,#60973,#60974),
(#60975,#60976,#60977),(#60978,#60979,#60980),(#60981,#60982,#60983),(#60984,
#60985,#60986),(#60987,#60988,#60989),(#60990,#60991,#60992),(#60993,#60994,
#60995),(#60996,#60997,#60998),(#60999,#61000,#61001),(#61002,#61003,#61004),
(#61005,#61006,#61007),(#61008,#61009,#61010),(#61011,#61012,#61013),(#61014,
#61015,#61016),(#61017,#61018,#61019),(#61020,#61021,#61022),(#61023,#61024,
#61025),(#61026,#61027,#61028),(#61029,#61030,#61031),(#61032,#61033,#61034),
(#61035,#61036,#61037),(#61038,#61039,#61040),(#61041,#61042,#61043),(#61044,
#61045,#61046),(#61047,#61048,#61049),(#61050,#61051,#61052),(#61053,#61054,
#61055),(#61056,#61057,#61058),(#61059,#61060,#61061),(#61062,#61063,#61064),
(#61065,#61066,#61067),(#61068,#61069,#61070),(#61071,#61072,#61073),(#61074,
#61075,#61076),(#61077,#61078,#61079),(#61080,#61081,#61082),(#61083,#61084,
#61085),(#61086,#61087,#61088),(#61089,#61090,#61091),(#61092,#61093,#61094),
(#61095,#61096,#61097),(#61098,#61099,#61100),(#61101,#61102,#61103),(#61104,
#61105,#61106),(#61107,#61108,#61109),(#61110,#61111,#61112),(#61113,#61114,
#61115),(#61116,#61117,#61118),(#61119,#61120,#61121),(#61122,#61123,#61124),
(#61125,#61126,#61127),(#61128,#61129,#61130),(#61131,#61132,#61133),(#61134,
#61135,#61136),(#61137,#61138,#61139),(#61140,#61141,#61142),(#61143,#61144,
#61145),(#61146,#61147,#61148),(#61149,#61150,#61151),(#61152,#61153,#61154),
(#61155,#61156,#61157),(#61158,#61159,#61160),(#61161,#61162,#61163),(#61164,
#61165,#61166),(#61167,#61168,#61169),(#61170,#61171,#61172),(#61173,#61174,
#61175),(#61176,#61177,#61178),(#61179,#61180,#61181),(#61182,#61183,#61184),
(#61185,#61186,#61187),(#61188,#61189,#61190),(#61191,#61192,#61193),(#61194,
#61195,#61196),(#61197,#61198,#61199),(#61200,#61201,#61202),(#61203,#61204,
#61205),(#61206,#61207,#61208),(#61209,#61210,#61211),(#61212,#61213,#61214),
(#61215,#61216,#61217),(#61218,#61219,#61220),(#61221,#61222,#61223),(#61224,
#61225,#61226),(#61227,#61228,#61229),(#61230,#61231,#61232),(#61233,#61234,
#61235),(#61236,#61237,#61238),(#61239,#61240,#61241),(#61242,#61243,#61244),
(#61245,#61246,#61247),(#61248,#61249,#61250),(#61251,#61252,#61253),(#61254,
#61255,#61256),(#61257,#61258,#61259),(#61260,#61261,#61262),(#61263,#61264,
#61265),(#61266,#61267,#61268),(#61269,#61270,#61271),(#61272,#61273,#61274),
(#61275,#61276,#61277),(#61278,#61279,#61280),(#61281,#61282,#61283),(#61284,
#61285,#61286),(#61287,#61288,#61289),(#61290,#61291,#61292),(#61293,#61294,
#61295),(#61296,#61297,#61298),(#61299,#61300,#61301),(#61302,#61303,#61304),
(#61305,#61306,#61307),(#61308,#61309,#61310),(#61311,#61312,#61313),(#61314,
#61315,#61316),(#61317,#61318,#61319),(#61320,#61321,#61322),(#61323,#61324,
#61325),(#61326,#61327,#61328),(#61329,#61330,#61331),(#61332,#61333,#61334),
(#61335,#61336,#61337),(#61338,#61339,#61340),(#61341,#61342,#61343),(#61344,
#61345,#61346),(#61347,#61348,#61349),(#61350,#61351,#61352),(#61353,#61354,
#61355),(#61356,#61357,#61358),(#61359,#61360,#61361),(#61362,#61363,#61364),
(#61365,#61366,#61367),(#61368,#61369,#61370),(#61371,#61372,#61373),(#61374,
#61375,#61376),(#61377,#61378,#61379),(#61380,#61381,#61382),(#61383,#61384,
#61385),(#61386,#61387,#61388),(#61389,#61390,#61391),(#61392,#61393,#61394),
(#61395,#61396,#61397),(#61398,#61399,#61400),(#61401,#61402,#61403),(#61404,
#61405,#61406),(#61407,#61408,#61409),(#61410,#61411,#61412),(#61413,#61414,
#61415),(#61416,#61417,#61418),(#61419,#61420,#61421),(#61422,#61423,#61424),
(#61425,#61426,#61427),(#61428,#61429,#61430),(#61431,#61432,#61433),(#61434,
#61435,#61436),(#61437,#61438,#61439),(#61440,#61441,#61442),(#61443,#61444,
#61445),(#61446,#61447,#61448),(#61449,#61450,#61451),(#61452,#61453,#61454),
(#61455,#61456,#61457),(#61458,#61459,#61460),(#61461,#61462,#61463),(#61464,
#61465,#61466),(#61467,#61468,#61469),(#61470,#61471,#61472),(#61473,#61474,
#61475),(#61476,#61477,#61478),(#61479,#61480,#61481),(#61482,#61483,#61484),
(#61485,#61486,#61487),(#61488,#61489,#61490),(#61491,#61492,#61493),(#61494,
#61495,#61496),(#61497,#61498,#61499),(#61500,#61501,#61502),(#61503,#61504,
#61505),(#61506,#61507,#61508),(#61509,#61510,#61511),(#61512,#61513,#61514),
(#61515,#61516,#61517),(#61518,#61519,#61520),(#61521,#61522,#61523),(#61524,
#61525,#61526),(#61527,#61528,#61529)),.UNSPECIFIED.,.F.,.F.,.F.)
B_SPLINE_SURFACE_WITH_KNOTS((4,2,2,2,2,2,2,2,2,2,2,2,2,2,2,2,2,2,2,2,2,
2,2,2,2,2,2,2,2,2,2,2,2,2,2,2,2,2,2,2,2,2,2,2,2,2,2,2,2,2,2,2,2,2,2,2,2,
2,2,2,2,2,2,2,2,2,2,2,2,2,2,2,2,2,2,2,2,2,2,2,2,2,2,2,2,2,2,2,2,2,2,2,2,
2,2,2,2,2,2,2,2,2,2,2,2,2,2,2,2,2,2,2,2,2,2,2,2,2,2,2,2,2,2,2,2,2,2,2,2,
2,2,4),(3,3),(0.00550389531139888,0.00574810157344769,0.0058702047044721,
0.0059923078354965,0.00648072035959412,0.00745754540778936,0.0084343704559846,
0.00892278298008221,0.00916698924213102,0.00928909237315543,0.00941119550417983,
0.0103880205523751,0.0113648456005703,0.0118532581246679,0.0123416706487656,
0.0125858769108144,0.0127079800418388,0.0128300831728632,0.0133184956969608,
0.014295320745156,0.0152721457933513,0.0155163520554001,0.0156384551864245,
0.0157605583174489,0.0162489708415465,0.0172257958897417,0.018202620937937,
0.0184468271999858,0.0185689303310102,0.0186910334620346,0.0191794459861322,
0.0201562710343275,0.0211330960825227,0.0213773023445715,0.0214994054755959,
0.0216215086066203,0.0221099211307179,0.0230867461789132,0.0240635712271084,
0.024551983751206,0.0246740868822304,0.0247961900132548,0.0250403962753037,
0.0260172213234989,0.0269940463716941,0.0279708714198894,0.0282150776819382,
0.0283371808129626,0.028459283943987,0.0289476964680846,0.0299245215162798,
0.0309013465644751,0.0313897590885727,0.0316339653506215,0.0317560684816459,
0.0318781716126703,0.0323665841367679,0.0328549966608656,0.0333434091849632,
0.0338318217090608,0.0343202342331584,0.0345644404952072,0.0346865436262316,
0.034808646757256,0.0352970592813537,0.0357854718054513,0.0367622968536465,
0.0377391219018418,0.0379833281638906,0.038105431294915,0.0382275344259394,
0.038715946950037,0.0396927719982322,0.0406695970464275,0.0411580095705251,
0.0414022158325739,0.0415243189635983,0.0416464220946227,0.0426232471428179,
0.0436000721910132,0.0440884847151108,0.0445768972392084,0.045065309763306,
0.0453095160253549,0.0455537222874037,0.0465305473355989,0.0475073723837941,
0.047751578645843,0.0478736817768674,0.0479957849078918,0.0484841974319894,
0.0494610224801846,0.0504378475283799,0.0506820537904287,0.0508041569214531,
0.0509262600524775,0.0514146725765751,0.0523914976247703,0.0533683226729656,
0.0536125289350144,0.0537346320660388,0.0538567351970632,0.0543451477211608,
0.055321972769356,0.0562987978175513,0.0567872103416489,0.0569093134726733,
0.0570314166036977,0.0572756228657465,0.0582524479139418,0.059229272962137,
0.0602060980103322,0.0604503042723811,0.0605724074034055,0.0606945105344299,
0.0611829230585275,0.0621597481067227,0.063136573154918,0.0636249856790156,
0.0638691919410644,0.0639302435065766,0.0639912950720888,0.0641133982031132,
0.0646018107272108,0.0650902232513084,0.0655786357754061,0.0660670482995037,
0.0665554608236013,0.0667996670856501,0.0669217702166745,0.0670438733476989,
0.0680206983958942),(-4.72906511448186E-7,1.),.UNSPECIFIED.)
GEOMETRIC_REPRESENTATION_ITEM()
RATIONAL_B_SPLINE_SURFACE(((1.00000023498091,0.751556694153118,1.),(1.00000023378176,
0.752824548397775,1.),(1.00000023256666,0.754109265472953,1.),(1.00000023072186,
0.756059754072068,1.),(1.00000023010324,0.756713819297174,1.),(1.0000002288589,
0.758029444458224,1.),(1.000000228233,0.75869120103434,1.),(1.00000022508853,
0.76201582674644,1.),(1.00000022253726,0.76471326317563,1.),(1.00000021480751,
0.77288585853503,1.),(1.00000020955378,0.778440589326931,1.),(1.00000019899112,
0.789608400404832,1.),(1.00000019368186,0.795221829049161,1.),(1.00000018577219,
0.803584653975839,1.),(1.00000018314456,0.806362824271203,1.),(1.00000017922784,
0.810503941986009,1.),(1.00000017792638,0.811879961599245,1.),(1.00000017598177,
0.813935983448259,1.),(1.0000001753352,0.814619594228044,1.),(1.00000017404777,
0.815980786342396,1.),(1.00000017340658,0.816658712809378,1.),(1.00000016765943,
0.822735126197709,1.),(1.0000001627188,0.827958812159829,1.),(1.00000015326503,
0.837954194734113,1.),(1.00000014875159,0.842726222382481,1.),(1.00000014236885,
0.849474639737199,1.),(1.00000014030585,0.851655826992419,1.),(1.00000013632082,
0.855869168446521,1.),(1.00000013439877,0.857901334912284,1.),(1.00000013163084,
0.860827846311646,1.),(1.00000013072739,0.861783052685079,1.),(1.00000012940227,
0.863184085582916,1.),(1.00000012896558,0.863645799803543,1.),(1.00000012810242,
0.864558404613122,1.),(1.00000012767567,0.865009605497141,1.),(1.00000012557194,
0.867233865854088,1.),(1.00000012398733,0.868909259809825,1.),(1.00000011953754,
0.873613984612272,1.),(1.00000011697604,0.876322231319804,1.),(1.00000011271749,
0.880824759327638,1.),(1.00000011102027,0.882619221541114,1.),(1.00000010948111,
0.884246560006968,1.),(1.00000010920244,0.884541198563755,1.),(1.00000010882909,
0.884935937378963,1.),(1.00000010871208,0.885059646520894,1.),(1.00000010849312,
0.885291153381852,1.),(1.00000010839109,0.88539903398853,1.),(1.00000010792017,
0.885896934847654,1.),(1.00000010766867,0.886162837228243,1.),(1.00000010728335,
0.886570231636448,1.),(1.00000010751835,0.886321775490983,1.),(1.00000010894598,
0.884812349368159,1.),(1.00000011013867,0.883551331717548,1.),(1.00000011221839,
0.881352460936778,1.),(1.0000001126638,0.88088153148373,1.),(1.000000113376,
0.880128522727162,1.),(1.00000011362075,0.879869750411651,1.),(1.00000011412494,
0.879336683160622,1.),(1.00000011438458,0.879062164951402,1.),(1.00000011571638,
0.877654060682486,1.),(1.0000001168888,0.876414476784003,1.),(1.00000012070877,
0.872375657113504,1.),(1.00000012365859,0.869256837455263,1.),(1.0000001302817,
0.86225427633696,1.),(1.00000013395525,0.858370260865121,1.),(1.0000001389552,
0.853083860085661,1.),(1.00000013997561,0.852004991745369,1.),(1.00000014153605,
0.850355143413675,1.),(1.00000014206137,0.849799736088604,1.),(1.00000014311937,
0.848681114911057,1.),(1.00000014365233,0.848117621698517,1.),(1.00000014633638,
0.845279799797655,1.),(1.0000001485452,0.842944430835434,1.),(1.00000015533688,
0.835763650211785,1.),(1.00000016008491,0.830743595177666,1.),(1.0000001699216,
0.820343351831782,1.),(1.00000017501058,0.814962810757057,1.),(1.0000001828229,
0.806702912434936,1.),(1.00000018545676,0.803918154992135,1.),(1.00000018877756,
0.800407100997016,1.),(1.00000018944312,0.799703414672647,1.),(1.00000019077364,
0.798296664875502,1.),(1.00000019143901,0.797593180627382,1.),(1.00000019343504,
0.795482793926751,1.),(1.00000019476564,0.794075956555709,1.),(1.00000020141324,
0.78704750614951,1.),(1.00000020671441,0.781442625039865,1.),(1.00000021714846,
0.770410799011106,1.),(1.00000022228161,0.764983560872734,1.),(1.00000023222946,
0.754465779333137,1.),(1.00000023704448,0.749374905591535,1.),(1.00000024275479,
0.743337436815082,1.),(1.00000024388136,0.742146327927527,1.),(1.00000024554567,
0.740386673133335,1.),(1.00000024609518,0.739805676275109,1.),(1.00000024718247,
0.738656092994039,1.),(1.0000002477204,0.738087342446234,1.),(1.00000025038083,
0.735274497907314,1.),(1.00000025241562,0.73312312519276,1.),(1.00000025821379,
0.726992773429071,1.),(1.00000026167096,0.723337538949804,1.),(1.00000026763152,
0.717035483201795,1.),(1.00000027013488,0.714388705392069,1.),(1.00000027307154,
0.711283802444097,1.),(1.00000027391403,0.710393041672387,1.),(1.00000027496038,
0.70928675234185,1.),(1.00000027527292,0.708956297159223,1.),(1.0000002756858,
0.708519762422626,1.),(1.00000027581414,0.708384075000737,1.),(1.00000027605176,
0.708132837756234,1.),(1.0000002761608,0.708017549283914,1.),(1.00000027665727,
0.707492635552901,1.),(1.00000027689845,0.707237643899567,1.),(1.00000027707247,
0.707053652944908,1.),(1.00000027700532,0.707124653493474,1.),(1.00000027656751,
0.707587539289571,1.),(1.00000027619686,0.707979423441002,1.),(1.00000027515804,
0.709077765452766,1.),(1.00000027448986,0.709784221424154,1.),(1.00000027286305,
0.711504238909358,1.),(1.00000027190441,0.71251779792269,1.),(1.00000027025468,
0.714262047196191,1.),(1.00000026966948,0.714880773824933,1.),(1.00000026873957,
0.715863955555072,1.),(1.00000026842092,0.716200864287518,1.),(1.00000026776639,
0.716892893458133,1.),(1.00000026743032,0.717248218521567,1.),(1.00000026570947,
0.719067653552063,1.),(1.00000026420991,0.720653126054481,1.),(1.00000026098872,
0.724058862455822,1.),(1.00000025926709,0.725879130357689,1.),(1.00000025380292,
0.731656351861655,1.),(1.00000024976157,0.73592923685194,1.),(1.00000024105014,
0.745139754107446,1.),(1.00000023637996,0.750077498999356,1.),(1.00000023024597,
0.756562909310098,1.),(1.00000022900433,0.757875682834899,1.),(1.00000022712135,
0.759866544520447,1.),(1.00000022649027,0.760533782306009,1.),(1.00000022522155,
0.761875189848965,1.),(1.00000022458429,0.762548959437356,1.),(1.00000022139052,
0.765925697624077,1.),(1.00000021880595,0.768658341855167,1.),(1.00000021099365,
0.776918218582894,1.),(1.00000020570797,0.782506721948014,1.),(1.00000019512297,
0.793698161123683,1.),(1.0000001898233,0.799301448123694,1.),(1.00000018195664,
0.807618799497514,1.),(1.00000017934813,0.810376757675791,1.),(1.00000017546704,
0.81448020734433,1.),(1.00000017417861,0.815842445219629,1.),(1.00000017225527,
0.817875977839375,1.),(1.00000017161558,0.818552316235376,1.),(1.00000017034262,
0.819898209492926,1.),(1.00000016970896,0.82056816809445,1.),(1.00000016403231,
0.826570043806966,1.),(1.0000001591733,0.831707434235114,1.),(1.00000014991731,
0.841493708708982,1.),(1.00000014552003,0.846142917478774,1.),(1.00000013933591,
0.852681332968294,1.),(1.0000001373432,0.854788213702908,1.),(1.00000013350673,
0.858844481985634,1.),(1.00000013166296,0.860793881731502,1.),(1.00000012813688,
0.864521979247798,1.),(1.00000012645455,0.866300691342452,1.),(1.00000012406244,
0.868829842162124,1.),(1.00000012329029,0.869646238009235,1.),(1.00000012179807,
0.87122394532148,1.),(1.00000012107784,0.871985436590129,1.),(1.00000011760779,
0.875654291255009,1.),(1.00000011525083,0.87814628298712,1.),(1.00000011142444,
0.882191896881282,1.),(1.00000010995485,0.883745677395368,1.),(1.00000010871133,
0.885060444051895,1.),(1.00000010849234,0.885291984185686,1.),(1.00000010820926,
0.885591273045841,1.),(1.00000010812248,0.885683031852686,1.),(1.00000010796419,
0.885850383459224,1.),(1.00000010789265,0.885926031072474,1.),(1.00000010757428,
0.886262631448316,1.),(1.00000010744539,0.886398908559158,1.),(1.00000010742813,
0.886417163206912,1.),(1.0000001079088,0.885908946265843,1.),(1.00000010982151,
0.88388666077102,1.),(1.0000001112536,0.882372526971855,1.),(1.00000011362453,
0.879865758662412,1.),(1.00000011412778,0.879333674429881,1.),(1.00000011492607,
0.878489652629009,1.),(1.0000001151994,0.87820066249251,1.),(1.0000001157605,
0.877607413101931,1.),(1.00000011604836,0.877303065972634,1.),(1.00000011751912,
0.875748046563914,1.),(1.00000011879965,0.87439415067658,1.),(1.00000012293461,
0.870022288419149,1.),(1.00000012608197,0.866694610164977,1.),(1.00000013307372,
0.859302298416578,1.),(1.00000013691837,0.855237378460135,1.),(1.00000014211423,
0.849743845714332,1.),(1.00000014317292,0.848624503463328,1.),(1.0000001447894,
0.846915410070114,1.),(1.00000014533277,0.846340908054068,1.),(1.00000014642633,
0.845184698703843,1.),(1.0000001469768,0.844602685849943,1.),(1.00000014974713,
0.841673639940311,1.),(1.00000015202083,0.839269684772021,1.),(1.00000015899447,
0.831896507955678,1.),(1.00000016384702,0.826765951203782,1.),(1.00000017385695,
0.816182532882831,1.),(1.00000017901468,0.810729315211788,1.),(1.00000018690038,
0.80239183329862,1.),(1.00000018955373,0.799586467378934,1.),(1.00000019289228,
0.796056651380399,1.),(1.00000019356127,0.795349331223752,1.),(1.00000019489798,
0.793936034393844,1.),(1.00000019556608,0.793229659050175,1.),(1.00000019756922,
0.791111755587851,1.),(1.00000019890311,0.789701448963109,1.),(1.0000002055597,
0.782663492366119,1.),(1.00000021084436,0.777076066790433,1.),(1.00000022119435,
0.766133106017418,1.),(1.00000022625995,0.7607772915656,1.),(1.00000023601756,
0.750460654634383,1.),(1.00000024070987,0.745499520465223,1.),(1.00000024622976,
0.739663381402246,1.),(1.0000002473164,0.738514495390714,1.),(1.00000024891798,
0.736821157275602,1.),(1.00000024944697,0.736261859406495,1.),(1.00000025049176,
0.73515720721303,1.),(1.00000025100799,0.73461140273185,1.),(1.00000025355765,
0.731915666474236,1.),(1.00000025549664,0.729865595746991,1.),(1.00000026098678,
0.724060911408639,1.),(1.00000026421107,0.720651898486557,1.),(1.00000026965822,
0.714892677044352,1.),(1.00000027188102,0.712542530134079,1.),(1.00000027436892,
0.709912091354844,1.),(1.0000002750572,0.709184377859772,1.),(1.00000027586651,
0.708328704157888,1.),(1.0000002760991,0.708082793128139,1.),(1.00000027634216,
0.707825802489092,1.),(1.00000027638839,0.707776924211404,1.),(1.00000027647605,
0.707684238567988,1.),(1.00000027651752,0.707640402018307,1.),(1.00000027663423,
0.707517005252166,1.),(1.00000027670223,0.707445102385259,1.),(1.00000027699347,
0.707137182867287,1.),(1.00000027707025,0.707055995209309,1.),(1.00000027691727,
0.707217741884412,1.),(1.0000002766875,0.707460675529496,1.),(1.00000027592831,
0.708263359580143,1.),(1.0000002753989,0.708823108402302,1.),(1.00000027404836,
0.710251021221229,1.),(1.00000027322724,0.711119182945965,1.),(1.00000027130223,
0.713154483324201,1.),(1.00000027019833,0.71432161923774,1.),(1.00000026833779,
0.716288757540562,1.),(1.0000002676835,0.716980535502155,1.),(1.00000026665187,
0.718071263738537,1.),(1.00000026629963,0.71844368295856,1.),(1.00000026557859,
0.719206030037194,1.),(1.00000026520954,0.719596229989639,1.),(1.0000002618201,
0.723179856882723,1.),(1.000000258339,0.726860386021971,1.),(1.00000025448214,
0.730938217147024,1.)))
REPRESENTATION_ITEM('')
SURFACE()
);
#188=(
BOUNDED_SURFACE()
B_SPLINE_SURFACE(3,2,((#61530,#61531,#61532),(#61533,#61534,#61535),(#61536,
#61537,#61538),(#61539,#61540,#61541),(#61542,#61543,#61544),(#61545,#61546,
#61547),(#61548,#61549,#61550),(#61551,#61552,#61553),(#61554,#61555,#61556),
(#61557,#61558,#61559),(#61560,#61561,#61562),(#61563,#61564,#61565),(#61566,
#61567,#61568),(#61569,#61570,#61571),(#61572,#61573,#61574),(#61575,#61576,
#61577),(#61578,#61579,#61580),(#61581,#61582,#61583),(#61584,#61585,#61586),
(#61587,#61588,#61589),(#61590,#61591,#61592),(#61593,#61594,#61595),(#61596,
#61597,#61598),(#61599,#61600,#61601),(#61602,#61603,#61604),(#61605,#61606,
#61607),(#61608,#61609,#61610),(#61611,#61612,#61613),(#61614,#61615,#61616),
(#61617,#61618,#61619),(#61620,#61621,#61622),(#61623,#61624,#61625),(#61626,
#61627,#61628),(#61629,#61630,#61631),(#61632,#61633,#61634),(#61635,#61636,
#61637),(#61638,#61639,#61640),(#61641,#61642,#61643),(#61644,#61645,#61646),
(#61647,#61648,#61649),(#61650,#61651,#61652),(#61653,#61654,#61655),(#61656,
#61657,#61658),(#61659,#61660,#61661),(#61662,#61663,#61664),(#61665,#61666,
#61667),(#61668,#61669,#61670),(#61671,#61672,#61673),(#61674,#61675,#61676),
(#61677,#61678,#61679),(#61680,#61681,#61682),(#61683,#61684,#61685),(#61686,
#61687,#61688),(#61689,#61690,#61691),(#61692,#61693,#61694),(#61695,#61696,
#61697),(#61698,#61699,#61700),(#61701,#61702,#61703),(#61704,#61705,#61706),
(#61707,#61708,#61709),(#61710,#61711,#61712),(#61713,#61714,#61715),(#61716,
#61717,#61718),(#61719,#61720,#61721),(#61722,#61723,#61724),(#61725,#61726,
#61727),(#61728,#61729,#61730),(#61731,#61732,#61733),(#61734,#61735,#61736),
(#61737,#61738,#61739),(#61740,#61741,#61742),(#61743,#61744,#61745),(#61746,
#61747,#61748),(#61749,#61750,#61751),(#61752,#61753,#61754),(#61755,#61756,
#61757),(#61758,#61759,#61760),(#61761,#61762,#61763),(#61764,#61765,#61766),
(#61767,#61768,#61769),(#61770,#61771,#61772),(#61773,#61774,#61775),(#61776,
#61777,#61778),(#61779,#61780,#61781),(#61782,#61783,#61784),(#61785,#61786,
#61787),(#61788,#61789,#61790),(#61791,#61792,#61793),(#61794,#61795,#61796),
(#61797,#61798,#61799),(#61800,#61801,#61802),(#61803,#61804,#61805),(#61806,
#61807,#61808),(#61809,#61810,#61811),(#61812,#61813,#61814),(#61815,#61816,
#61817),(#61818,#61819,#61820),(#61821,#61822,#61823),(#61824,#61825,#61826),
(#61827,#61828,#61829),(#61830,#61831,#61832),(#61833,#61834,#61835),(#61836,
#61837,#61838),(#61839,#61840,#61841),(#61842,#61843,#61844),(#61845,#61846,
#61847),(#61848,#61849,#61850),(#61851,#61852,#61853),(#61854,#61855,#61856),
(#61857,#61858,#61859),(#61860,#61861,#61862),(#61863,#61864,#61865),(#61866,
#61867,#61868),(#61869,#61870,#61871),(#61872,#61873,#61874),(#61875,#61876,
#61877),(#61878,#61879,#61880),(#61881,#61882,#61883)),.UNSPECIFIED.,.F.,
 .F.,.F.)
B_SPLINE_SURFACE_WITH_KNOTS((4,2,2,2,2,2,2,2,2,2,2,2,2,2,2,2,2,2,2,2,2,
2,2,2,2,2,2,2,2,2,2,2,2,2,2,2,2,2,2,2,2,2,2,2,2,2,2,2,2,2,2,2,2,2,2,2,2,
2,4),(3,3),(0.00917852058677495,0.00979162970055923,0.0104047388143435,
0.0110178479281278,0.0113244024850199,0.011477679763466,0.0116309570419121,
0.0122440661556963,0.0128571752694806,0.0134702843832649,0.0136235616617109,
0.013700200300934,0.013776838940157,0.0140833934970491,0.0146965026108334,
0.0150030571677256,0.0153096117246177,0.0156161662815098,0.0157694435599559,
0.015922720838402,0.0162292753952941,0.0165358299521862,0.0168423845090784,
0.0171489390659705,0.0174554936228627,0.0175321322620857,0.0176087709013087,
0.0177620481797548,0.0180686027366469,0.0183751572935391,0.0189882664073233,
0.0191415436857694,0.0192181823249925,0.0192948209642155,0.0196013755211076,
0.0202144846348919,0.0208275937486762,0.0209808710271222,0.0211341483055683,
0.0214407028624604,0.0217472574193526,0.0218238960585756,0.0219005346977986,
0.0220538119762447,0.022666921090029,0.0232800302038133,0.0238931393175975,
0.0245062484313818,0.024812802988274,0.02496608026672,0.0251193575451661,
0.0257324666589504,0.0263455757727346,0.0269586848865189,0.0275717940003032,
0.0278783485571953,0.0280316258356414,0.0281849031140875,0.0287980122278717),
(0.,1.),.UNSPECIFIED.)
GEOMETRIC_REPRESENTATION_ITEM()
RATIONAL_B_SPLINE_SURFACE(((1.,0.695382524078308,1.),(1.,0.690973084826369,
1.),(1.,0.686397501074747,1.),(1.,0.676941961810577,1.),(1.,0.672061709768397,
1.),(1.,0.66203086632443,1.),(1.,0.656880116106326,1.),(1.,0.64898582257856,
1.),(1.,0.646326468817071,1.),(1.,0.642301097907339,1.),(1.,0.640953260446955,
1.),(1.,0.638246544124457,1.),(1.,0.636892439350123,1.),(1.,0.630130032747308,
1.),(1.,0.624736470834729,1.),(1.,0.614080890649201,1.),(1.,0.608818559901416,
1.),(1.,0.598549562946725,1.),(1.,0.593542431435649,1.),(1.,0.587544087100298,
1.),(1.,0.586357558941886,1.),(1.,0.58459974489545,1.),(1.,0.584017471589961,
1.),(1.,0.58286065407134,1.),(1.,0.582285714201984,1.),(1.,0.579441033435682,
1.),(1.,0.577255035039604,1.),(1.,0.57099407208922,1.),(1.,0.567215424254483,
1.),(1.,0.562263998546966,1.),(1.,0.56073312267832,1.),(1.,0.557933367235571,
1.),(1.,0.556664483779403,1.),(1.,0.554413089085532,1.),(1.,0.55343057236855,
1.),(1.,0.552191143920635,1.),(1.,0.551817026223423,1.),(1.,0.551150559711954,
1.),(1.,0.550860123121361,1.),(1.,0.550117918145604,1.),(1.,0.54979527502456,
1.),(1.,0.549497678024855,1.),(1.,0.54952272712658,1.),(1.,0.549923199329552,
1.),(1.,0.550298623229659,1.),(1.,0.551401777926261,1.),(1.,0.552129507376673,
1.),(1.,0.553938461937551,1.),(1.,0.555019683583193,1.),(1.,0.55659246824619,
1.),(1.,0.556918368573493,1.),(1.,0.557590793133884,1.),(1.,0.557937171309798,
1.),(1.,0.559006327612528,1.),(1.,0.559759125759416,1.),(1.,0.56213386569043,
1.),(1.,0.563872123771208,1.),(1.,0.567639632538003,1.),(1.,0.56966888369193,
1.),(1.,0.576165737003702,1.),(1.,0.581041953914996,1.),(1.,0.587734307209788,
1.),(1.,0.589102670011644,1.),(1.,0.591198589894367,1.),(1.,0.591904329882334,
1.),(1.,0.593326306107057,1.),(1.,0.59404298699,1.),(1.,0.597653969719517,
1.),(1.,0.600630906054337,1.),(1.,0.609794672912413,1.),(1.,0.616213457755282,
1.),(1.,0.629529817492585,1.),(1.,0.636427647260283,1.),(1.,0.64528002230528,
1.),(1.,0.647062576663052,1.),(1.,0.650647123113913,1.),(1.,0.652446504467237,
1.),(1.,0.657863706040612,1.),(1.,0.661500537891968,1.),(1.,0.668814039957785,
1.),(1.,0.672490718153945,1.),(1.,0.677105532455178,1.),(1.,0.678029446716273,
1.),(1.,0.679879041255836,1.),(1.,0.6808048791055,1.),(1.,0.683580788138606,
1.),(1.,0.685430538496766,1.),(1.,0.694672821737992,1.),(1.,0.702045375777937,
1.),(1.,0.716701955734308,1.),(1.,0.723986149925766,1.),(1.,0.738431955919895,
1.),(1.,0.745593682702893,1.),(1.,0.759767797075294,1.),(1.,0.766780270092341,
1.),(1.,0.777170190252166,1.),(1.,0.780612058728018,1.),(1.,0.785740760463396,
1.),(1.,0.787445924233964,1.),(1.,0.790834278540273,1.),(1.,0.792518300408504,
1.),(1.,0.800887468641132,1.),(1.,0.807419900116371,1.),(1.,0.820153190581628,
1.),(1.,0.826354102318175,1.),(1.,0.838415054767577,1.),(1.,0.844275167314104,
1.),(1.,0.855639785590181,1.),(1.,0.86114440303444,1.),(1.,0.869117500840641,
1.),(1.,0.871727822221485,1.),(1.,0.875569253717761,1.),(1.,0.876838215848048,
1.),(1.,0.879341120217273,1.),(1.,0.880576146721508,1.),(1.,0.886668389923952,
1.),(1.,0.891277339697025,1.),(1.,0.895607410402154,1.)))
REPRESENTATION_ITEM('')
SURFACE()
);
#189=(
BOUNDED_SURFACE()
B_SPLINE_SURFACE(3,2,((#61911,#61912,#61913),(#61914,#61915,#61916),(#61917,
#61918,#61919),(#61920,#61921,#61922),(#61923,#61924,#61925),(#61926,#61927,
#61928),(#61929,#61930,#61931),(#61932,#61933,#61934),(#61935,#61936,#61937),
(#61938,#61939,#61940),(#61941,#61942,#61943),(#61944,#61945,#61946),(#61947,
#61948,#61949),(#61950,#61951,#61952),(#61953,#61954,#61955),(#61956,#61957,
#61958),(#61959,#61960,#61961),(#61962,#61963,#61964),(#61965,#61966,#61967),
(#61968,#61969,#61970),(#61971,#61972,#61973),(#61974,#61975,#61976),(#61977,
#61978,#61979),(#61980,#61981,#61982),(#61983,#61984,#61985),(#61986,#61987,
#61988),(#61989,#61990,#61991),(#61992,#61993,#61994),(#61995,#61996,#61997),
(#61998,#61999,#62000),(#62001,#62002,#62003),(#62004,#62005,#62006),(#62007,
#62008,#62009),(#62010,#62011,#62012),(#62013,#62014,#62015),(#62016,#62017,
#62018),(#62019,#62020,#62021),(#62022,#62023,#62024),(#62025,#62026,#62027),
(#62028,#62029,#62030),(#62031,#62032,#62033),(#62034,#62035,#62036),(#62037,
#62038,#62039),(#62040,#62041,#62042),(#62043,#62044,#62045),(#62046,#62047,
#62048),(#62049,#62050,#62051),(#62052,#62053,#62054),(#62055,#62056,#62057),
(#62058,#62059,#62060),(#62061,#62062,#62063),(#62064,#62065,#62066),(#62067,
#62068,#62069),(#62070,#62071,#62072),(#62073,#62074,#62075),(#62076,#62077,
#62078),(#62079,#62080,#62081),(#62082,#62083,#62084),(#62085,#62086,#62087),
(#62088,#62089,#62090),(#62091,#62092,#62093),(#62094,#62095,#62096),(#62097,
#62098,#62099),(#62100,#62101,#62102),(#62103,#62104,#62105),(#62106,#62107,
#62108),(#62109,#62110,#62111),(#62112,#62113,#62114),(#62115,#62116,#62117),
(#62118,#62119,#62120),(#62121,#62122,#62123),(#62124,#62125,#62126),(#62127,
#62128,#62129),(#62130,#62131,#62132),(#62133,#62134,#62135),(#62136,#62137,
#62138),(#62139,#62140,#62141),(#62142,#62143,#62144),(#62145,#62146,#62147),
(#62148,#62149,#62150),(#62151,#62152,#62153),(#62154,#62155,#62156),(#62157,
#62158,#62159),(#62160,#62161,#62162),(#62163,#62164,#62165),(#62166,#62167,
#62168),(#62169,#62170,#62171),(#62172,#62173,#62174),(#62175,#62176,#62177),
(#62178,#62179,#62180),(#62181,#62182,#62183),(#62184,#62185,#62186),(#62187,
#62188,#62189),(#62190,#62191,#62192),(#62193,#62194,#62195),(#62196,#62197,
#62198),(#62199,#62200,#62201),(#62202,#62203,#62204),(#62205,#62206,#62207),
(#62208,#62209,#62210),(#62211,#62212,#62213),(#62214,#62215,#62216),(#62217,
#62218,#62219),(#62220,#62221,#62222),(#62223,#62224,#62225),(#62226,#62227,
#62228),(#62229,#62230,#62231),(#62232,#62233,#62234),(#62235,#62236,#62237),
(#62238,#62239,#62240),(#62241,#62242,#62243),(#62244,#62245,#62246),(#62247,
#62248,#62249),(#62250,#62251,#62252),(#62253,#62254,#62255),(#62256,#62257,
#62258)),.UNSPECIFIED.,.F.,.F.,.F.)
B_SPLINE_SURFACE_WITH_KNOTS((4,2,2,2,2,2,2,2,2,2,2,2,2,2,2,2,2,2,2,2,2,
2,2,2,2,2,2,2,2,2,2,2,2,2,2,2,2,2,2,2,2,2,2,2,2,2,2,2,2,2,2,2,2,2,2,2,2,
4),(3,3),(0.0134638639862926,0.0138444481692976,0.0142250323523026,0.0144153244438052,
0.0145104704895564,0.0145580435124321,0.0146056165353077,0.0149862007183127,
0.0153667849013178,0.0155570769928203,0.0156046500156959,0.0156522230385716,
0.0157473690843228,0.0161279532673279,0.0165085374503329,0.0166036834960842,
0.0166988295418354,0.0168891216333379,0.017269705816343,0.017650289999348,
0.0178405820908505,0.0179357281366018,0.0180308741823531,0.0184114583653581,
0.0187920425483631,0.0191726267313682,0.0195532109143732,0.0196007839372489,
0.0196483569601245,0.0197435030058757,0.0199337950973783,0.0203143792803833,
0.0206949634633883,0.0210755476463934,0.0211706936921447,0.0212182667150203,
0.0212658397378959,0.0214561318293984,0.0218367160124035,0.0222173001954085,
0.0225978843784136,0.0226930304241648,0.0227406034470404,0.0227881764699161,
0.0229784685614186,0.0233590527444236,0.0237396369274287,0.0239299290189312,
0.0240250750646825,0.0240726480875581,0.0241202211104337,0.0245008052934388,
0.0248813894764438,0.0252619736594488,0.0253095466823245,0.0253571197052001,
0.0254522657509514,0.0256425578424539),(0.,1.),.UNSPECIFIED.)
GEOMETRIC_REPRESENTATION_ITEM()
RATIONAL_B_SPLINE_SURFACE(((1.,0.902225890492542,1.),(1.,0.903132443490707,
1.),(1.,0.903653998020159,1.),(1.,0.903944517231158,1.),(1.,0.903713722905418,
1.),(1.,0.902804847362988,1.),(1.,0.902407978119384,1.),(1.,0.901670791643955,
1.),(1.,0.901401407340477,1.),(1.,0.900961642998138,1.),(1.,0.900809228648317,
1.),(1.,0.900493618235616,1.),(1.,0.900330315112404,1.),(1.,0.898811704236251,
1.),(1.,0.897115152223068,1.),(1.,0.8930832276658,1.),(1.,0.890747678105234,
1.),(1.,0.886791425592428,1.),(1.,0.885397053276724,1.),(1.,0.88356139649318,
1.),(1.,0.883189677780271,1.),(1.,0.882439027225991,1.),(1.,0.882059854491219,
1.),(1.,0.880910975326534,1.),(1.,0.880129910230349,1.),(1.,0.876151119296445,
1.),(1.,0.872733625123037,1.),(1.,0.865476631221263,1.),(1.,0.861636969494005,
1.),(1.,0.856594588614554,1.),(1.,0.855573946399914,1.),(1.,0.85350876220382,
1.),(1.,0.85246323174813,1.),(1.,0.849298841078223,1.),(1.,0.847155538255743,
1.),(1.,0.840632122902037,1.),(1.,0.836158689703462,1.),(1.,0.82699763309876,
1.),(1.,0.822309914051737,1.),(1.,0.815139949640102,1.),(1.,0.812726867725303,
1.),(1.,0.809075207829036,1.),(1.,0.807852647321983,1.),(1.,0.805397269639103,
1.),(1.,0.804163344999755,1.),(1.,0.797982958897003,1.),(1.,0.793019937597689,
1.),(1.,0.783088423023321,1.),(1.,0.778119879402164,1.),(1.,0.76820928668916,
1.),(1.,0.763267195819894,1.),(1.,0.75344296730385,1.),(1.,0.748560790284006,
1.),(1.,0.743122393008669,1.),(1.,0.742518700341634,1.),(1.,0.741315692842442,
1.),(1.,0.740716049307044,1.),(1.,0.738922777819631,1.),(1.,0.737734808757582,
1.),(1.,0.734194170605456,1.),(1.,0.731864767933108,1.),(1.,0.724974784496934,
1.),(1.,0.720512392415405,1.),(1.,0.711877877500243,1.),(1.,0.70770576200713,
1.),(1.,0.699681270084328,1.),(1.,0.69582890373149,1.),(1.,0.691232191837726,
1.),(1.,0.690323788182993,1.),(1.,0.688977948962119,1.),(1.,0.688531815215766,
1.),(1.,0.687646982863273,1.),(1.,0.687208339799286,1.),(1.,0.685033941452217,
1.),(1.,0.68335464007595,1.),(1.,0.678495463402553,1.),(1.,0.675494391175647,
1.),(1.,0.669957389536595,1.),(1.,0.667421498945256,1.),(1.,0.662800458311643,
1.),(1.,0.660715343376615,1.),(1.,0.658379180374724,1.),(1.,0.657925448212519,
1.),(1.,0.6572648494954,1.),(1.,0.657048060234475,1.),(1.,0.656622369647382,
1.),(1.,0.65641330403604,1.),(1.,0.655386526701698,1.),(1.,0.654624456485959,
1.),(1.,0.65250324404021,1.),(1.,0.65130900668008,1.),(1.,0.649293555942829,
1.),(1.,0.648472385523653,1.),(1.,0.647472276924539,1.),(1.,0.64717753120397,
1.),(1.,0.64678743528618,1.),(1.,0.646666074433016,1.),(1.,0.646496305039786,
1.),(1.,0.646441723439099,1.),(1.,0.646336727153311,1.),(1.,0.646286326879338,
1.),(1.,0.6458508188832,1.),(1.,0.645591760552018,1.),(1.,0.645249142331117,
1.),(1.,0.645165683168743,1.),(1.,0.645106841085182,1.),(1.,0.645131514983531,
1.),(1.,0.645188093182711,1.),(1.,0.645194786243544,1.),(1.,0.645208884878214,
1.),(1.,0.645216298795827,1.),(1.,0.64523934086315,1.),(1.,0.645255850813146,
1.),(1.,0.645307638180231,1.),(1.,0.645345156614371,1.),(1.,0.64538287972702,
1.)))
REPRESENTATION_ITEM('')
SURFACE()
);
#190=(
BOUNDED_SURFACE()
B_SPLINE_SURFACE(3,2,((#62260,#62261,#62262),(#62263,#62264,#62265),(#62266,
#62267,#62268),(#62269,#62270,#62271),(#62272,#62273,#62274),(#62275,#62276,
#62277),(#62278,#62279,#62280),(#62281,#62282,#62283),(#62284,#62285,#62286),
(#62287,#62288,#62289),(#62290,#62291,#62292),(#62293,#62294,#62295)),
 .UNSPECIFIED.,.F.,.F.,.F.)
B_SPLINE_SURFACE_WITH_KNOTS((4,2,2,2,2,4),(3,3),(-4.34222970080445E-17,
0.000193738907016803,0.000387477814033649,0.000484347267542072,0.000581216721050495,
0.000774955628067341),(0.,1.),.UNSPECIFIED.)
GEOMETRIC_REPRESENTATION_ITEM()
RATIONAL_B_SPLINE_SURFACE(((1.,0.902225890492542,1.),(1.,0.900702231639175,
1.),(1.,0.898361639865931,1.),(1.,0.892256701302875,1.),(1.,0.88849270261023,
1.),(1.,0.881893015251816,1.),(1.,0.87953374069531,1.),(1.,0.87451093966713,
1.),(1.,0.871866113555864,1.),(1.,0.863573635793879,1.),(1.,0.857564565511076,
1.),(1.,0.851143038957624,1.)))
REPRESENTATION_ITEM('')
SURFACE()
);
#191=(
BOUNDED_SURFACE()
B_SPLINE_SURFACE(3,2,((#62297,#62298,#62299),(#62300,#62301,#62302),(#62303,
#62304,#62305),(#62306,#62307,#62308),(#62309,#62310,#62311),(#62312,#62313,
#62314),(#62315,#62316,#62317),(#62318,#62319,#62320),(#62321,#62322,#62323),
(#62324,#62325,#62326),(#62327,#62328,#62329),(#62330,#62331,#62332),(#62333,
#62334,#62335),(#62336,#62337,#62338),(#62339,#62340,#62341),(#62342,#62343,
#62344),(#62345,#62346,#62347),(#62348,#62349,#62350),(#62351,#62352,#62353),
(#62354,#62355,#62356),(#62357,#62358,#62359),(#62360,#62361,#62362),(#62363,
#62364,#62365),(#62366,#62367,#62368),(#62369,#62370,#62371),(#62372,#62373,
#62374),(#62375,#62376,#62377),(#62378,#62379,#62380),(#62381,#62382,#62383),
(#62384,#62385,#62386),(#62387,#62388,#62389),(#62390,#62391,#62392),(#62393,
#62394,#62395),(#62396,#62397,#62398),(#62399,#62400,#62401),(#62402,#62403,
#62404),(#62405,#62406,#62407),(#62408,#62409,#62410),(#62411,#62412,#62413),
(#62414,#62415,#62416),(#62417,#62418,#62419),(#62420,#62421,#62422),(#62423,
#62424,#62425),(#62426,#62427,#62428),(#62429,#62430,#62431),(#62432,#62433,
#62434),(#62435,#62436,#62437),(#62438,#62439,#62440),(#62441,#62442,#62443),
(#62444,#62445,#62446),(#62447,#62448,#62449),(#62450,#62451,#62452),(#62453,
#62454,#62455),(#62456,#62457,#62458),(#62459,#62460,#62461),(#62462,#62463,
#62464),(#62465,#62466,#62467),(#62468,#62469,#62470),(#62471,#62472,#62473),
(#62474,#62475,#62476),(#62477,#62478,#62479),(#62480,#62481,#62482),(#62483,
#62484,#62485),(#62486,#62487,#62488),(#62489,#62490,#62491),(#62492,#62493,
#62494),(#62495,#62496,#62497),(#62498,#62499,#62500),(#62501,#62502,#62503),
(#62504,#62505,#62506),(#62507,#62508,#62509),(#62510,#62511,#62512),(#62513,
#62514,#62515),(#62516,#62517,#62518),(#62519,#62520,#62521),(#62522,#62523,
#62524),(#62525,#62526,#62527),(#62528,#62529,#62530),(#62531,#62532,#62533),
(#62534,#62535,#62536),(#62537,#62538,#62539),(#62540,#62541,#62542),(#62543,
#62544,#62545),(#62546,#62547,#62548),(#62549,#62550,#62551),(#62552,#62553,
#62554),(#62555,#62556,#62557),(#62558,#62559,#62560),(#62561,#62562,#62563),
(#62564,#62565,#62566),(#62567,#62568,#62569),(#62570,#62571,#62572),(#62573,
#62574,#62575),(#62576,#62577,#62578),(#62579,#62580,#62581),(#62582,#62583,
#62584),(#62585,#62586,#62587),(#62588,#62589,#62590),(#62591,#62592,#62593),
(#62594,#62595,#62596),(#62597,#62598,#62599),(#62600,#62601,#62602)),
 .UNSPECIFIED.,.F.,.F.,.F.)
B_SPLINE_SURFACE_WITH_KNOTS((4,2,2,2,2,2,2,2,2,2,2,2,2,2,2,2,2,2,2,2,2,
2,2,2,2,2,2,2,2,2,2,2,2,2,2,2,2,2,2,2,2,2,2,2,2,2,2,2,2,2,4),(3,3),(0.0137607578966189,
0.0141248143649128,0.0144888708332067,0.0148529273015007,0.0152169837697946,
0.0155810402380886,0.015672054355162,0.0157630684722355,0.0159450967063825,
0.0163091531746764,0.0166732096429704,0.0170372661112643,0.0174013225795583,
0.0175833508137052,0.0176743649307787,0.0177653790478522,0.0181294355161461,
0.0184934919844401,0.018857548452734,0.019039576686881,0.0191305908039545,
0.019221604921028,0.0195856613893219,0.0199497178576158,0.0203137743259098,
0.0203592813844465,0.0204047884429833,0.0204958025600567,0.0206778307942037,
0.0210418872624977,0.0214059437307916,0.0215879719649386,0.0216789860820121,
0.0217700001990855,0.0221340566673795,0.0224981131356734,0.0226801413698204,
0.0227256484283571,0.0227711554868939,0.0228621696039674,0.0232262260722613,
0.0235902825405552,0.0237723107747022,0.0238633248917757,0.0239543390088492,
0.0243183954771431,0.0246824519454371,0.025046508413731,0.0251375225308045,
0.025228536647878,0.0254105648820249),(0.,1.),.UNSPECIFIED.)
GEOMETRIC_REPRESENTATION_ITEM()
RATIONAL_B_SPLINE_SURFACE(((1.,0.851143038957625,1.),(1.,0.846479387833395,
1.),(1.,0.841684047649747,1.),(1.,0.831843628329292,1.),(1.,0.826798581401555,
1.),(1.,0.816468255419326,1.),(1.,0.811182939537333,1.),(1.,0.800378089079313,
1.),(1.,0.79485852833921,1.),(1.,0.783588798399719,1.),(1.,0.77783860835381,
1.),(1.,0.770507923158056,1.),(1.,0.769034635357085,1.),(1.,0.766073776121258,
1.),(1.,0.764586399638179,1.),(1.,0.760117744617778,1.),(1.,0.757125076740806,
1.),(1.,0.748108634667927,1.),(1.,0.742046356031758,1.),(1.,0.729832440045022,
1.),(1.,0.723680764192416,1.),(1.,0.711303823843107,1.),(1.,0.705078509161493,
1.),(1.,0.6925739237358,1.),(1.,0.686294583365353,1.),(1.,0.676854046105913,
1.),(1.,0.673703662794336,1.),(1.,0.668975704676001,1.),(1.,0.667399235894792,
1.),(1.,0.664246417134242,1.),(1.,0.662674576423675,1.),(1.,0.654839788640746,
1.),(1.,0.648649695295625,1.),(1.,0.636471040983231,1.),(1.,0.630482388018559,
1.),(1.,0.618763892218915,1.),(1.,0.613033921427266,1.),(1.,0.604686972618327,
1.),(1.,0.601946116421347,1.),(1.,0.597905078993139,1.),(1.,0.596569784084661,
1.),(1.,0.593924099614706,1.),(1.,0.592613436616545,1.),(1.,0.586158271598212,
1.),(1.,0.581281465080226,1.),(1.,0.572174439101757,1.),(1.,0.567944193517853,
1.),(1.,0.560213073119294,1.),(1.,0.55671214421852,1.),(1.,0.553237178148869,
1.),(1.,0.55285751778881,1.),(1.,0.55211129142054,1.),(1.,0.551744475791875,
1.),(1.,0.550665824157476,1.),(1.,0.549976737095303,1.),(1.,0.54799961392759,
1.),(1.,0.546801718122489,1.),(1.,0.543569310149808,1.),(1.,0.54189614782828,
1.),(1.,0.539515970413853,1.),(1.,0.53880894909132,1.),(1.,0.538473378107389,
1.),(1.,0.538482331182785,1.),(1.,0.538676931129144,1.),(1.,0.538772236119652,
1.),(1.,0.539021359113027,1.),(1.,0.539175170865797,1.),(1.,0.540085972132753,
1.),(1.,0.541267672929542,1.),(1.,0.544430358927514,1.),(1.,0.546411368970525,
1.),(1.,0.549911779882456,1.),(1.,0.551166829738738,1.),(1.,0.552839328341023,
1.),(1.,0.553179014364036,1.),(1.,0.553868601162557,1.),(1.,0.554218660677656,
1.),(1.,0.555280888150674,1.),(1.,0.55600596370185,1.),(1.,0.559710766897414,
1.),(1.,0.562927650586242,1.),(1.,0.569753621382414,1.),(1.,0.573362909796628,
1.),(1.,0.579004661887682,1.),(1.,0.580923392305157,1.),(1.,0.58385183530157,
1.),(1.,0.584836827643457,1.),(1.,0.586820704360992,1.),(1.,0.587816792889683,
1.),(1.,0.592815092417132,1.),(1.,0.596870022611588,1.),(1.,0.605033066578426,
1.),(1.,0.609141359017907,1.),(1.,0.617370572384848,1.),(1.,0.621491593376493,
1.),(1.,0.626634299394224,1.),(1.,0.627661241677736,1.),(1.,0.629705159449786,
1.),(1.,0.630723104403595,1.),(1.,0.633764717654218,1.),(1.,0.635776155601376,
1.),(1.,0.637771010909975,1.)))
REPRESENTATION_ITEM('')
SURFACE()
);
#192=B_SPLINE_SURFACE_WITH_KNOTS('',3,3,((#21716,#21717,#21718,#21719,#21720,
#21721,#21722,#21723,#21724,#21725,#21726,#21727,#21728,#21729,#21730,#21731,
#21732,#21733,#21734,#21735,#21736,#21737,#21738,#21739,#21740,#21741,#21742,
#21743,#21744,#21745,#21746,#21747,#21748,#21749,#21750,#21751,#21752,#21753,
#21754,#21755,#21756,#21757,#21758,#21759,#21760,#21761,#21762,#21763,#21764),
(#21765,#21766,#21767,#21768,#21769,#21770,#21771,#21772,#21773,#21774,
#21775,#21776,#21777,#21778,#21779,#21780,#21781,#21782,#21783,#21784,#21785,
#21786,#21787,#21788,#21789,#21790,#21791,#21792,#21793,#21794,#21795,#21796,
#21797,#21798,#21799,#21800,#21801,#21802,#21803,#21804,#21805,#21806,#21807,
#21808,#21809,#21810,#21811,#21812,#21813),(#21814,#21815,#21816,#21817,
#21818,#21819,#21820,#21821,#21822,#21823,#21824,#21825,#21826,#21827,#21828,
#21829,#21830,#21831,#21832,#21833,#21834,#21835,#21836,#21837,#21838,#21839,
#21840,#21841,#21842,#21843,#21844,#21845,#21846,#21847,#21848,#21849,#21850,
#21851,#21852,#21853,#21854,#21855,#21856,#21857,#21858,#21859,#21860,#21861,
#21862),(#21863,#21864,#21865,#21866,#21867,#21868,#21869,#21870,#21871,
#21872,#21873,#21874,#21875,#21876,#21877,#21878,#21879,#21880,#21881,#21882,
#21883,#21884,#21885,#21886,#21887,#21888,#21889,#21890,#21891,#21892,#21893,
#21894,#21895,#21896,#21897,#21898,#21899,#21900,#21901,#21902,#21903,#21904,
#21905,#21906,#21907,#21908,#21909,#21910,#21911),(#21912,#21913,#21914,
#21915,#21916,#21917,#21918,#21919,#21920,#21921,#21922,#21923,#21924,#21925,
#21926,#21927,#21928,#21929,#21930,#21931,#21932,#21933,#21934,#21935,#21936,
#21937,#21938,#21939,#21940,#21941,#21942,#21943,#21944,#21945,#21946,#21947,
#21948,#21949,#21950,#21951,#21952,#21953,#21954,#21955,#21956,#21957,#21958,
#21959,#21960),(#21961,#21962,#21963,#21964,#21965,#21966,#21967,#21968,
#21969,#21970,#21971,#21972,#21973,#21974,#21975,#21976,#21977,#21978,#21979,
#21980,#21981,#21982,#21983,#21984,#21985,#21986,#21987,#21988,#21989,#21990,
#21991,#21992,#21993,#21994,#21995,#21996,#21997,#21998,#21999,#22000,#22001,
#22002,#22003,#22004,#22005,#22006,#22007,#22008,#22009),(#22010,#22011,
#22012,#22013,#22014,#22015,#22016,#22017,#22018,#22019,#22020,#22021,#22022,
#22023,#22024,#22025,#22026,#22027,#22028,#22029,#22030,#22031,#22032,#22033,
#22034,#22035,#22036,#22037,#22038,#22039,#22040,#22041,#22042,#22043,#22044,
#22045,#22046,#22047,#22048,#22049,#22050,#22051,#22052,#22053,#22054,#22055,
#22056,#22057,#22058),(#22059,#22060,#22061,#22062,#22063,#22064,#22065,
#22066,#22067,#22068,#22069,#22070,#22071,#22072,#22073,#22074,#22075,#22076,
#22077,#22078,#22079,#22080,#22081,#22082,#22083,#22084,#22085,#22086,#22087,
#22088,#22089,#22090,#22091,#22092,#22093,#22094,#22095,#22096,#22097,#22098,
#22099,#22100,#22101,#22102,#22103,#22104,#22105,#22106,#22107),(#22108,
#22109,#22110,#22111,#22112,#22113,#22114,#22115,#22116,#22117,#22118,#22119,
#22120,#22121,#22122,#22123,#22124,#22125,#22126,#22127,#22128,#22129,#22130,
#22131,#22132,#22133,#22134,#22135,#22136,#22137,#22138,#22139,#22140,#22141,
#22142,#22143,#22144,#22145,#22146,#22147,#22148,#22149,#22150,#22151,#22152,
#22153,#22154,#22155,#22156),(#22157,#22158,#22159,#22160,#22161,#22162,
#22163,#22164,#22165,#22166,#22167,#22168,#22169,#22170,#22171,#22172,#22173,
#22174,#22175,#22176,#22177,#22178,#22179,#22180,#22181,#22182,#22183,#22184,
#22185,#22186,#22187,#22188,#22189,#22190,#22191,#22192,#22193,#22194,#22195,
#22196,#22197,#22198,#22199,#22200,#22201,#22202,#22203,#22204,#22205),
(#22206,#22207,#22208,#22209,#22210,#22211,#22212,#22213,#22214,#22215,
#22216,#22217,#22218,#22219,#22220,#22221,#22222,#22223,#22224,#22225,#22226,
#22227,#22228,#22229,#22230,#22231,#22232,#22233,#22234,#22235,#22236,#22237,
#22238,#22239,#22240,#22241,#22242,#22243,#22244,#22245,#22246,#22247,#22248,
#22249,#22250,#22251,#22252,#22253,#22254),(#22255,#22256,#22257,#22258,
#22259,#22260,#22261,#22262,#22263,#22264,#22265,#22266,#22267,#22268,#22269,
#22270,#22271,#22272,#22273,#22274,#22275,#22276,#22277,#22278,#22279,#22280,
#22281,#22282,#22283,#22284,#22285,#22286,#22287,#22288,#22289,#22290,#22291,
#22292,#22293,#22294,#22295,#22296,#22297,#22298,#22299,#22300,#22301,#22302,
#22303),(#22304,#22305,#22306,#22307,#22308,#22309,#22310,#22311,#22312,
#22313,#22314,#22315,#22316,#22317,#22318,#22319,#22320,#22321,#22322,#22323,
#22324,#22325,#22326,#22327,#22328,#22329,#22330,#22331,#22332,#22333,#22334,
#22335,#22336,#22337,#22338,#22339,#22340,#22341,#22342,#22343,#22344,#22345,
#22346,#22347,#22348,#22349,#22350,#22351,#22352),(#22353,#22354,#22355,
#22356,#22357,#22358,#22359,#22360,#22361,#22362,#22363,#22364,#22365,#22366,
#22367,#22368,#22369,#22370,#22371,#22372,#22373,#22374,#22375,#22376,#22377,
#22378,#22379,#22380,#22381,#22382,#22383,#22384,#22385,#22386,#22387,#22388,
#22389,#22390,#22391,#22392,#22393,#22394,#22395,#22396,#22397,#22398,#22399,
#22400,#22401),(#22402,#22403,#22404,#22405,#22406,#22407,#22408,#22409,
#22410,#22411,#22412,#22413,#22414,#22415,#22416,#22417,#22418,#22419,#22420,
#22421,#22422,#22423,#22424,#22425,#22426,#22427,#22428,#22429,#22430,#22431,
#22432,#22433,#22434,#22435,#22436,#22437,#22438,#22439,#22440,#22441,#22442,
#22443,#22444,#22445,#22446,#22447,#22448,#22449,#22450),(#22451,#22452,
#22453,#22454,#22455,#22456,#22457,#22458,#22459,#22460,#22461,#22462,#22463,
#22464,#22465,#22466,#22467,#22468,#22469,#22470,#22471,#22472,#22473,#22474,
#22475,#22476,#22477,#22478,#22479,#22480,#22481,#22482,#22483,#22484,#22485,
#22486,#22487,#22488,#22489,#22490,#22491,#22492,#22493,#22494,#22495,#22496,
#22497,#22498,#22499),(#22500,#22501,#22502,#22503,#22504,#22505,#22506,
#22507,#22508,#22509,#22510,#22511,#22512,#22513,#22514,#22515,#22516,#22517,
#22518,#22519,#22520,#22521,#22522,#22523,#22524,#22525,#22526,#22527,#22528,
#22529,#22530,#22531,#22532,#22533,#22534,#22535,#22536,#22537,#22538,#22539,
#22540,#22541,#22542,#22543,#22544,#22545,#22546,#22547,#22548),(#22549,
#22550,#22551,#22552,#22553,#22554,#22555,#22556,#22557,#22558,#22559,#22560,
#22561,#22562,#22563,#22564,#22565,#22566,#22567,#22568,#22569,#22570,#22571,
#22572,#22573,#22574,#22575,#22576,#22577,#22578,#22579,#22580,#22581,#22582,
#22583,#22584,#22585,#22586,#22587,#22588,#22589,#22590,#22591,#22592,#22593,
#22594,#22595,#22596,#22597),(#22598,#22599,#22600,#22601,#22602,#22603,
#22604,#22605,#22606,#22607,#22608,#22609,#22610,#22611,#22612,#22613,#22614,
#22615,#22616,#22617,#22618,#22619,#22620,#22621,#22622,#22623,#22624,#22625,
#22626,#22627,#22628,#22629,#22630,#22631,#22632,#22633,#22634,#22635,#22636,
#22637,#22638,#22639,#22640,#22641,#22642,#22643,#22644,#22645,#22646),
(#22647,#22648,#22649,#22650,#22651,#22652,#22653,#22654,#22655,#22656,
#22657,#22658,#22659,#22660,#22661,#22662,#22663,#22664,#22665,#22666,#22667,
#22668,#22669,#22670,#22671,#22672,#22673,#22674,#22675,#22676,#22677,#22678,
#22679,#22680,#22681,#22682,#22683,#22684,#22685,#22686,#22687,#22688,#22689,
#22690,#22691,#22692,#22693,#22694,#22695),(#22696,#22697,#22698,#22699,
#22700,#22701,#22702,#22703,#22704,#22705,#22706,#22707,#22708,#22709,#22710,
#22711,#22712,#22713,#22714,#22715,#22716,#22717,#22718,#22719,#22720,#22721,
#22722,#22723,#22724,#22725,#22726,#22727,#22728,#22729,#22730,#22731,#22732,
#22733,#22734,#22735,#22736,#22737,#22738,#22739,#22740,#22741,#22742,#22743,
#22744),(#22745,#22746,#22747,#22748,#22749,#22750,#22751,#22752,#22753,
#22754,#22755,#22756,#22757,#22758,#22759,#22760,#22761,#22762,#22763,#22764,
#22765,#22766,#22767,#22768,#22769,#22770,#22771,#22772,#22773,#22774,#22775,
#22776,#22777,#22778,#22779,#22780,#22781,#22782,#22783,#22784,#22785,#22786,
#22787,#22788,#22789,#22790,#22791,#22792,#22793),(#22794,#22795,#22796,
#22797,#22798,#22799,#22800,#22801,#22802,#22803,#22804,#22805,#22806,#22807,
#22808,#22809,#22810,#22811,#22812,#22813,#22814,#22815,#22816,#22817,#22818,
#22819,#22820,#22821,#22822,#22823,#22824,#22825,#22826,#22827,#22828,#22829,
#22830,#22831,#22832,#22833,#22834,#22835,#22836,#22837,#22838,#22839,#22840,
#22841,#22842),(#22843,#22844,#22845,#22846,#22847,#22848,#22849,#22850,
#22851,#22852,#22853,#22854,#22855,#22856,#22857,#22858,#22859,#22860,#22861,
#22862,#22863,#22864,#22865,#22866,#22867,#22868,#22869,#22870,#22871,#22872,
#22873,#22874,#22875,#22876,#22877,#22878,#22879,#22880,#22881,#22882,#22883,
#22884,#22885,#22886,#22887,#22888,#22889,#22890,#22891),(#22892,#22893,
#22894,#22895,#22896,#22897,#22898,#22899,#22900,#22901,#22902,#22903,#22904,
#22905,#22906,#22907,#22908,#22909,#22910,#22911,#22912,#22913,#22914,#22915,
#22916,#22917,#22918,#22919,#22920,#22921,#22922,#22923,#22924,#22925,#22926,
#22927,#22928,#22929,#22930,#22931,#22932,#22933,#22934,#22935,#22936,#22937,
#22938,#22939,#22940),(#22941,#22942,#22943,#22944,#22945,#22946,#22947,
#22948,#22949,#22950,#22951,#22952,#22953,#22954,#22955,#22956,#22957,#22958,
#22959,#22960,#22961,#22962,#22963,#22964,#22965,#22966,#22967,#22968,#22969,
#22970,#22971,#22972,#22973,#22974,#22975,#22976,#22977,#22978,#22979,#22980,
#22981,#22982,#22983,#22984,#22985,#22986,#22987,#22988,#22989),(#22990,
#22991,#22992,#22993,#22994,#22995,#22996,#22997,#22998,#22999,#23000,#23001,
#23002,#23003,#23004,#23005,#23006,#23007,#23008,#23009,#23010,#23011,#23012,
#23013,#23014,#23015,#23016,#23017,#23018,#23019,#23020,#23021,#23022,#23023,
#23024,#23025,#23026,#23027,#23028,#23029,#23030,#23031,#23032,#23033,#23034,
#23035,#23036,#23037,#23038),(#23039,#23040,#23041,#23042,#23043,#23044,
#23045,#23046,#23047,#23048,#23049,#23050,#23051,#23052,#23053,#23054,#23055,
#23056,#23057,#23058,#23059,#23060,#23061,#23062,#23063,#23064,#23065,#23066,
#23067,#23068,#23069,#23070,#23071,#23072,#23073,#23074,#23075,#23076,#23077,
#23078,#23079,#23080,#23081,#23082,#23083,#23084,#23085,#23086,#23087),
(#23088,#23089,#23090,#23091,#23092,#23093,#23094,#23095,#23096,#23097,
#23098,#23099,#23100,#23101,#23102,#23103,#23104,#23105,#23106,#23107,#23108,
#23109,#23110,#23111,#23112,#23113,#23114,#23115,#23116,#23117,#23118,#23119,
#23120,#23121,#23122,#23123,#23124,#23125,#23126,#23127,#23128,#23129,#23130,
#23131,#23132,#23133,#23134,#23135,#23136),(#23137,#23138,#23139,#23140,
#23141,#23142,#23143,#23144,#23145,#23146,#23147,#23148,#23149,#23150,#23151,
#23152,#23153,#23154,#23155,#23156,#23157,#23158,#23159,#23160,#23161,#23162,
#23163,#23164,#23165,#23166,#23167,#23168,#23169,#23170,#23171,#23172,#23173,
#23174,#23175,#23176,#23177,#23178,#23179,#23180,#23181,#23182,#23183,#23184,
#23185),(#23186,#23187,#23188,#23189,#23190,#23191,#23192,#23193,#23194,
#23195,#23196,#23197,#23198,#23199,#23200,#23201,#23202,#23203,#23204,#23205,
#23206,#23207,#23208,#23209,#23210,#23211,#23212,#23213,#23214,#23215,#23216,
#23217,#23218,#23219,#23220,#23221,#23222,#23223,#23224,#23225,#23226,#23227,
#23228,#23229,#23230,#23231,#23232,#23233,#23234),(#23235,#23236,#23237,
#23238,#23239,#23240,#23241,#23242,#23243,#23244,#23245,#23246,#23247,#23248,
#23249,#23250,#23251,#23252,#23253,#23254,#23255,#23256,#23257,#23258,#23259,
#23260,#23261,#23262,#23263,#23264,#23265,#23266,#23267,#23268,#23269,#23270,
#23271,#23272,#23273,#23274,#23275,#23276,#23277,#23278,#23279,#23280,#23281,
#23282,#23283),(#23284,#23285,#23286,#23287,#23288,#23289,#23290,#23291,
#23292,#23293,#23294,#23295,#23296,#23297,#23298,#23299,#23300,#23301,#23302,
#23303,#23304,#23305,#23306,#23307,#23308,#23309,#23310,#23311,#23312,#23313,
#23314,#23315,#23316,#23317,#23318,#23319,#23320,#23321,#23322,#23323,#23324,
#23325,#23326,#23327,#23328,#23329,#23330,#23331,#23332),(#23333,#23334,
#23335,#23336,#23337,#23338,#23339,#23340,#23341,#23342,#23343,#23344,#23345,
#23346,#23347,#23348,#23349,#23350,#23351,#23352,#23353,#23354,#23355,#23356,
#23357,#23358,#23359,#23360,#23361,#23362,#23363,#23364,#23365,#23366,#23367,
#23368,#23369,#23370,#23371,#23372,#23373,#23374,#23375,#23376,#23377,#23378,
#23379,#23380,#23381),(#23382,#23383,#23384,#23385,#23386,#23387,#23388,
#23389,#23390,#23391,#23392,#23393,#23394,#23395,#23396,#23397,#23398,#23399,
#23400,#23401,#23402,#23403,#23404,#23405,#23406,#23407,#23408,#23409,#23410,
#23411,#23412,#23413,#23414,#23415,#23416,#23417,#23418,#23419,#23420,#23421,
#23422,#23423,#23424,#23425,#23426,#23427,#23428,#23429,#23430),(#23431,
#23432,#23433,#23434,#23435,#23436,#23437,#23438,#23439,#23440,#23441,#23442,
#23443,#23444,#23445,#23446,#23447,#23448,#23449,#23450,#23451,#23452,#23453,
#23454,#23455,#23456,#23457,#23458,#23459,#23460,#23461,#23462,#23463,#23464,
#23465,#23466,#23467,#23468,#23469,#23470,#23471,#23472,#23473,#23474,#23475,
#23476,#23477,#23478,#23479),(#23480,#23481,#23482,#23483,#23484,#23485,
#23486,#23487,#23488,#23489,#23490,#23491,#23492,#23493,#23494,#23495,#23496,
#23497,#23498,#23499,#23500,#23501,#23502,#23503,#23504,#23505,#23506,#23507,
#23508,#23509,#23510,#23511,#23512,#23513,#23514,#23515,#23516,#23517,#23518,
#23519,#23520,#23521,#23522,#23523,#23524,#23525,#23526,#23527,#23528),
(#23529,#23530,#23531,#23532,#23533,#23534,#23535,#23536,#23537,#23538,
#23539,#23540,#23541,#23542,#23543,#23544,#23545,#23546,#23547,#23548,#23549,
#23550,#23551,#23552,#23553,#23554,#23555,#23556,#23557,#23558,#23559,#23560,
#23561,#23562,#23563,#23564,#23565,#23566,#23567,#23568,#23569,#23570,#23571,
#23572,#23573,#23574,#23575,#23576,#23577),(#23578,#23579,#23580,#23581,
#23582,#23583,#23584,#23585,#23586,#23587,#23588,#23589,#23590,#23591,#23592,
#23593,#23594,#23595,#23596,#23597,#23598,#23599,#23600,#23601,#23602,#23603,
#23604,#23605,#23606,#23607,#23608,#23609,#23610,#23611,#23612,#23613,#23614,
#23615,#23616,#23617,#23618,#23619,#23620,#23621,#23622,#23623,#23624,#23625,
#23626),(#23627,#23628,#23629,#23630,#23631,#23632,#23633,#23634,#23635,
#23636,#23637,#23638,#23639,#23640,#23641,#23642,#23643,#23644,#23645,#23646,
#23647,#23648,#23649,#23650,#23651,#23652,#23653,#23654,#23655,#23656,#23657,
#23658,#23659,#23660,#23661,#23662,#23663,#23664,#23665,#23666,#23667,#23668,
#23669,#23670,#23671,#23672,#23673,#23674,#23675),(#23676,#23677,#23678,
#23679,#23680,#23681,#23682,#23683,#23684,#23685,#23686,#23687,#23688,#23689,
#23690,#23691,#23692,#23693,#23694,#23695,#23696,#23697,#23698,#23699,#23700,
#23701,#23702,#23703,#23704,#23705,#23706,#23707,#23708,#23709,#23710,#23711,
#23712,#23713,#23714,#23715,#23716,#23717,#23718,#23719,#23720,#23721,#23722,
#23723,#23724),(#23725,#23726,#23727,#23728,#23729,#23730,#23731,#23732,
#23733,#23734,#23735,#23736,#23737,#23738,#23739,#23740,#23741,#23742,#23743,
#23744,#23745,#23746,#23747,#23748,#23749,#23750,#23751,#23752,#23753,#23754,
#23755,#23756,#23757,#23758,#23759,#23760,#23761,#23762,#23763,#23764,#23765,
#23766,#23767,#23768,#23769,#23770,#23771,#23772,#23773),(#23774,#23775,
#23776,#23777,#23778,#23779,#23780,#23781,#23782,#23783,#23784,#23785,#23786,
#23787,#23788,#23789,#23790,#23791,#23792,#23793,#23794,#23795,#23796,#23797,
#23798,#23799,#23800,#23801,#23802,#23803,#23804,#23805,#23806,#23807,#23808,
#23809,#23810,#23811,#23812,#23813,#23814,#23815,#23816,#23817,#23818,#23819,
#23820,#23821,#23822),(#23823,#23824,#23825,#23826,#23827,#23828,#23829,
#23830,#23831,#23832,#23833,#23834,#23835,#23836,#23837,#23838,#23839,#23840,
#23841,#23842,#23843,#23844,#23845,#23846,#23847,#23848,#23849,#23850,#23851,
#23852,#23853,#23854,#23855,#23856,#23857,#23858,#23859,#23860,#23861,#23862,
#23863,#23864,#23865,#23866,#23867,#23868,#23869,#23870,#23871),(#23872,
#23873,#23874,#23875,#23876,#23877,#23878,#23879,#23880,#23881,#23882,#23883,
#23884,#23885,#23886,#23887,#23888,#23889,#23890,#23891,#23892,#23893,#23894,
#23895,#23896,#23897,#23898,#23899,#23900,#23901,#23902,#23903,#23904,#23905,
#23906,#23907,#23908,#23909,#23910,#23911,#23912,#23913,#23914,#23915,#23916,
#23917,#23918,#23919,#23920),(#23921,#23922,#23923,#23924,#23925,#23926,
#23927,#23928,#23929,#23930,#23931,#23932,#23933,#23934,#23935,#23936,#23937,
#23938,#23939,#23940,#23941,#23942,#23943,#23944,#23945,#23946,#23947,#23948,
#23949,#23950,#23951,#23952,#23953,#23954,#23955,#23956,#23957,#23958,#23959,
#23960,#23961,#23962,#23963,#23964,#23965,#23966,#23967,#23968,#23969),
(#23970,#23971,#23972,#23973,#23974,#23975,#23976,#23977,#23978,#23979,
#23980,#23981,#23982,#23983,#23984,#23985,#23986,#23987,#23988,#23989,#23990,
#23991,#23992,#23993,#23994,#23995,#23996,#23997,#23998,#23999,#24000,#24001,
#24002,#24003,#24004,#24005,#24006,#24007,#24008,#24009,#24010,#24011,#24012,
#24013,#24014,#24015,#24016,#24017,#24018),(#24019,#24020,#24021,#24022,
#24023,#24024,#24025,#24026,#24027,#24028,#24029,#24030,#24031,#24032,#24033,
#24034,#24035,#24036,#24037,#24038,#24039,#24040,#24041,#24042,#24043,#24044,
#24045,#24046,#24047,#24048,#24049,#24050,#24051,#24052,#24053,#24054,#24055,
#24056,#24057,#24058,#24059,#24060,#24061,#24062,#24063,#24064,#24065,#24066,
#24067),(#24068,#24069,#24070,#24071,#24072,#24073,#24074,#24075,#24076,
#24077,#24078,#24079,#24080,#24081,#24082,#24083,#24084,#24085,#24086,#24087,
#24088,#24089,#24090,#24091,#24092,#24093,#24094,#24095,#24096,#24097,#24098,
#24099,#24100,#24101,#24102,#24103,#24104,#24105,#24106,#24107,#24108,#24109,
#24110,#24111,#24112,#24113,#24114,#24115,#24116),(#24117,#24118,#24119,
#24120,#24121,#24122,#24123,#24124,#24125,#24126,#24127,#24128,#24129,#24130,
#24131,#24132,#24133,#24134,#24135,#24136,#24137,#24138,#24139,#24140,#24141,
#24142,#24143,#24144,#24145,#24146,#24147,#24148,#24149,#24150,#24151,#24152,
#24153,#24154,#24155,#24156,#24157,#24158,#24159,#24160,#24161,#24162,#24163,
#24164,#24165),(#24166,#24167,#24168,#24169,#24170,#24171,#24172,#24173,
#24174,#24175,#24176,#24177,#24178,#24179,#24180,#24181,#24182,#24183,#24184,
#24185,#24186,#24187,#24188,#24189,#24190,#24191,#24192,#24193,#24194,#24195,
#24196,#24197,#24198,#24199,#24200,#24201,#24202,#24203,#24204,#24205,#24206,
#24207,#24208,#24209,#24210,#24211,#24212,#24213,#24214),(#24215,#24216,
#24217,#24218,#24219,#24220,#24221,#24222,#24223,#24224,#24225,#24226,#24227,
#24228,#24229,#24230,#24231,#24232,#24233,#24234,#24235,#24236,#24237,#24238,
#24239,#24240,#24241,#24242,#24243,#24244,#24245,#24246,#24247,#24248,#24249,
#24250,#24251,#24252,#24253,#24254,#24255,#24256,#24257,#24258,#24259,#24260,
#24261,#24262,#24263),(#24264,#24265,#24266,#24267,#24268,#24269,#24270,
#24271,#24272,#24273,#24274,#24275,#24276,#24277,#24278,#24279,#24280,#24281,
#24282,#24283,#24284,#24285,#24286,#24287,#24288,#24289,#24290,#24291,#24292,
#24293,#24294,#24295,#24296,#24297,#24298,#24299,#24300,#24301,#24302,#24303,
#24304,#24305,#24306,#24307,#24308,#24309,#24310,#24311,#24312),(#24313,
#24314,#24315,#24316,#24317,#24318,#24319,#24320,#24321,#24322,#24323,#24324,
#24325,#24326,#24327,#24328,#24329,#24330,#24331,#24332,#24333,#24334,#24335,
#24336,#24337,#24338,#24339,#24340,#24341,#24342,#24343,#24344,#24345,#24346,
#24347,#24348,#24349,#24350,#24351,#24352,#24353,#24354,#24355,#24356,#24357,
#24358,#24359,#24360,#24361),(#24362,#24363,#24364,#24365,#24366,#24367,
#24368,#24369,#24370,#24371,#24372,#24373,#24374,#24375,#24376,#24377,#24378,
#24379,#24380,#24381,#24382,#24383,#24384,#24385,#24386,#24387,#24388,#24389,
#24390,#24391,#24392,#24393,#24394,#24395,#24396,#24397,#24398,#24399,#24400,
#24401,#24402,#24403,#24404,#24405,#24406,#24407,#24408,#24409,#24410),
(#24411,#24412,#24413,#24414,#24415,#24416,#24417,#24418,#24419,#24420,
#24421,#24422,#24423,#24424,#24425,#24426,#24427,#24428,#24429,#24430,#24431,
#24432,#24433,#24434,#24435,#24436,#24437,#24438,#24439,#24440,#24441,#24442,
#24443,#24444,#24445,#24446,#24447,#24448,#24449,#24450,#24451,#24452,#24453,
#24454,#24455,#24456,#24457,#24458,#24459),(#24460,#24461,#24462,#24463,
#24464,#24465,#24466,#24467,#24468,#24469,#24470,#24471,#24472,#24473,#24474,
#24475,#24476,#24477,#24478,#24479,#24480,#24481,#24482,#24483,#24484,#24485,
#24486,#24487,#24488,#24489,#24490,#24491,#24492,#24493,#24494,#24495,#24496,
#24497,#24498,#24499,#24500,#24501,#24502,#24503,#24504,#24505,#24506,#24507,
#24508),(#24509,#24510,#24511,#24512,#24513,#24514,#24515,#24516,#24517,
#24518,#24519,#24520,#24521,#24522,#24523,#24524,#24525,#24526,#24527,#24528,
#24529,#24530,#24531,#24532,#24533,#24534,#24535,#24536,#24537,#24538,#24539,
#24540,#24541,#24542,#24543,#24544,#24545,#24546,#24547,#24548,#24549,#24550,
#24551,#24552,#24553,#24554,#24555,#24556,#24557),(#24558,#24559,#24560,
#24561,#24562,#24563,#24564,#24565,#24566,#24567,#24568,#24569,#24570,#24571,
#24572,#24573,#24574,#24575,#24576,#24577,#24578,#24579,#24580,#24581,#24582,
#24583,#24584,#24585,#24586,#24587,#24588,#24589,#24590,#24591,#24592,#24593,
#24594,#24595,#24596,#24597,#24598,#24599,#24600,#24601,#24602,#24603,#24604,
#24605,#24606),(#24607,#24608,#24609,#24610,#24611,#24612,#24613,#24614,
#24615,#24616,#24617,#24618,#24619,#24620,#24621,#24622,#24623,#24624,#24625,
#24626,#24627,#24628,#24629,#24630,#24631,#24632,#24633,#24634,#24635,#24636,
#24637,#24638,#24639,#24640,#24641,#24642,#24643,#24644,#24645,#24646,#24647,
#24648,#24649,#24650,#24651,#24652,#24653,#24654,#24655),(#24656,#24657,
#24658,#24659,#24660,#24661,#24662,#24663,#24664,#24665,#24666,#24667,#24668,
#24669,#24670,#24671,#24672,#24673,#24674,#24675,#24676,#24677,#24678,#24679,
#24680,#24681,#24682,#24683,#24684,#24685,#24686,#24687,#24688,#24689,#24690,
#24691,#24692,#24693,#24694,#24695,#24696,#24697,#24698,#24699,#24700,#24701,
#24702,#24703,#24704),(#24705,#24706,#24707,#24708,#24709,#24710,#24711,
#24712,#24713,#24714,#24715,#24716,#24717,#24718,#24719,#24720,#24721,#24722,
#24723,#24724,#24725,#24726,#24727,#24728,#24729,#24730,#24731,#24732,#24733,
#24734,#24735,#24736,#24737,#24738,#24739,#24740,#24741,#24742,#24743,#24744,
#24745,#24746,#24747,#24748,#24749,#24750,#24751,#24752,#24753),(#24754,
#24755,#24756,#24757,#24758,#24759,#24760,#24761,#24762,#24763,#24764,#24765,
#24766,#24767,#24768,#24769,#24770,#24771,#24772,#24773,#24774,#24775,#24776,
#24777,#24778,#24779,#24780,#24781,#24782,#24783,#24784,#24785,#24786,#24787,
#24788,#24789,#24790,#24791,#24792,#24793,#24794,#24795,#24796,#24797,#24798,
#24799,#24800,#24801,#24802),(#24803,#24804,#24805,#24806,#24807,#24808,
#24809,#24810,#24811,#24812,#24813,#24814,#24815,#24816,#24817,#24818,#24819,
#24820,#24821,#24822,#24823,#24824,#24825,#24826,#24827,#24828,#24829,#24830,
#24831,#24832,#24833,#24834,#24835,#24836,#24837,#24838,#24839,#24840,#24841,
#24842,#24843,#24844,#24845,#24846,#24847,#24848,#24849,#24850,#24851),
(#24852,#24853,#24854,#24855,#24856,#24857,#24858,#24859,#24860,#24861,
#24862,#24863,#24864,#24865,#24866,#24867,#24868,#24869,#24870,#24871,#24872,
#24873,#24874,#24875,#24876,#24877,#24878,#24879,#24880,#24881,#24882,#24883,
#24884,#24885,#24886,#24887,#24888,#24889,#24890,#24891,#24892,#24893,#24894,
#24895,#24896,#24897,#24898,#24899,#24900),(#24901,#24902,#24903,#24904,
#24905,#24906,#24907,#24908,#24909,#24910,#24911,#24912,#24913,#24914,#24915,
#24916,#24917,#24918,#24919,#24920,#24921,#24922,#24923,#24924,#24925,#24926,
#24927,#24928,#24929,#24930,#24931,#24932,#24933,#24934,#24935,#24936,#24937,
#24938,#24939,#24940,#24941,#24942,#24943,#24944,#24945,#24946,#24947,#24948,
#24949),(#24950,#24951,#24952,#24953,#24954,#24955,#24956,#24957,#24958,
#24959,#24960,#24961,#24962,#24963,#24964,#24965,#24966,#24967,#24968,#24969,
#24970,#24971,#24972,#24973,#24974,#24975,#24976,#24977,#24978,#24979,#24980,
#24981,#24982,#24983,#24984,#24985,#24986,#24987,#24988,#24989,#24990,#24991,
#24992,#24993,#24994,#24995,#24996,#24997,#24998),(#24999,#25000,#25001,
#25002,#25003,#25004,#25005,#25006,#25007,#25008,#25009,#25010,#25011,#25012,
#25013,#25014,#25015,#25016,#25017,#25018,#25019,#25020,#25021,#25022,#25023,
#25024,#25025,#25026,#25027,#25028,#25029,#25030,#25031,#25032,#25033,#25034,
#25035,#25036,#25037,#25038,#25039,#25040,#25041,#25042,#25043,#25044,#25045,
#25046,#25047),(#25048,#25049,#25050,#25051,#25052,#25053,#25054,#25055,
#25056,#25057,#25058,#25059,#25060,#25061,#25062,#25063,#25064,#25065,#25066,
#25067,#25068,#25069,#25070,#25071,#25072,#25073,#25074,#25075,#25076,#25077,
#25078,#25079,#25080,#25081,#25082,#25083,#25084,#25085,#25086,#25087,#25088,
#25089,#25090,#25091,#25092,#25093,#25094,#25095,#25096),(#25097,#25098,
#25099,#25100,#25101,#25102,#25103,#25104,#25105,#25106,#25107,#25108,#25109,
#25110,#25111,#25112,#25113,#25114,#25115,#25116,#25117,#25118,#25119,#25120,
#25121,#25122,#25123,#25124,#25125,#25126,#25127,#25128,#25129,#25130,#25131,
#25132,#25133,#25134,#25135,#25136,#25137,#25138,#25139,#25140,#25141,#25142,
#25143,#25144,#25145),(#25146,#25147,#25148,#25149,#25150,#25151,#25152,
#25153,#25154,#25155,#25156,#25157,#25158,#25159,#25160,#25161,#25162,#25163,
#25164,#25165,#25166,#25167,#25168,#25169,#25170,#25171,#25172,#25173,#25174,
#25175,#25176,#25177,#25178,#25179,#25180,#25181,#25182,#25183,#25184,#25185,
#25186,#25187,#25188,#25189,#25190,#25191,#25192,#25193,#25194),(#25195,
#25196,#25197,#25198,#25199,#25200,#25201,#25202,#25203,#25204,#25205,#25206,
#25207,#25208,#25209,#25210,#25211,#25212,#25213,#25214,#25215,#25216,#25217,
#25218,#25219,#25220,#25221,#25222,#25223,#25224,#25225,#25226,#25227,#25228,
#25229,#25230,#25231,#25232,#25233,#25234,#25235,#25236,#25237,#25238,#25239,
#25240,#25241,#25242,#25243),(#25244,#25245,#25246,#25247,#25248,#25249,
#25250,#25251,#25252,#25253,#25254,#25255,#25256,#25257,#25258,#25259,#25260,
#25261,#25262,#25263,#25264,#25265,#25266,#25267,#25268,#25269,#25270,#25271,
#25272,#25273,#25274,#25275,#25276,#25277,#25278,#25279,#25280,#25281,#25282,
#25283,#25284,#25285,#25286,#25287,#25288,#25289,#25290,#25291,#25292),
(#25293,#25294,#25295,#25296,#25297,#25298,#25299,#25300,#25301,#25302,
#25303,#25304,#25305,#25306,#25307,#25308,#25309,#25310,#25311,#25312,#25313,
#25314,#25315,#25316,#25317,#25318,#25319,#25320,#25321,#25322,#25323,#25324,
#25325,#25326,#25327,#25328,#25329,#25330,#25331,#25332,#25333,#25334,#25335,
#25336,#25337,#25338,#25339,#25340,#25341),(#25342,#25343,#25344,#25345,
#25346,#25347,#25348,#25349,#25350,#25351,#25352,#25353,#25354,#25355,#25356,
#25357,#25358,#25359,#25360,#25361,#25362,#25363,#25364,#25365,#25366,#25367,
#25368,#25369,#25370,#25371,#25372,#25373,#25374,#25375,#25376,#25377,#25378,
#25379,#25380,#25381,#25382,#25383,#25384,#25385,#25386,#25387,#25388,#25389,
#25390),(#25391,#25392,#25393,#25394,#25395,#25396,#25397,#25398,#25399,
#25400,#25401,#25402,#25403,#25404,#25405,#25406,#25407,#25408,#25409,#25410,
#25411,#25412,#25413,#25414,#25415,#25416,#25417,#25418,#25419,#25420,#25421,
#25422,#25423,#25424,#25425,#25426,#25427,#25428,#25429,#25430,#25431,#25432,
#25433,#25434,#25435,#25436,#25437,#25438,#25439),(#25440,#25441,#25442,
#25443,#25444,#25445,#25446,#25447,#25448,#25449,#25450,#25451,#25452,#25453,
#25454,#25455,#25456,#25457,#25458,#25459,#25460,#25461,#25462,#25463,#25464,
#25465,#25466,#25467,#25468,#25469,#25470,#25471,#25472,#25473,#25474,#25475,
#25476,#25477,#25478,#25479,#25480,#25481,#25482,#25483,#25484,#25485,#25486,
#25487,#25488),(#25489,#25490,#25491,#25492,#25493,#25494,#25495,#25496,
#25497,#25498,#25499,#25500,#25501,#25502,#25503,#25504,#25505,#25506,#25507,
#25508,#25509,#25510,#25511,#25512,#25513,#25514,#25515,#25516,#25517,#25518,
#25519,#25520,#25521,#25522,#25523,#25524,#25525,#25526,#25527,#25528,#25529,
#25530,#25531,#25532,#25533,#25534,#25535,#25536,#25537),(#25538,#25539,
#25540,#25541,#25542,#25543,#25544,#25545,#25546,#25547,#25548,#25549,#25550,
#25551,#25552,#25553,#25554,#25555,#25556,#25557,#25558,#25559,#25560,#25561,
#25562,#25563,#25564,#25565,#25566,#25567,#25568,#25569,#25570,#25571,#25572,
#25573,#25574,#25575,#25576,#25577,#25578,#25579,#25580,#25581,#25582,#25583,
#25584,#25585,#25586),(#25587,#25588,#25589,#25590,#25591,#25592,#25593,
#25594,#25595,#25596,#25597,#25598,#25599,#25600,#25601,#25602,#25603,#25604,
#25605,#25606,#25607,#25608,#25609,#25610,#25611,#25612,#25613,#25614,#25615,
#25616,#25617,#25618,#25619,#25620,#25621,#25622,#25623,#25624,#25625,#25626,
#25627,#25628,#25629,#25630,#25631,#25632,#25633,#25634,#25635),(#25636,
#25637,#25638,#25639,#25640,#25641,#25642,#25643,#25644,#25645,#25646,#25647,
#25648,#25649,#25650,#25651,#25652,#25653,#25654,#25655,#25656,#25657,#25658,
#25659,#25660,#25661,#25662,#25663,#25664,#25665,#25666,#25667,#25668,#25669,
#25670,#25671,#25672,#25673,#25674,#25675,#25676,#25677,#25678,#25679,#25680,
#25681,#25682,#25683,#25684),(#25685,#25686,#25687,#25688,#25689,#25690,
#25691,#25692,#25693,#25694,#25695,#25696,#25697,#25698,#25699,#25700,#25701,
#25702,#25703,#25704,#25705,#25706,#25707,#25708,#25709,#25710,#25711,#25712,
#25713,#25714,#25715,#25716,#25717,#25718,#25719,#25720,#25721,#25722,#25723,
#25724,#25725,#25726,#25727,#25728,#25729,#25730,#25731,#25732,#25733),
(#25734,#25735,#25736,#25737,#25738,#25739,#25740,#25741,#25742,#25743,
#25744,#25745,#25746,#25747,#25748,#25749,#25750,#25751,#25752,#25753,#25754,
#25755,#25756,#25757,#25758,#25759,#25760,#25761,#25762,#25763,#25764,#25765,
#25766,#25767,#25768,#25769,#25770,#25771,#25772,#25773,#25774,#25775,#25776,
#25777,#25778,#25779,#25780,#25781,#25782),(#25783,#25784,#25785,#25786,
#25787,#25788,#25789,#25790,#25791,#25792,#25793,#25794,#25795,#25796,#25797,
#25798,#25799,#25800,#25801,#25802,#25803,#25804,#25805,#25806,#25807,#25808,
#25809,#25810,#25811,#25812,#25813,#25814,#25815,#25816,#25817,#25818,#25819,
#25820,#25821,#25822,#25823,#25824,#25825,#25826,#25827,#25828,#25829,#25830,
#25831),(#25832,#25833,#25834,#25835,#25836,#25837,#25838,#25839,#25840,
#25841,#25842,#25843,#25844,#25845,#25846,#25847,#25848,#25849,#25850,#25851,
#25852,#25853,#25854,#25855,#25856,#25857,#25858,#25859,#25860,#25861,#25862,
#25863,#25864,#25865,#25866,#25867,#25868,#25869,#25870,#25871,#25872,#25873,
#25874,#25875,#25876,#25877,#25878,#25879,#25880),(#25881,#25882,#25883,
#25884,#25885,#25886,#25887,#25888,#25889,#25890,#25891,#25892,#25893,#25894,
#25895,#25896,#25897,#25898,#25899,#25900,#25901,#25902,#25903,#25904,#25905,
#25906,#25907,#25908,#25909,#25910,#25911,#25912,#25913,#25914,#25915,#25916,
#25917,#25918,#25919,#25920,#25921,#25922,#25923,#25924,#25925,#25926,#25927,
#25928,#25929),(#25930,#25931,#25932,#25933,#25934,#25935,#25936,#25937,
#25938,#25939,#25940,#25941,#25942,#25943,#25944,#25945,#25946,#25947,#25948,
#25949,#25950,#25951,#25952,#25953,#25954,#25955,#25956,#25957,#25958,#25959,
#25960,#25961,#25962,#25963,#25964,#25965,#25966,#25967,#25968,#25969,#25970,
#25971,#25972,#25973,#25974,#25975,#25976,#25977,#25978),(#25979,#25980,
#25981,#25982,#25983,#25984,#25985,#25986,#25987,#25988,#25989,#25990,#25991,
#25992,#25993,#25994,#25995,#25996,#25997,#25998,#25999,#26000,#26001,#26002,
#26003,#26004,#26005,#26006,#26007,#26008,#26009,#26010,#26011,#26012,#26013,
#26014,#26015,#26016,#26017,#26018,#26019,#26020,#26021,#26022,#26023,#26024,
#26025,#26026,#26027),(#26028,#26029,#26030,#26031,#26032,#26033,#26034,
#26035,#26036,#26037,#26038,#26039,#26040,#26041,#26042,#26043,#26044,#26045,
#26046,#26047,#26048,#26049,#26050,#26051,#26052,#26053,#26054,#26055,#26056,
#26057,#26058,#26059,#26060,#26061,#26062,#26063,#26064,#26065,#26066,#26067,
#26068,#26069,#26070,#26071,#26072,#26073,#26074,#26075,#26076),(#26077,
#26078,#26079,#26080,#26081,#26082,#26083,#26084,#26085,#26086,#26087,#26088,
#26089,#26090,#26091,#26092,#26093,#26094,#26095,#26096,#26097,#26098,#26099,
#26100,#26101,#26102,#26103,#26104,#26105,#26106,#26107,#26108,#26109,#26110,
#26111,#26112,#26113,#26114,#26115,#26116,#26117,#26118,#26119,#26120,#26121,
#26122,#26123,#26124,#26125),(#26126,#26127,#26128,#26129,#26130,#26131,
#26132,#26133,#26134,#26135,#26136,#26137,#26138,#26139,#26140,#26141,#26142,
#26143,#26144,#26145,#26146,#26147,#26148,#26149,#26150,#26151,#26152,#26153,
#26154,#26155,#26156,#26157,#26158,#26159,#26160,#26161,#26162,#26163,#26164,
#26165,#26166,#26167,#26168,#26169,#26170,#26171,#26172,#26173,#26174),
(#26175,#26176,#26177,#26178,#26179,#26180,#26181,#26182,#26183,#26184,
#26185,#26186,#26187,#26188,#26189,#26190,#26191,#26192,#26193,#26194,#26195,
#26196,#26197,#26198,#26199,#26200,#26201,#26202,#26203,#26204,#26205,#26206,
#26207,#26208,#26209,#26210,#26211,#26212,#26213,#26214,#26215,#26216,#26217,
#26218,#26219,#26220,#26221,#26222,#26223),(#26224,#26225,#26226,#26227,
#26228,#26229,#26230,#26231,#26232,#26233,#26234,#26235,#26236,#26237,#26238,
#26239,#26240,#26241,#26242,#26243,#26244,#26245,#26246,#26247,#26248,#26249,
#26250,#26251,#26252,#26253,#26254,#26255,#26256,#26257,#26258,#26259,#26260,
#26261,#26262,#26263,#26264,#26265,#26266,#26267,#26268,#26269,#26270,#26271,
#26272),(#26273,#26274,#26275,#26276,#26277,#26278,#26279,#26280,#26281,
#26282,#26283,#26284,#26285,#26286,#26287,#26288,#26289,#26290,#26291,#26292,
#26293,#26294,#26295,#26296,#26297,#26298,#26299,#26300,#26301,#26302,#26303,
#26304,#26305,#26306,#26307,#26308,#26309,#26310,#26311,#26312,#26313,#26314,
#26315,#26316,#26317,#26318,#26319,#26320,#26321),(#26322,#26323,#26324,
#26325,#26326,#26327,#26328,#26329,#26330,#26331,#26332,#26333,#26334,#26335,
#26336,#26337,#26338,#26339,#26340,#26341,#26342,#26343,#26344,#26345,#26346,
#26347,#26348,#26349,#26350,#26351,#26352,#26353,#26354,#26355,#26356,#26357,
#26358,#26359,#26360,#26361,#26362,#26363,#26364,#26365,#26366,#26367,#26368,
#26369,#26370),(#26371,#26372,#26373,#26374,#26375,#26376,#26377,#26378,
#26379,#26380,#26381,#26382,#26383,#26384,#26385,#26386,#26387,#26388,#26389,
#26390,#26391,#26392,#26393,#26394,#26395,#26396,#26397,#26398,#26399,#26400,
#26401,#26402,#26403,#26404,#26405,#26406,#26407,#26408,#26409,#26410,#26411,
#26412,#26413,#26414,#26415,#26416,#26417,#26418,#26419),(#26420,#26421,
#26422,#26423,#26424,#26425,#26426,#26427,#26428,#26429,#26430,#26431,#26432,
#26433,#26434,#26435,#26436,#26437,#26438,#26439,#26440,#26441,#26442,#26443,
#26444,#26445,#26446,#26447,#26448,#26449,#26450,#26451,#26452,#26453,#26454,
#26455,#26456,#26457,#26458,#26459,#26460,#26461,#26462,#26463,#26464,#26465,
#26466,#26467,#26468),(#26469,#26470,#26471,#26472,#26473,#26474,#26475,
#26476,#26477,#26478,#26479,#26480,#26481,#26482,#26483,#26484,#26485,#26486,
#26487,#26488,#26489,#26490,#26491,#26492,#26493,#26494,#26495,#26496,#26497,
#26498,#26499,#26500,#26501,#26502,#26503,#26504,#26505,#26506,#26507,#26508,
#26509,#26510,#26511,#26512,#26513,#26514,#26515,#26516,#26517),(#26518,
#26519,#26520,#26521,#26522,#26523,#26524,#26525,#26526,#26527,#26528,#26529,
#26530,#26531,#26532,#26533,#26534,#26535,#26536,#26537,#26538,#26539,#26540,
#26541,#26542,#26543,#26544,#26545,#26546,#26547,#26548,#26549,#26550,#26551,
#26552,#26553,#26554,#26555,#26556,#26557,#26558,#26559,#26560,#26561,#26562,
#26563,#26564,#26565,#26566),(#26567,#26568,#26569,#26570,#26571,#26572,
#26573,#26574,#26575,#26576,#26577,#26578,#26579,#26580,#26581,#26582,#26583,
#26584,#26585,#26586,#26587,#26588,#26589,#26590,#26591,#26592,#26593,#26594,
#26595,#26596,#26597,#26598,#26599,#26600,#26601,#26602,#26603,#26604,#26605,
#26606,#26607,#26608,#26609,#26610,#26611,#26612,#26613,#26614,#26615),
(#26616,#26617,#26618,#26619,#26620,#26621,#26622,#26623,#26624,#26625,
#26626,#26627,#26628,#26629,#26630,#26631,#26632,#26633,#26634,#26635,#26636,
#26637,#26638,#26639,#26640,#26641,#26642,#26643,#26644,#26645,#26646,#26647,
#26648,#26649,#26650,#26651,#26652,#26653,#26654,#26655,#26656,#26657,#26658,
#26659,#26660,#26661,#26662,#26663,#26664),(#26665,#26666,#26667,#26668,
#26669,#26670,#26671,#26672,#26673,#26674,#26675,#26676,#26677,#26678,#26679,
#26680,#26681,#26682,#26683,#26684,#26685,#26686,#26687,#26688,#26689,#26690,
#26691,#26692,#26693,#26694,#26695,#26696,#26697,#26698,#26699,#26700,#26701,
#26702,#26703,#26704,#26705,#26706,#26707,#26708,#26709,#26710,#26711,#26712,
#26713),(#26714,#26715,#26716,#26717,#26718,#26719,#26720,#26721,#26722,
#26723,#26724,#26725,#26726,#26727,#26728,#26729,#26730,#26731,#26732,#26733,
#26734,#26735,#26736,#26737,#26738,#26739,#26740,#26741,#26742,#26743,#26744,
#26745,#26746,#26747,#26748,#26749,#26750,#26751,#26752,#26753,#26754,#26755,
#26756,#26757,#26758,#26759,#26760,#26761,#26762),(#26763,#26764,#26765,
#26766,#26767,#26768,#26769,#26770,#26771,#26772,#26773,#26774,#26775,#26776,
#26777,#26778,#26779,#26780,#26781,#26782,#26783,#26784,#26785,#26786,#26787,
#26788,#26789,#26790,#26791,#26792,#26793,#26794,#26795,#26796,#26797,#26798,
#26799,#26800,#26801,#26802,#26803,#26804,#26805,#26806,#26807,#26808,#26809,
#26810,#26811),(#26812,#26813,#26814,#26815,#26816,#26817,#26818,#26819,
#26820,#26821,#26822,#26823,#26824,#26825,#26826,#26827,#26828,#26829,#26830,
#26831,#26832,#26833,#26834,#26835,#26836,#26837,#26838,#26839,#26840,#26841,
#26842,#26843,#26844,#26845,#26846,#26847,#26848,#26849,#26850,#26851,#26852,
#26853,#26854,#26855,#26856,#26857,#26858,#26859,#26860),(#26861,#26862,
#26863,#26864,#26865,#26866,#26867,#26868,#26869,#26870,#26871,#26872,#26873,
#26874,#26875,#26876,#26877,#26878,#26879,#26880,#26881,#26882,#26883,#26884,
#26885,#26886,#26887,#26888,#26889,#26890,#26891,#26892,#26893,#26894,#26895,
#26896,#26897,#26898,#26899,#26900,#26901,#26902,#26903,#26904,#26905,#26906,
#26907,#26908,#26909),(#26910,#26911,#26912,#26913,#26914,#26915,#26916,
#26917,#26918,#26919,#26920,#26921,#26922,#26923,#26924,#26925,#26926,#26927,
#26928,#26929,#26930,#26931,#26932,#26933,#26934,#26935,#26936,#26937,#26938,
#26939,#26940,#26941,#26942,#26943,#26944,#26945,#26946,#26947,#26948,#26949,
#26950,#26951,#26952,#26953,#26954,#26955,#26956,#26957,#26958),(#26959,
#26960,#26961,#26962,#26963,#26964,#26965,#26966,#26967,#26968,#26969,#26970,
#26971,#26972,#26973,#26974,#26975,#26976,#26977,#26978,#26979,#26980,#26981,
#26982,#26983,#26984,#26985,#26986,#26987,#26988,#26989,#26990,#26991,#26992,
#26993,#26994,#26995,#26996,#26997,#26998,#26999,#27000,#27001,#27002,#27003,
#27004,#27005,#27006,#27007),(#27008,#27009,#27010,#27011,#27012,#27013,
#27014,#27015,#27016,#27017,#27018,#27019,#27020,#27021,#27022,#27023,#27024,
#27025,#27026,#27027,#27028,#27029,#27030,#27031,#27032,#27033,#27034,#27035,
#27036,#27037,#27038,#27039,#27040,#27041,#27042,#27043,#27044,#27045,#27046,
#27047,#27048,#27049,#27050,#27051,#27052,#27053,#27054,#27055,#27056),
(#27057,#27058,#27059,#27060,#27061,#27062,#27063,#27064,#27065,#27066,
#27067,#27068,#27069,#27070,#27071,#27072,#27073,#27074,#27075,#27076,#27077,
#27078,#27079,#27080,#27081,#27082,#27083,#27084,#27085,#27086,#27087,#27088,
#27089,#27090,#27091,#27092,#27093,#27094,#27095,#27096,#27097,#27098,#27099,
#27100,#27101,#27102,#27103,#27104,#27105),(#27106,#27107,#27108,#27109,
#27110,#27111,#27112,#27113,#27114,#27115,#27116,#27117,#27118,#27119,#27120,
#27121,#27122,#27123,#27124,#27125,#27126,#27127,#27128,#27129,#27130,#27131,
#27132,#27133,#27134,#27135,#27136,#27137,#27138,#27139,#27140,#27141,#27142,
#27143,#27144,#27145,#27146,#27147,#27148,#27149,#27150,#27151,#27152,#27153,
#27154),(#27155,#27156,#27157,#27158,#27159,#27160,#27161,#27162,#27163,
#27164,#27165,#27166,#27167,#27168,#27169,#27170,#27171,#27172,#27173,#27174,
#27175,#27176,#27177,#27178,#27179,#27180,#27181,#27182,#27183,#27184,#27185,
#27186,#27187,#27188,#27189,#27190,#27191,#27192,#27193,#27194,#27195,#27196,
#27197,#27198,#27199,#27200,#27201,#27202,#27203),(#27204,#27205,#27206,
#27207,#27208,#27209,#27210,#27211,#27212,#27213,#27214,#27215,#27216,#27217,
#27218,#27219,#27220,#27221,#27222,#27223,#27224,#27225,#27226,#27227,#27228,
#27229,#27230,#27231,#27232,#27233,#27234,#27235,#27236,#27237,#27238,#27239,
#27240,#27241,#27242,#27243,#27244,#27245,#27246,#27247,#27248,#27249,#27250,
#27251,#27252),(#27253,#27254,#27255,#27256,#27257,#27258,#27259,#27260,
#27261,#27262,#27263,#27264,#27265,#27266,#27267,#27268,#27269,#27270,#27271,
#27272,#27273,#27274,#27275,#27276,#27277,#27278,#27279,#27280,#27281,#27282,
#27283,#27284,#27285,#27286,#27287,#27288,#27289,#27290,#27291,#27292,#27293,
#27294,#27295,#27296,#27297,#27298,#27299,#27300,#27301),(#27302,#27303,
#27304,#27305,#27306,#27307,#27308,#27309,#27310,#27311,#27312,#27313,#27314,
#27315,#27316,#27317,#27318,#27319,#27320,#27321,#27322,#27323,#27324,#27325,
#27326,#27327,#27328,#27329,#27330,#27331,#27332,#27333,#27334,#27335,#27336,
#27337,#27338,#27339,#27340,#27341,#27342,#27343,#27344,#27345,#27346,#27347,
#27348,#27349,#27350),(#27351,#27352,#27353,#27354,#27355,#27356,#27357,
#27358,#27359,#27360,#27361,#27362,#27363,#27364,#27365,#27366,#27367,#27368,
#27369,#27370,#27371,#27372,#27373,#27374,#27375,#27376,#27377,#27378,#27379,
#27380,#27381,#27382,#27383,#27384,#27385,#27386,#27387,#27388,#27389,#27390,
#27391,#27392,#27393,#27394,#27395,#27396,#27397,#27398,#27399),(#27400,
#27401,#27402,#27403,#27404,#27405,#27406,#27407,#27408,#27409,#27410,#27411,
#27412,#27413,#27414,#27415,#27416,#27417,#27418,#27419,#27420,#27421,#27422,
#27423,#27424,#27425,#27426,#27427,#27428,#27429,#27430,#27431,#27432,#27433,
#27434,#27435,#27436,#27437,#27438,#27439,#27440,#27441,#27442,#27443,#27444,
#27445,#27446,#27447,#27448),(#27449,#27450,#27451,#27452,#27453,#27454,
#27455,#27456,#27457,#27458,#27459,#27460,#27461,#27462,#27463,#27464,#27465,
#27466,#27467,#27468,#27469,#27470,#27471,#27472,#27473,#27474,#27475,#27476,
#27477,#27478,#27479,#27480,#27481,#27482,#27483,#27484,#27485,#27486,#27487,
#27488,#27489,#27490,#27491,#27492,#27493,#27494,#27495,#27496,#27497),
(#27498,#27499,#27500,#27501,#27502,#27503,#27504,#27505,#27506,#27507,
#27508,#27509,#27510,#27511,#27512,#27513,#27514,#27515,#27516,#27517,#27518,
#27519,#27520,#27521,#27522,#27523,#27524,#27525,#27526,#27527,#27528,#27529,
#27530,#27531,#27532,#27533,#27534,#27535,#27536,#27537,#27538,#27539,#27540,
#27541,#27542,#27543,#27544,#27545,#27546),(#27547,#27548,#27549,#27550,
#27551,#27552,#27553,#27554,#27555,#27556,#27557,#27558,#27559,#27560,#27561,
#27562,#27563,#27564,#27565,#27566,#27567,#27568,#27569,#27570,#27571,#27572,
#27573,#27574,#27575,#27576,#27577,#27578,#27579,#27580,#27581,#27582,#27583,
#27584,#27585,#27586,#27587,#27588,#27589,#27590,#27591,#27592,#27593,#27594,
#27595),(#27596,#27597,#27598,#27599,#27600,#27601,#27602,#27603,#27604,
#27605,#27606,#27607,#27608,#27609,#27610,#27611,#27612,#27613,#27614,#27615,
#27616,#27617,#27618,#27619,#27620,#27621,#27622,#27623,#27624,#27625,#27626,
#27627,#27628,#27629,#27630,#27631,#27632,#27633,#27634,#27635,#27636,#27637,
#27638,#27639,#27640,#27641,#27642,#27643,#27644)),.UNSPECIFIED.,.F.,.F.,
 .F.,(4,3,3,3,3,3,3,3,3,3,3,3,3,3,3,3,3,3,3,3,3,3,3,3,3,3,3,3,3,3,3,3,3,
3,3,3,3,3,3,3,4),(4,3,3,3,3,3,3,3,3,3,3,3,3,3,3,3,4),(-1.41424042909535E-5,
-3.89974880004448E-6,-1.33908492731722E-6,-5.87529909535886E-8,1.22157894541004E-6,
6.34290669086456E-6,2.68282176726826E-5,4.73135286545007E-5,6.77988396363188E-5,
8.82841506181369E-5,0.000108769461599955,0.000129254772581773,0.000149740083563591,
0.000190710705527227,0.000231681327490863,0.0002726519494545,0.000313622571418136,
0.000354593193381772,0.000395563815345408,0.00047750505927268,0.000559446303199953,
0.000641387547127225,0.000723328791054497,0.00080527003498177,0.000887211278909042,
0.000969152522836314,0.00113303501069086,0.0012969174985454,0.00146079998639995,
0.00162468247425449,0.00178856496210904,0.00195244744996358,0.00228021242567267,
0.00260797740138176,0.00293574237709085,0.00326350735279994,0.00359127232850903,
0.00391903730421812,0.00424680227992721,0.0045745672556363,0.00528564362815289),
(-5.55464210984207E-5,0.0625,0.125,0.1875,0.25,0.3125,0.375,0.4375,0.5,
0.5625,0.625,0.6875,0.75,0.8125,0.875,0.9375,1.),.UNSPECIFIED.);
#193=B_SPLINE_SURFACE_WITH_KNOTS('',3,3,((#27792,#27793,#27794,#27795,#27796,
#27797,#27798,#27799,#27800,#27801,#27802,#27803,#27804,#27805,#27806,#27807,
#27808,#27809,#27810,#27811,#27812,#27813,#27814,#27815,#27816,#27817,#27818,
#27819,#27820,#27821,#27822,#27823,#27824,#27825,#27826,#27827,#27828,#27829,
#27830,#27831,#27832,#27833,#27834,#27835,#27836,#27837,#27838,#27839,#27840),
(#27841,#27842,#27843,#27844,#27845,#27846,#27847,#27848,#27849,#27850,
#27851,#27852,#27853,#27854,#27855,#27856,#27857,#27858,#27859,#27860,#27861,
#27862,#27863,#27864,#27865,#27866,#27867,#27868,#27869,#27870,#27871,#27872,
#27873,#27874,#27875,#27876,#27877,#27878,#27879,#27880,#27881,#27882,#27883,
#27884,#27885,#27886,#27887,#27888,#27889),(#27890,#27891,#27892,#27893,
#27894,#27895,#27896,#27897,#27898,#27899,#27900,#27901,#27902,#27903,#27904,
#27905,#27906,#27907,#27908,#27909,#27910,#27911,#27912,#27913,#27914,#27915,
#27916,#27917,#27918,#27919,#27920,#27921,#27922,#27923,#27924,#27925,#27926,
#27927,#27928,#27929,#27930,#27931,#27932,#27933,#27934,#27935,#27936,#27937,
#27938),(#27939,#27940,#27941,#27942,#27943,#27944,#27945,#27946,#27947,
#27948,#27949,#27950,#27951,#27952,#27953,#27954,#27955,#27956,#27957,#27958,
#27959,#27960,#27961,#27962,#27963,#27964,#27965,#27966,#27967,#27968,#27969,
#27970,#27971,#27972,#27973,#27974,#27975,#27976,#27977,#27978,#27979,#27980,
#27981,#27982,#27983,#27984,#27985,#27986,#27987),(#27988,#27989,#27990,
#27991,#27992,#27993,#27994,#27995,#27996,#27997,#27998,#27999,#28000,#28001,
#28002,#28003,#28004,#28005,#28006,#28007,#28008,#28009,#28010,#28011,#28012,
#28013,#28014,#28015,#28016,#28017,#28018,#28019,#28020,#28021,#28022,#28023,
#28024,#28025,#28026,#28027,#28028,#28029,#28030,#28031,#28032,#28033,#28034,
#28035,#28036),(#28037,#28038,#28039,#28040,#28041,#28042,#28043,#28044,
#28045,#28046,#28047,#28048,#28049,#28050,#28051,#28052,#28053,#28054,#28055,
#28056,#28057,#28058,#28059,#28060,#28061,#28062,#28063,#28064,#28065,#28066,
#28067,#28068,#28069,#28070,#28071,#28072,#28073,#28074,#28075,#28076,#28077,
#28078,#28079,#28080,#28081,#28082,#28083,#28084,#28085),(#28086,#28087,
#28088,#28089,#28090,#28091,#28092,#28093,#28094,#28095,#28096,#28097,#28098,
#28099,#28100,#28101,#28102,#28103,#28104,#28105,#28106,#28107,#28108,#28109,
#28110,#28111,#28112,#28113,#28114,#28115,#28116,#28117,#28118,#28119,#28120,
#28121,#28122,#28123,#28124,#28125,#28126,#28127,#28128,#28129,#28130,#28131,
#28132,#28133,#28134),(#28135,#28136,#28137,#28138,#28139,#28140,#28141,
#28142,#28143,#28144,#28145,#28146,#28147,#28148,#28149,#28150,#28151,#28152,
#28153,#28154,#28155,#28156,#28157,#28158,#28159,#28160,#28161,#28162,#28163,
#28164,#28165,#28166,#28167,#28168,#28169,#28170,#28171,#28172,#28173,#28174,
#28175,#28176,#28177,#28178,#28179,#28180,#28181,#28182,#28183),(#28184,
#28185,#28186,#28187,#28188,#28189,#28190,#28191,#28192,#28193,#28194,#28195,
#28196,#28197,#28198,#28199,#28200,#28201,#28202,#28203,#28204,#28205,#28206,
#28207,#28208,#28209,#28210,#28211,#28212,#28213,#28214,#28215,#28216,#28217,
#28218,#28219,#28220,#28221,#28222,#28223,#28224,#28225,#28226,#28227,#28228,
#28229,#28230,#28231,#28232),(#28233,#28234,#28235,#28236,#28237,#28238,
#28239,#28240,#28241,#28242,#28243,#28244,#28245,#28246,#28247,#28248,#28249,
#28250,#28251,#28252,#28253,#28254,#28255,#28256,#28257,#28258,#28259,#28260,
#28261,#28262,#28263,#28264,#28265,#28266,#28267,#28268,#28269,#28270,#28271,
#28272,#28273,#28274,#28275,#28276,#28277,#28278,#28279,#28280,#28281),
(#28282,#28283,#28284,#28285,#28286,#28287,#28288,#28289,#28290,#28291,
#28292,#28293,#28294,#28295,#28296,#28297,#28298,#28299,#28300,#28301,#28302,
#28303,#28304,#28305,#28306,#28307,#28308,#28309,#28310,#28311,#28312,#28313,
#28314,#28315,#28316,#28317,#28318,#28319,#28320,#28321,#28322,#28323,#28324,
#28325,#28326,#28327,#28328,#28329,#28330),(#28331,#28332,#28333,#28334,
#28335,#28336,#28337,#28338,#28339,#28340,#28341,#28342,#28343,#28344,#28345,
#28346,#28347,#28348,#28349,#28350,#28351,#28352,#28353,#28354,#28355,#28356,
#28357,#28358,#28359,#28360,#28361,#28362,#28363,#28364,#28365,#28366,#28367,
#28368,#28369,#28370,#28371,#28372,#28373,#28374,#28375,#28376,#28377,#28378,
#28379),(#28380,#28381,#28382,#28383,#28384,#28385,#28386,#28387,#28388,
#28389,#28390,#28391,#28392,#28393,#28394,#28395,#28396,#28397,#28398,#28399,
#28400,#28401,#28402,#28403,#28404,#28405,#28406,#28407,#28408,#28409,#28410,
#28411,#28412,#28413,#28414,#28415,#28416,#28417,#28418,#28419,#28420,#28421,
#28422,#28423,#28424,#28425,#28426,#28427,#28428),(#28429,#28430,#28431,
#28432,#28433,#28434,#28435,#28436,#28437,#28438,#28439,#28440,#28441,#28442,
#28443,#28444,#28445,#28446,#28447,#28448,#28449,#28450,#28451,#28452,#28453,
#28454,#28455,#28456,#28457,#28458,#28459,#28460,#28461,#28462,#28463,#28464,
#28465,#28466,#28467,#28468,#28469,#28470,#28471,#28472,#28473,#28474,#28475,
#28476,#28477),(#28478,#28479,#28480,#28481,#28482,#28483,#28484,#28485,
#28486,#28487,#28488,#28489,#28490,#28491,#28492,#28493,#28494,#28495,#28496,
#28497,#28498,#28499,#28500,#28501,#28502,#28503,#28504,#28505,#28506,#28507,
#28508,#28509,#28510,#28511,#28512,#28513,#28514,#28515,#28516,#28517,#28518,
#28519,#28520,#28521,#28522,#28523,#28524,#28525,#28526),(#28527,#28528,
#28529,#28530,#28531,#28532,#28533,#28534,#28535,#28536,#28537,#28538,#28539,
#28540,#28541,#28542,#28543,#28544,#28545,#28546,#28547,#28548,#28549,#28550,
#28551,#28552,#28553,#28554,#28555,#28556,#28557,#28558,#28559,#28560,#28561,
#28562,#28563,#28564,#28565,#28566,#28567,#28568,#28569,#28570,#28571,#28572,
#28573,#28574,#28575),(#28576,#28577,#28578,#28579,#28580,#28581,#28582,
#28583,#28584,#28585,#28586,#28587,#28588,#28589,#28590,#28591,#28592,#28593,
#28594,#28595,#28596,#28597,#28598,#28599,#28600,#28601,#28602,#28603,#28604,
#28605,#28606,#28607,#28608,#28609,#28610,#28611,#28612,#28613,#28614,#28615,
#28616,#28617,#28618,#28619,#28620,#28621,#28622,#28623,#28624),(#28625,
#28626,#28627,#28628,#28629,#28630,#28631,#28632,#28633,#28634,#28635,#28636,
#28637,#28638,#28639,#28640,#28641,#28642,#28643,#28644,#28645,#28646,#28647,
#28648,#28649,#28650,#28651,#28652,#28653,#28654,#28655,#28656,#28657,#28658,
#28659,#28660,#28661,#28662,#28663,#28664,#28665,#28666,#28667,#28668,#28669,
#28670,#28671,#28672,#28673),(#28674,#28675,#28676,#28677,#28678,#28679,
#28680,#28681,#28682,#28683,#28684,#28685,#28686,#28687,#28688,#28689,#28690,
#28691,#28692,#28693,#28694,#28695,#28696,#28697,#28698,#28699,#28700,#28701,
#28702,#28703,#28704,#28705,#28706,#28707,#28708,#28709,#28710,#28711,#28712,
#28713,#28714,#28715,#28716,#28717,#28718,#28719,#28720,#28721,#28722),
(#28723,#28724,#28725,#28726,#28727,#28728,#28729,#28730,#28731,#28732,
#28733,#28734,#28735,#28736,#28737,#28738,#28739,#28740,#28741,#28742,#28743,
#28744,#28745,#28746,#28747,#28748,#28749,#28750,#28751,#28752,#28753,#28754,
#28755,#28756,#28757,#28758,#28759,#28760,#28761,#28762,#28763,#28764,#28765,
#28766,#28767,#28768,#28769,#28770,#28771),(#28772,#28773,#28774,#28775,
#28776,#28777,#28778,#28779,#28780,#28781,#28782,#28783,#28784,#28785,#28786,
#28787,#28788,#28789,#28790,#28791,#28792,#28793,#28794,#28795,#28796,#28797,
#28798,#28799,#28800,#28801,#28802,#28803,#28804,#28805,#28806,#28807,#28808,
#28809,#28810,#28811,#28812,#28813,#28814,#28815,#28816,#28817,#28818,#28819,
#28820),(#28821,#28822,#28823,#28824,#28825,#28826,#28827,#28828,#28829,
#28830,#28831,#28832,#28833,#28834,#28835,#28836,#28837,#28838,#28839,#28840,
#28841,#28842,#28843,#28844,#28845,#28846,#28847,#28848,#28849,#28850,#28851,
#28852,#28853,#28854,#28855,#28856,#28857,#28858,#28859,#28860,#28861,#28862,
#28863,#28864,#28865,#28866,#28867,#28868,#28869),(#28870,#28871,#28872,
#28873,#28874,#28875,#28876,#28877,#28878,#28879,#28880,#28881,#28882,#28883,
#28884,#28885,#28886,#28887,#28888,#28889,#28890,#28891,#28892,#28893,#28894,
#28895,#28896,#28897,#28898,#28899,#28900,#28901,#28902,#28903,#28904,#28905,
#28906,#28907,#28908,#28909,#28910,#28911,#28912,#28913,#28914,#28915,#28916,
#28917,#28918),(#28919,#28920,#28921,#28922,#28923,#28924,#28925,#28926,
#28927,#28928,#28929,#28930,#28931,#28932,#28933,#28934,#28935,#28936,#28937,
#28938,#28939,#28940,#28941,#28942,#28943,#28944,#28945,#28946,#28947,#28948,
#28949,#28950,#28951,#28952,#28953,#28954,#28955,#28956,#28957,#28958,#28959,
#28960,#28961,#28962,#28963,#28964,#28965,#28966,#28967),(#28968,#28969,
#28970,#28971,#28972,#28973,#28974,#28975,#28976,#28977,#28978,#28979,#28980,
#28981,#28982,#28983,#28984,#28985,#28986,#28987,#28988,#28989,#28990,#28991,
#28992,#28993,#28994,#28995,#28996,#28997,#28998,#28999,#29000,#29001,#29002,
#29003,#29004,#29005,#29006,#29007,#29008,#29009,#29010,#29011,#29012,#29013,
#29014,#29015,#29016),(#29017,#29018,#29019,#29020,#29021,#29022,#29023,
#29024,#29025,#29026,#29027,#29028,#29029,#29030,#29031,#29032,#29033,#29034,
#29035,#29036,#29037,#29038,#29039,#29040,#29041,#29042,#29043,#29044,#29045,
#29046,#29047,#29048,#29049,#29050,#29051,#29052,#29053,#29054,#29055,#29056,
#29057,#29058,#29059,#29060,#29061,#29062,#29063,#29064,#29065),(#29066,
#29067,#29068,#29069,#29070,#29071,#29072,#29073,#29074,#29075,#29076,#29077,
#29078,#29079,#29080,#29081,#29082,#29083,#29084,#29085,#29086,#29087,#29088,
#29089,#29090,#29091,#29092,#29093,#29094,#29095,#29096,#29097,#29098,#29099,
#29100,#29101,#29102,#29103,#29104,#29105,#29106,#29107,#29108,#29109,#29110,
#29111,#29112,#29113,#29114),(#29115,#29116,#29117,#29118,#29119,#29120,
#29121,#29122,#29123,#29124,#29125,#29126,#29127,#29128,#29129,#29130,#29131,
#29132,#29133,#29134,#29135,#29136,#29137,#29138,#29139,#29140,#29141,#29142,
#29143,#29144,#29145,#29146,#29147,#29148,#29149,#29150,#29151,#29152,#29153,
#29154,#29155,#29156,#29157,#29158,#29159,#29160,#29161,#29162,#29163),
(#29164,#29165,#29166,#29167,#29168,#29169,#29170,#29171,#29172,#29173,
#29174,#29175,#29176,#29177,#29178,#29179,#29180,#29181,#29182,#29183,#29184,
#29185,#29186,#29187,#29188,#29189,#29190,#29191,#29192,#29193,#29194,#29195,
#29196,#29197,#29198,#29199,#29200,#29201,#29202,#29203,#29204,#29205,#29206,
#29207,#29208,#29209,#29210,#29211,#29212),(#29213,#29214,#29215,#29216,
#29217,#29218,#29219,#29220,#29221,#29222,#29223,#29224,#29225,#29226,#29227,
#29228,#29229,#29230,#29231,#29232,#29233,#29234,#29235,#29236,#29237,#29238,
#29239,#29240,#29241,#29242,#29243,#29244,#29245,#29246,#29247,#29248,#29249,
#29250,#29251,#29252,#29253,#29254,#29255,#29256,#29257,#29258,#29259,#29260,
#29261),(#29262,#29263,#29264,#29265,#29266,#29267,#29268,#29269,#29270,
#29271,#29272,#29273,#29274,#29275,#29276,#29277,#29278,#29279,#29280,#29281,
#29282,#29283,#29284,#29285,#29286,#29287,#29288,#29289,#29290,#29291,#29292,
#29293,#29294,#29295,#29296,#29297,#29298,#29299,#29300,#29301,#29302,#29303,
#29304,#29305,#29306,#29307,#29308,#29309,#29310),(#29311,#29312,#29313,
#29314,#29315,#29316,#29317,#29318,#29319,#29320,#29321,#29322,#29323,#29324,
#29325,#29326,#29327,#29328,#29329,#29330,#29331,#29332,#29333,#29334,#29335,
#29336,#29337,#29338,#29339,#29340,#29341,#29342,#29343,#29344,#29345,#29346,
#29347,#29348,#29349,#29350,#29351,#29352,#29353,#29354,#29355,#29356,#29357,
#29358,#29359),(#29360,#29361,#29362,#29363,#29364,#29365,#29366,#29367,
#29368,#29369,#29370,#29371,#29372,#29373,#29374,#29375,#29376,#29377,#29378,
#29379,#29380,#29381,#29382,#29383,#29384,#29385,#29386,#29387,#29388,#29389,
#29390,#29391,#29392,#29393,#29394,#29395,#29396,#29397,#29398,#29399,#29400,
#29401,#29402,#29403,#29404,#29405,#29406,#29407,#29408),(#29409,#29410,
#29411,#29412,#29413,#29414,#29415,#29416,#29417,#29418,#29419,#29420,#29421,
#29422,#29423,#29424,#29425,#29426,#29427,#29428,#29429,#29430,#29431,#29432,
#29433,#29434,#29435,#29436,#29437,#29438,#29439,#29440,#29441,#29442,#29443,
#29444,#29445,#29446,#29447,#29448,#29449,#29450,#29451,#29452,#29453,#29454,
#29455,#29456,#29457),(#29458,#29459,#29460,#29461,#29462,#29463,#29464,
#29465,#29466,#29467,#29468,#29469,#29470,#29471,#29472,#29473,#29474,#29475,
#29476,#29477,#29478,#29479,#29480,#29481,#29482,#29483,#29484,#29485,#29486,
#29487,#29488,#29489,#29490,#29491,#29492,#29493,#29494,#29495,#29496,#29497,
#29498,#29499,#29500,#29501,#29502,#29503,#29504,#29505,#29506),(#29507,
#29508,#29509,#29510,#29511,#29512,#29513,#29514,#29515,#29516,#29517,#29518,
#29519,#29520,#29521,#29522,#29523,#29524,#29525,#29526,#29527,#29528,#29529,
#29530,#29531,#29532,#29533,#29534,#29535,#29536,#29537,#29538,#29539,#29540,
#29541,#29542,#29543,#29544,#29545,#29546,#29547,#29548,#29549,#29550,#29551,
#29552,#29553,#29554,#29555),(#29556,#29557,#29558,#29559,#29560,#29561,
#29562,#29563,#29564,#29565,#29566,#29567,#29568,#29569,#29570,#29571,#29572,
#29573,#29574,#29575,#29576,#29577,#29578,#29579,#29580,#29581,#29582,#29583,
#29584,#29585,#29586,#29587,#29588,#29589,#29590,#29591,#29592,#29593,#29594,
#29595,#29596,#29597,#29598,#29599,#29600,#29601,#29602,#29603,#29604),
(#29605,#29606,#29607,#29608,#29609,#29610,#29611,#29612,#29613,#29614,
#29615,#29616,#29617,#29618,#29619,#29620,#29621,#29622,#29623,#29624,#29625,
#29626,#29627,#29628,#29629,#29630,#29631,#29632,#29633,#29634,#29635,#29636,
#29637,#29638,#29639,#29640,#29641,#29642,#29643,#29644,#29645,#29646,#29647,
#29648,#29649,#29650,#29651,#29652,#29653),(#29654,#29655,#29656,#29657,
#29658,#29659,#29660,#29661,#29662,#29663,#29664,#29665,#29666,#29667,#29668,
#29669,#29670,#29671,#29672,#29673,#29674,#29675,#29676,#29677,#29678,#29679,
#29680,#29681,#29682,#29683,#29684,#29685,#29686,#29687,#29688,#29689,#29690,
#29691,#29692,#29693,#29694,#29695,#29696,#29697,#29698,#29699,#29700,#29701,
#29702),(#29703,#29704,#29705,#29706,#29707,#29708,#29709,#29710,#29711,
#29712,#29713,#29714,#29715,#29716,#29717,#29718,#29719,#29720,#29721,#29722,
#29723,#29724,#29725,#29726,#29727,#29728,#29729,#29730,#29731,#29732,#29733,
#29734,#29735,#29736,#29737,#29738,#29739,#29740,#29741,#29742,#29743,#29744,
#29745,#29746,#29747,#29748,#29749,#29750,#29751),(#29752,#29753,#29754,
#29755,#29756,#29757,#29758,#29759,#29760,#29761,#29762,#29763,#29764,#29765,
#29766,#29767,#29768,#29769,#29770,#29771,#29772,#29773,#29774,#29775,#29776,
#29777,#29778,#29779,#29780,#29781,#29782,#29783,#29784,#29785,#29786,#29787,
#29788,#29789,#29790,#29791,#29792,#29793,#29794,#29795,#29796,#29797,#29798,
#29799,#29800),(#29801,#29802,#29803,#29804,#29805,#29806,#29807,#29808,
#29809,#29810,#29811,#29812,#29813,#29814,#29815,#29816,#29817,#29818,#29819,
#29820,#29821,#29822,#29823,#29824,#29825,#29826,#29827,#29828,#29829,#29830,
#29831,#29832,#29833,#29834,#29835,#29836,#29837,#29838,#29839,#29840,#29841,
#29842,#29843,#29844,#29845,#29846,#29847,#29848,#29849),(#29850,#29851,
#29852,#29853,#29854,#29855,#29856,#29857,#29858,#29859,#29860,#29861,#29862,
#29863,#29864,#29865,#29866,#29867,#29868,#29869,#29870,#29871,#29872,#29873,
#29874,#29875,#29876,#29877,#29878,#29879,#29880,#29881,#29882,#29883,#29884,
#29885,#29886,#29887,#29888,#29889,#29890,#29891,#29892,#29893,#29894,#29895,
#29896,#29897,#29898),(#29899,#29900,#29901,#29902,#29903,#29904,#29905,
#29906,#29907,#29908,#29909,#29910,#29911,#29912,#29913,#29914,#29915,#29916,
#29917,#29918,#29919,#29920,#29921,#29922,#29923,#29924,#29925,#29926,#29927,
#29928,#29929,#29930,#29931,#29932,#29933,#29934,#29935,#29936,#29937,#29938,
#29939,#29940,#29941,#29942,#29943,#29944,#29945,#29946,#29947),(#29948,
#29949,#29950,#29951,#29952,#29953,#29954,#29955,#29956,#29957,#29958,#29959,
#29960,#29961,#29962,#29963,#29964,#29965,#29966,#29967,#29968,#29969,#29970,
#29971,#29972,#29973,#29974,#29975,#29976,#29977,#29978,#29979,#29980,#29981,
#29982,#29983,#29984,#29985,#29986,#29987,#29988,#29989,#29990,#29991,#29992,
#29993,#29994,#29995,#29996),(#29997,#29998,#29999,#30000,#30001,#30002,
#30003,#30004,#30005,#30006,#30007,#30008,#30009,#30010,#30011,#30012,#30013,
#30014,#30015,#30016,#30017,#30018,#30019,#30020,#30021,#30022,#30023,#30024,
#30025,#30026,#30027,#30028,#30029,#30030,#30031,#30032,#30033,#30034,#30035,
#30036,#30037,#30038,#30039,#30040,#30041,#30042,#30043,#30044,#30045),
(#30046,#30047,#30048,#30049,#30050,#30051,#30052,#30053,#30054,#30055,
#30056,#30057,#30058,#30059,#30060,#30061,#30062,#30063,#30064,#30065,#30066,
#30067,#30068,#30069,#30070,#30071,#30072,#30073,#30074,#30075,#30076,#30077,
#30078,#30079,#30080,#30081,#30082,#30083,#30084,#30085,#30086,#30087,#30088,
#30089,#30090,#30091,#30092,#30093,#30094),(#30095,#30096,#30097,#30098,
#30099,#30100,#30101,#30102,#30103,#30104,#30105,#30106,#30107,#30108,#30109,
#30110,#30111,#30112,#30113,#30114,#30115,#30116,#30117,#30118,#30119,#30120,
#30121,#30122,#30123,#30124,#30125,#30126,#30127,#30128,#30129,#30130,#30131,
#30132,#30133,#30134,#30135,#30136,#30137,#30138,#30139,#30140,#30141,#30142,
#30143),(#30144,#30145,#30146,#30147,#30148,#30149,#30150,#30151,#30152,
#30153,#30154,#30155,#30156,#30157,#30158,#30159,#30160,#30161,#30162,#30163,
#30164,#30165,#30166,#30167,#30168,#30169,#30170,#30171,#30172,#30173,#30174,
#30175,#30176,#30177,#30178,#30179,#30180,#30181,#30182,#30183,#30184,#30185,
#30186,#30187,#30188,#30189,#30190,#30191,#30192),(#30193,#30194,#30195,
#30196,#30197,#30198,#30199,#30200,#30201,#30202,#30203,#30204,#30205,#30206,
#30207,#30208,#30209,#30210,#30211,#30212,#30213,#30214,#30215,#30216,#30217,
#30218,#30219,#30220,#30221,#30222,#30223,#30224,#30225,#30226,#30227,#30228,
#30229,#30230,#30231,#30232,#30233,#30234,#30235,#30236,#30237,#30238,#30239,
#30240,#30241),(#30242,#30243,#30244,#30245,#30246,#30247,#30248,#30249,
#30250,#30251,#30252,#30253,#30254,#30255,#30256,#30257,#30258,#30259,#30260,
#30261,#30262,#30263,#30264,#30265,#30266,#30267,#30268,#30269,#30270,#30271,
#30272,#30273,#30274,#30275,#30276,#30277,#30278,#30279,#30280,#30281,#30282,
#30283,#30284,#30285,#30286,#30287,#30288,#30289,#30290),(#30291,#30292,
#30293,#30294,#30295,#30296,#30297,#30298,#30299,#30300,#30301,#30302,#30303,
#30304,#30305,#30306,#30307,#30308,#30309,#30310,#30311,#30312,#30313,#30314,
#30315,#30316,#30317,#30318,#30319,#30320,#30321,#30322,#30323,#30324,#30325,
#30326,#30327,#30328,#30329,#30330,#30331,#30332,#30333,#30334,#30335,#30336,
#30337,#30338,#30339),(#30340,#30341,#30342,#30343,#30344,#30345,#30346,
#30347,#30348,#30349,#30350,#30351,#30352,#30353,#30354,#30355,#30356,#30357,
#30358,#30359,#30360,#30361,#30362,#30363,#30364,#30365,#30366,#30367,#30368,
#30369,#30370,#30371,#30372,#30373,#30374,#30375,#30376,#30377,#30378,#30379,
#30380,#30381,#30382,#30383,#30384,#30385,#30386,#30387,#30388),(#30389,
#30390,#30391,#30392,#30393,#30394,#30395,#30396,#30397,#30398,#30399,#30400,
#30401,#30402,#30403,#30404,#30405,#30406,#30407,#30408,#30409,#30410,#30411,
#30412,#30413,#30414,#30415,#30416,#30417,#30418,#30419,#30420,#30421,#30422,
#30423,#30424,#30425,#30426,#30427,#30428,#30429,#30430,#30431,#30432,#30433,
#30434,#30435,#30436,#30437),(#30438,#30439,#30440,#30441,#30442,#30443,
#30444,#30445,#30446,#30447,#30448,#30449,#30450,#30451,#30452,#30453,#30454,
#30455,#30456,#30457,#30458,#30459,#30460,#30461,#30462,#30463,#30464,#30465,
#30466,#30467,#30468,#30469,#30470,#30471,#30472,#30473,#30474,#30475,#30476,
#30477,#30478,#30479,#30480,#30481,#30482,#30483,#30484,#30485,#30486),
(#30487,#30488,#30489,#30490,#30491,#30492,#30493,#30494,#30495,#30496,
#30497,#30498,#30499,#30500,#30501,#30502,#30503,#30504,#30505,#30506,#30507,
#30508,#30509,#30510,#30511,#30512,#30513,#30514,#30515,#30516,#30517,#30518,
#30519,#30520,#30521,#30522,#30523,#30524,#30525,#30526,#30527,#30528,#30529,
#30530,#30531,#30532,#30533,#30534,#30535),(#30536,#30537,#30538,#30539,
#30540,#30541,#30542,#30543,#30544,#30545,#30546,#30547,#30548,#30549,#30550,
#30551,#30552,#30553,#30554,#30555,#30556,#30557,#30558,#30559,#30560,#30561,
#30562,#30563,#30564,#30565,#30566,#30567,#30568,#30569,#30570,#30571,#30572,
#30573,#30574,#30575,#30576,#30577,#30578,#30579,#30580,#30581,#30582,#30583,
#30584),(#30585,#30586,#30587,#30588,#30589,#30590,#30591,#30592,#30593,
#30594,#30595,#30596,#30597,#30598,#30599,#30600,#30601,#30602,#30603,#30604,
#30605,#30606,#30607,#30608,#30609,#30610,#30611,#30612,#30613,#30614,#30615,
#30616,#30617,#30618,#30619,#30620,#30621,#30622,#30623,#30624,#30625,#30626,
#30627,#30628,#30629,#30630,#30631,#30632,#30633),(#30634,#30635,#30636,
#30637,#30638,#30639,#30640,#30641,#30642,#30643,#30644,#30645,#30646,#30647,
#30648,#30649,#30650,#30651,#30652,#30653,#30654,#30655,#30656,#30657,#30658,
#30659,#30660,#30661,#30662,#30663,#30664,#30665,#30666,#30667,#30668,#30669,
#30670,#30671,#30672,#30673,#30674,#30675,#30676,#30677,#30678,#30679,#30680,
#30681,#30682),(#30683,#30684,#30685,#30686,#30687,#30688,#30689,#30690,
#30691,#30692,#30693,#30694,#30695,#30696,#30697,#30698,#30699,#30700,#30701,
#30702,#30703,#30704,#30705,#30706,#30707,#30708,#30709,#30710,#30711,#30712,
#30713,#30714,#30715,#30716,#30717,#30718,#30719,#30720,#30721,#30722,#30723,
#30724,#30725,#30726,#30727,#30728,#30729,#30730,#30731),(#30732,#30733,
#30734,#30735,#30736,#30737,#30738,#30739,#30740,#30741,#30742,#30743,#30744,
#30745,#30746,#30747,#30748,#30749,#30750,#30751,#30752,#30753,#30754,#30755,
#30756,#30757,#30758,#30759,#30760,#30761,#30762,#30763,#30764,#30765,#30766,
#30767,#30768,#30769,#30770,#30771,#30772,#30773,#30774,#30775,#30776,#30777,
#30778,#30779,#30780),(#30781,#30782,#30783,#30784,#30785,#30786,#30787,
#30788,#30789,#30790,#30791,#30792,#30793,#30794,#30795,#30796,#30797,#30798,
#30799,#30800,#30801,#30802,#30803,#30804,#30805,#30806,#30807,#30808,#30809,
#30810,#30811,#30812,#30813,#30814,#30815,#30816,#30817,#30818,#30819,#30820,
#30821,#30822,#30823,#30824,#30825,#30826,#30827,#30828,#30829),(#30830,
#30831,#30832,#30833,#30834,#30835,#30836,#30837,#30838,#30839,#30840,#30841,
#30842,#30843,#30844,#30845,#30846,#30847,#30848,#30849,#30850,#30851,#30852,
#30853,#30854,#30855,#30856,#30857,#30858,#30859,#30860,#30861,#30862,#30863,
#30864,#30865,#30866,#30867,#30868,#30869,#30870,#30871,#30872,#30873,#30874,
#30875,#30876,#30877,#30878),(#30879,#30880,#30881,#30882,#30883,#30884,
#30885,#30886,#30887,#30888,#30889,#30890,#30891,#30892,#30893,#30894,#30895,
#30896,#30897,#30898,#30899,#30900,#30901,#30902,#30903,#30904,#30905,#30906,
#30907,#30908,#30909,#30910,#30911,#30912,#30913,#30914,#30915,#30916,#30917,
#30918,#30919,#30920,#30921,#30922,#30923,#30924,#30925,#30926,#30927),
(#30928,#30929,#30930,#30931,#30932,#30933,#30934,#30935,#30936,#30937,
#30938,#30939,#30940,#30941,#30942,#30943,#30944,#30945,#30946,#30947,#30948,
#30949,#30950,#30951,#30952,#30953,#30954,#30955,#30956,#30957,#30958,#30959,
#30960,#30961,#30962,#30963,#30964,#30965,#30966,#30967,#30968,#30969,#30970,
#30971,#30972,#30973,#30974,#30975,#30976),(#30977,#30978,#30979,#30980,
#30981,#30982,#30983,#30984,#30985,#30986,#30987,#30988,#30989,#30990,#30991,
#30992,#30993,#30994,#30995,#30996,#30997,#30998,#30999,#31000,#31001,#31002,
#31003,#31004,#31005,#31006,#31007,#31008,#31009,#31010,#31011,#31012,#31013,
#31014,#31015,#31016,#31017,#31018,#31019,#31020,#31021,#31022,#31023,#31024,
#31025),(#31026,#31027,#31028,#31029,#31030,#31031,#31032,#31033,#31034,
#31035,#31036,#31037,#31038,#31039,#31040,#31041,#31042,#31043,#31044,#31045,
#31046,#31047,#31048,#31049,#31050,#31051,#31052,#31053,#31054,#31055,#31056,
#31057,#31058,#31059,#31060,#31061,#31062,#31063,#31064,#31065,#31066,#31067,
#31068,#31069,#31070,#31071,#31072,#31073,#31074),(#31075,#31076,#31077,
#31078,#31079,#31080,#31081,#31082,#31083,#31084,#31085,#31086,#31087,#31088,
#31089,#31090,#31091,#31092,#31093,#31094,#31095,#31096,#31097,#31098,#31099,
#31100,#31101,#31102,#31103,#31104,#31105,#31106,#31107,#31108,#31109,#31110,
#31111,#31112,#31113,#31114,#31115,#31116,#31117,#31118,#31119,#31120,#31121,
#31122,#31123),(#31124,#31125,#31126,#31127,#31128,#31129,#31130,#31131,
#31132,#31133,#31134,#31135,#31136,#31137,#31138,#31139,#31140,#31141,#31142,
#31143,#31144,#31145,#31146,#31147,#31148,#31149,#31150,#31151,#31152,#31153,
#31154,#31155,#31156,#31157,#31158,#31159,#31160,#31161,#31162,#31163,#31164,
#31165,#31166,#31167,#31168,#31169,#31170,#31171,#31172),(#31173,#31174,
#31175,#31176,#31177,#31178,#31179,#31180,#31181,#31182,#31183,#31184,#31185,
#31186,#31187,#31188,#31189,#31190,#31191,#31192,#31193,#31194,#31195,#31196,
#31197,#31198,#31199,#31200,#31201,#31202,#31203,#31204,#31205,#31206,#31207,
#31208,#31209,#31210,#31211,#31212,#31213,#31214,#31215,#31216,#31217,#31218,
#31219,#31220,#31221),(#31222,#31223,#31224,#31225,#31226,#31227,#31228,
#31229,#31230,#31231,#31232,#31233,#31234,#31235,#31236,#31237,#31238,#31239,
#31240,#31241,#31242,#31243,#31244,#31245,#31246,#31247,#31248,#31249,#31250,
#31251,#31252,#31253,#31254,#31255,#31256,#31257,#31258,#31259,#31260,#31261,
#31262,#31263,#31264,#31265,#31266,#31267,#31268,#31269,#31270),(#31271,
#31272,#31273,#31274,#31275,#31276,#31277,#31278,#31279,#31280,#31281,#31282,
#31283,#31284,#31285,#31286,#31287,#31288,#31289,#31290,#31291,#31292,#31293,
#31294,#31295,#31296,#31297,#31298,#31299,#31300,#31301,#31302,#31303,#31304,
#31305,#31306,#31307,#31308,#31309,#31310,#31311,#31312,#31313,#31314,#31315,
#31316,#31317,#31318,#31319),(#31320,#31321,#31322,#31323,#31324,#31325,
#31326,#31327,#31328,#31329,#31330,#31331,#31332,#31333,#31334,#31335,#31336,
#31337,#31338,#31339,#31340,#31341,#31342,#31343,#31344,#31345,#31346,#31347,
#31348,#31349,#31350,#31351,#31352,#31353,#31354,#31355,#31356,#31357,#31358,
#31359,#31360,#31361,#31362,#31363,#31364,#31365,#31366,#31367,#31368),
(#31369,#31370,#31371,#31372,#31373,#31374,#31375,#31376,#31377,#31378,
#31379,#31380,#31381,#31382,#31383,#31384,#31385,#31386,#31387,#31388,#31389,
#31390,#31391,#31392,#31393,#31394,#31395,#31396,#31397,#31398,#31399,#31400,
#31401,#31402,#31403,#31404,#31405,#31406,#31407,#31408,#31409,#31410,#31411,
#31412,#31413,#31414,#31415,#31416,#31417),(#31418,#31419,#31420,#31421,
#31422,#31423,#31424,#31425,#31426,#31427,#31428,#31429,#31430,#31431,#31432,
#31433,#31434,#31435,#31436,#31437,#31438,#31439,#31440,#31441,#31442,#31443,
#31444,#31445,#31446,#31447,#31448,#31449,#31450,#31451,#31452,#31453,#31454,
#31455,#31456,#31457,#31458,#31459,#31460,#31461,#31462,#31463,#31464,#31465,
#31466),(#31467,#31468,#31469,#31470,#31471,#31472,#31473,#31474,#31475,
#31476,#31477,#31478,#31479,#31480,#31481,#31482,#31483,#31484,#31485,#31486,
#31487,#31488,#31489,#31490,#31491,#31492,#31493,#31494,#31495,#31496,#31497,
#31498,#31499,#31500,#31501,#31502,#31503,#31504,#31505,#31506,#31507,#31508,
#31509,#31510,#31511,#31512,#31513,#31514,#31515),(#31516,#31517,#31518,
#31519,#31520,#31521,#31522,#31523,#31524,#31525,#31526,#31527,#31528,#31529,
#31530,#31531,#31532,#31533,#31534,#31535,#31536,#31537,#31538,#31539,#31540,
#31541,#31542,#31543,#31544,#31545,#31546,#31547,#31548,#31549,#31550,#31551,
#31552,#31553,#31554,#31555,#31556,#31557,#31558,#31559,#31560,#31561,#31562,
#31563,#31564),(#31565,#31566,#31567,#31568,#31569,#31570,#31571,#31572,
#31573,#31574,#31575,#31576,#31577,#31578,#31579,#31580,#31581,#31582,#31583,
#31584,#31585,#31586,#31587,#31588,#31589,#31590,#31591,#31592,#31593,#31594,
#31595,#31596,#31597,#31598,#31599,#31600,#31601,#31602,#31603,#31604,#31605,
#31606,#31607,#31608,#31609,#31610,#31611,#31612,#31613),(#31614,#31615,
#31616,#31617,#31618,#31619,#31620,#31621,#31622,#31623,#31624,#31625,#31626,
#31627,#31628,#31629,#31630,#31631,#31632,#31633,#31634,#31635,#31636,#31637,
#31638,#31639,#31640,#31641,#31642,#31643,#31644,#31645,#31646,#31647,#31648,
#31649,#31650,#31651,#31652,#31653,#31654,#31655,#31656,#31657,#31658,#31659,
#31660,#31661,#31662),(#31663,#31664,#31665,#31666,#31667,#31668,#31669,
#31670,#31671,#31672,#31673,#31674,#31675,#31676,#31677,#31678,#31679,#31680,
#31681,#31682,#31683,#31684,#31685,#31686,#31687,#31688,#31689,#31690,#31691,
#31692,#31693,#31694,#31695,#31696,#31697,#31698,#31699,#31700,#31701,#31702,
#31703,#31704,#31705,#31706,#31707,#31708,#31709,#31710,#31711),(#31712,
#31713,#31714,#31715,#31716,#31717,#31718,#31719,#31720,#31721,#31722,#31723,
#31724,#31725,#31726,#31727,#31728,#31729,#31730,#31731,#31732,#31733,#31734,
#31735,#31736,#31737,#31738,#31739,#31740,#31741,#31742,#31743,#31744,#31745,
#31746,#31747,#31748,#31749,#31750,#31751,#31752,#31753,#31754,#31755,#31756,
#31757,#31758,#31759,#31760),(#31761,#31762,#31763,#31764,#31765,#31766,
#31767,#31768,#31769,#31770,#31771,#31772,#31773,#31774,#31775,#31776,#31777,
#31778,#31779,#31780,#31781,#31782,#31783,#31784,#31785,#31786,#31787,#31788,
#31789,#31790,#31791,#31792,#31793,#31794,#31795,#31796,#31797,#31798,#31799,
#31800,#31801,#31802,#31803,#31804,#31805,#31806,#31807,#31808,#31809),
(#31810,#31811,#31812,#31813,#31814,#31815,#31816,#31817,#31818,#31819,
#31820,#31821,#31822,#31823,#31824,#31825,#31826,#31827,#31828,#31829,#31830,
#31831,#31832,#31833,#31834,#31835,#31836,#31837,#31838,#31839,#31840,#31841,
#31842,#31843,#31844,#31845,#31846,#31847,#31848,#31849,#31850,#31851,#31852,
#31853,#31854,#31855,#31856,#31857,#31858),(#31859,#31860,#31861,#31862,
#31863,#31864,#31865,#31866,#31867,#31868,#31869,#31870,#31871,#31872,#31873,
#31874,#31875,#31876,#31877,#31878,#31879,#31880,#31881,#31882,#31883,#31884,
#31885,#31886,#31887,#31888,#31889,#31890,#31891,#31892,#31893,#31894,#31895,
#31896,#31897,#31898,#31899,#31900,#31901,#31902,#31903,#31904,#31905,#31906,
#31907),(#31908,#31909,#31910,#31911,#31912,#31913,#31914,#31915,#31916,
#31917,#31918,#31919,#31920,#31921,#31922,#31923,#31924,#31925,#31926,#31927,
#31928,#31929,#31930,#31931,#31932,#31933,#31934,#31935,#31936,#31937,#31938,
#31939,#31940,#31941,#31942,#31943,#31944,#31945,#31946,#31947,#31948,#31949,
#31950,#31951,#31952,#31953,#31954,#31955,#31956),(#31957,#31958,#31959,
#31960,#31961,#31962,#31963,#31964,#31965,#31966,#31967,#31968,#31969,#31970,
#31971,#31972,#31973,#31974,#31975,#31976,#31977,#31978,#31979,#31980,#31981,
#31982,#31983,#31984,#31985,#31986,#31987,#31988,#31989,#31990,#31991,#31992,
#31993,#31994,#31995,#31996,#31997,#31998,#31999,#32000,#32001,#32002,#32003,
#32004,#32005),(#32006,#32007,#32008,#32009,#32010,#32011,#32012,#32013,
#32014,#32015,#32016,#32017,#32018,#32019,#32020,#32021,#32022,#32023,#32024,
#32025,#32026,#32027,#32028,#32029,#32030,#32031,#32032,#32033,#32034,#32035,
#32036,#32037,#32038,#32039,#32040,#32041,#32042,#32043,#32044,#32045,#32046,
#32047,#32048,#32049,#32050,#32051,#32052,#32053,#32054),(#32055,#32056,
#32057,#32058,#32059,#32060,#32061,#32062,#32063,#32064,#32065,#32066,#32067,
#32068,#32069,#32070,#32071,#32072,#32073,#32074,#32075,#32076,#32077,#32078,
#32079,#32080,#32081,#32082,#32083,#32084,#32085,#32086,#32087,#32088,#32089,
#32090,#32091,#32092,#32093,#32094,#32095,#32096,#32097,#32098,#32099,#32100,
#32101,#32102,#32103),(#32104,#32105,#32106,#32107,#32108,#32109,#32110,
#32111,#32112,#32113,#32114,#32115,#32116,#32117,#32118,#32119,#32120,#32121,
#32122,#32123,#32124,#32125,#32126,#32127,#32128,#32129,#32130,#32131,#32132,
#32133,#32134,#32135,#32136,#32137,#32138,#32139,#32140,#32141,#32142,#32143,
#32144,#32145,#32146,#32147,#32148,#32149,#32150,#32151,#32152),(#32153,
#32154,#32155,#32156,#32157,#32158,#32159,#32160,#32161,#32162,#32163,#32164,
#32165,#32166,#32167,#32168,#32169,#32170,#32171,#32172,#32173,#32174,#32175,
#32176,#32177,#32178,#32179,#32180,#32181,#32182,#32183,#32184,#32185,#32186,
#32187,#32188,#32189,#32190,#32191,#32192,#32193,#32194,#32195,#32196,#32197,
#32198,#32199,#32200,#32201),(#32202,#32203,#32204,#32205,#32206,#32207,
#32208,#32209,#32210,#32211,#32212,#32213,#32214,#32215,#32216,#32217,#32218,
#32219,#32220,#32221,#32222,#32223,#32224,#32225,#32226,#32227,#32228,#32229,
#32230,#32231,#32232,#32233,#32234,#32235,#32236,#32237,#32238,#32239,#32240,
#32241,#32242,#32243,#32244,#32245,#32246,#32247,#32248,#32249,#32250),
(#32251,#32252,#32253,#32254,#32255,#32256,#32257,#32258,#32259,#32260,
#32261,#32262,#32263,#32264,#32265,#32266,#32267,#32268,#32269,#32270,#32271,
#32272,#32273,#32274,#32275,#32276,#32277,#32278,#32279,#32280,#32281,#32282,
#32283,#32284,#32285,#32286,#32287,#32288,#32289,#32290,#32291,#32292,#32293,
#32294,#32295,#32296,#32297,#32298,#32299),(#32300,#32301,#32302,#32303,
#32304,#32305,#32306,#32307,#32308,#32309,#32310,#32311,#32312,#32313,#32314,
#32315,#32316,#32317,#32318,#32319,#32320,#32321,#32322,#32323,#32324,#32325,
#32326,#32327,#32328,#32329,#32330,#32331,#32332,#32333,#32334,#32335,#32336,
#32337,#32338,#32339,#32340,#32341,#32342,#32343,#32344,#32345,#32346,#32347,
#32348),(#32349,#32350,#32351,#32352,#32353,#32354,#32355,#32356,#32357,
#32358,#32359,#32360,#32361,#32362,#32363,#32364,#32365,#32366,#32367,#32368,
#32369,#32370,#32371,#32372,#32373,#32374,#32375,#32376,#32377,#32378,#32379,
#32380,#32381,#32382,#32383,#32384,#32385,#32386,#32387,#32388,#32389,#32390,
#32391,#32392,#32393,#32394,#32395,#32396,#32397),(#32398,#32399,#32400,
#32401,#32402,#32403,#32404,#32405,#32406,#32407,#32408,#32409,#32410,#32411,
#32412,#32413,#32414,#32415,#32416,#32417,#32418,#32419,#32420,#32421,#32422,
#32423,#32424,#32425,#32426,#32427,#32428,#32429,#32430,#32431,#32432,#32433,
#32434,#32435,#32436,#32437,#32438,#32439,#32440,#32441,#32442,#32443,#32444,
#32445,#32446),(#32447,#32448,#32449,#32450,#32451,#32452,#32453,#32454,
#32455,#32456,#32457,#32458,#32459,#32460,#32461,#32462,#32463,#32464,#32465,
#32466,#32467,#32468,#32469,#32470,#32471,#32472,#32473,#32474,#32475,#32476,
#32477,#32478,#32479,#32480,#32481,#32482,#32483,#32484,#32485,#32486,#32487,
#32488,#32489,#32490,#32491,#32492,#32493,#32494,#32495),(#32496,#32497,
#32498,#32499,#32500,#32501,#32502,#32503,#32504,#32505,#32506,#32507,#32508,
#32509,#32510,#32511,#32512,#32513,#32514,#32515,#32516,#32517,#32518,#32519,
#32520,#32521,#32522,#32523,#32524,#32525,#32526,#32527,#32528,#32529,#32530,
#32531,#32532,#32533,#32534,#32535,#32536,#32537,#32538,#32539,#32540,#32541,
#32542,#32543,#32544),(#32545,#32546,#32547,#32548,#32549,#32550,#32551,
#32552,#32553,#32554,#32555,#32556,#32557,#32558,#32559,#32560,#32561,#32562,
#32563,#32564,#32565,#32566,#32567,#32568,#32569,#32570,#32571,#32572,#32573,
#32574,#32575,#32576,#32577,#32578,#32579,#32580,#32581,#32582,#32583,#32584,
#32585,#32586,#32587,#32588,#32589,#32590,#32591,#32592,#32593),(#32594,
#32595,#32596,#32597,#32598,#32599,#32600,#32601,#32602,#32603,#32604,#32605,
#32606,#32607,#32608,#32609,#32610,#32611,#32612,#32613,#32614,#32615,#32616,
#32617,#32618,#32619,#32620,#32621,#32622,#32623,#32624,#32625,#32626,#32627,
#32628,#32629,#32630,#32631,#32632,#32633,#32634,#32635,#32636,#32637,#32638,
#32639,#32640,#32641,#32642),(#32643,#32644,#32645,#32646,#32647,#32648,
#32649,#32650,#32651,#32652,#32653,#32654,#32655,#32656,#32657,#32658,#32659,
#32660,#32661,#32662,#32663,#32664,#32665,#32666,#32667,#32668,#32669,#32670,
#32671,#32672,#32673,#32674,#32675,#32676,#32677,#32678,#32679,#32680,#32681,
#32682,#32683,#32684,#32685,#32686,#32687,#32688,#32689,#32690,#32691),
(#32692,#32693,#32694,#32695,#32696,#32697,#32698,#32699,#32700,#32701,
#32702,#32703,#32704,#32705,#32706,#32707,#32708,#32709,#32710,#32711,#32712,
#32713,#32714,#32715,#32716,#32717,#32718,#32719,#32720,#32721,#32722,#32723,
#32724,#32725,#32726,#32727,#32728,#32729,#32730,#32731,#32732,#32733,#32734,
#32735,#32736,#32737,#32738,#32739,#32740),(#32741,#32742,#32743,#32744,
#32745,#32746,#32747,#32748,#32749,#32750,#32751,#32752,#32753,#32754,#32755,
#32756,#32757,#32758,#32759,#32760,#32761,#32762,#32763,#32764,#32765,#32766,
#32767,#32768,#32769,#32770,#32771,#32772,#32773,#32774,#32775,#32776,#32777,
#32778,#32779,#32780,#32781,#32782,#32783,#32784,#32785,#32786,#32787,#32788,
#32789),(#32790,#32791,#32792,#32793,#32794,#32795,#32796,#32797,#32798,
#32799,#32800,#32801,#32802,#32803,#32804,#32805,#32806,#32807,#32808,#32809,
#32810,#32811,#32812,#32813,#32814,#32815,#32816,#32817,#32818,#32819,#32820,
#32821,#32822,#32823,#32824,#32825,#32826,#32827,#32828,#32829,#32830,#32831,
#32832,#32833,#32834,#32835,#32836,#32837,#32838),(#32839,#32840,#32841,
#32842,#32843,#32844,#32845,#32846,#32847,#32848,#32849,#32850,#32851,#32852,
#32853,#32854,#32855,#32856,#32857,#32858,#32859,#32860,#32861,#32862,#32863,
#32864,#32865,#32866,#32867,#32868,#32869,#32870,#32871,#32872,#32873,#32874,
#32875,#32876,#32877,#32878,#32879,#32880,#32881,#32882,#32883,#32884,#32885,
#32886,#32887),(#32888,#32889,#32890,#32891,#32892,#32893,#32894,#32895,
#32896,#32897,#32898,#32899,#32900,#32901,#32902,#32903,#32904,#32905,#32906,
#32907,#32908,#32909,#32910,#32911,#32912,#32913,#32914,#32915,#32916,#32917,
#32918,#32919,#32920,#32921,#32922,#32923,#32924,#32925,#32926,#32927,#32928,
#32929,#32930,#32931,#32932,#32933,#32934,#32935,#32936),(#32937,#32938,
#32939,#32940,#32941,#32942,#32943,#32944,#32945,#32946,#32947,#32948,#32949,
#32950,#32951,#32952,#32953,#32954,#32955,#32956,#32957,#32958,#32959,#32960,
#32961,#32962,#32963,#32964,#32965,#32966,#32967,#32968,#32969,#32970,#32971,
#32972,#32973,#32974,#32975,#32976,#32977,#32978,#32979,#32980,#32981,#32982,
#32983,#32984,#32985),(#32986,#32987,#32988,#32989,#32990,#32991,#32992,
#32993,#32994,#32995,#32996,#32997,#32998,#32999,#33000,#33001,#33002,#33003,
#33004,#33005,#33006,#33007,#33008,#33009,#33010,#33011,#33012,#33013,#33014,
#33015,#33016,#33017,#33018,#33019,#33020,#33021,#33022,#33023,#33024,#33025,
#33026,#33027,#33028,#33029,#33030,#33031,#33032,#33033,#33034),(#33035,
#33036,#33037,#33038,#33039,#33040,#33041,#33042,#33043,#33044,#33045,#33046,
#33047,#33048,#33049,#33050,#33051,#33052,#33053,#33054,#33055,#33056,#33057,
#33058,#33059,#33060,#33061,#33062,#33063,#33064,#33065,#33066,#33067,#33068,
#33069,#33070,#33071,#33072,#33073,#33074,#33075,#33076,#33077,#33078,#33079,
#33080,#33081,#33082,#33083),(#33084,#33085,#33086,#33087,#33088,#33089,
#33090,#33091,#33092,#33093,#33094,#33095,#33096,#33097,#33098,#33099,#33100,
#33101,#33102,#33103,#33104,#33105,#33106,#33107,#33108,#33109,#33110,#33111,
#33112,#33113,#33114,#33115,#33116,#33117,#33118,#33119,#33120,#33121,#33122,
#33123,#33124,#33125,#33126,#33127,#33128,#33129,#33130,#33131,#33132),
(#33133,#33134,#33135,#33136,#33137,#33138,#33139,#33140,#33141,#33142,
#33143,#33144,#33145,#33146,#33147,#33148,#33149,#33150,#33151,#33152,#33153,
#33154,#33155,#33156,#33157,#33158,#33159,#33160,#33161,#33162,#33163,#33164,
#33165,#33166,#33167,#33168,#33169,#33170,#33171,#33172,#33173,#33174,#33175,
#33176,#33177,#33178,#33179,#33180,#33181),(#33182,#33183,#33184,#33185,
#33186,#33187,#33188,#33189,#33190,#33191,#33192,#33193,#33194,#33195,#33196,
#33197,#33198,#33199,#33200,#33201,#33202,#33203,#33204,#33205,#33206,#33207,
#33208,#33209,#33210,#33211,#33212,#33213,#33214,#33215,#33216,#33217,#33218,
#33219,#33220,#33221,#33222,#33223,#33224,#33225,#33226,#33227,#33228,#33229,
#33230),(#33231,#33232,#33233,#33234,#33235,#33236,#33237,#33238,#33239,
#33240,#33241,#33242,#33243,#33244,#33245,#33246,#33247,#33248,#33249,#33250,
#33251,#33252,#33253,#33254,#33255,#33256,#33257,#33258,#33259,#33260,#33261,
#33262,#33263,#33264,#33265,#33266,#33267,#33268,#33269,#33270,#33271,#33272,
#33273,#33274,#33275,#33276,#33277,#33278,#33279),(#33280,#33281,#33282,
#33283,#33284,#33285,#33286,#33287,#33288,#33289,#33290,#33291,#33292,#33293,
#33294,#33295,#33296,#33297,#33298,#33299,#33300,#33301,#33302,#33303,#33304,
#33305,#33306,#33307,#33308,#33309,#33310,#33311,#33312,#33313,#33314,#33315,
#33316,#33317,#33318,#33319,#33320,#33321,#33322,#33323,#33324,#33325,#33326,
#33327,#33328),(#33329,#33330,#33331,#33332,#33333,#33334,#33335,#33336,
#33337,#33338,#33339,#33340,#33341,#33342,#33343,#33344,#33345,#33346,#33347,
#33348,#33349,#33350,#33351,#33352,#33353,#33354,#33355,#33356,#33357,#33358,
#33359,#33360,#33361,#33362,#33363,#33364,#33365,#33366,#33367,#33368,#33369,
#33370,#33371,#33372,#33373,#33374,#33375,#33376,#33377),(#33378,#33379,
#33380,#33381,#33382,#33383,#33384,#33385,#33386,#33387,#33388,#33389,#33390,
#33391,#33392,#33393,#33394,#33395,#33396,#33397,#33398,#33399,#33400,#33401,
#33402,#33403,#33404,#33405,#33406,#33407,#33408,#33409,#33410,#33411,#33412,
#33413,#33414,#33415,#33416,#33417,#33418,#33419,#33420,#33421,#33422,#33423,
#33424,#33425,#33426),(#33427,#33428,#33429,#33430,#33431,#33432,#33433,
#33434,#33435,#33436,#33437,#33438,#33439,#33440,#33441,#33442,#33443,#33444,
#33445,#33446,#33447,#33448,#33449,#33450,#33451,#33452,#33453,#33454,#33455,
#33456,#33457,#33458,#33459,#33460,#33461,#33462,#33463,#33464,#33465,#33466,
#33467,#33468,#33469,#33470,#33471,#33472,#33473,#33474,#33475),(#33476,
#33477,#33478,#33479,#33480,#33481,#33482,#33483,#33484,#33485,#33486,#33487,
#33488,#33489,#33490,#33491,#33492,#33493,#33494,#33495,#33496,#33497,#33498,
#33499,#33500,#33501,#33502,#33503,#33504,#33505,#33506,#33507,#33508,#33509,
#33510,#33511,#33512,#33513,#33514,#33515,#33516,#33517,#33518,#33519,#33520,
#33521,#33522,#33523,#33524),(#33525,#33526,#33527,#33528,#33529,#33530,
#33531,#33532,#33533,#33534,#33535,#33536,#33537,#33538,#33539,#33540,#33541,
#33542,#33543,#33544,#33545,#33546,#33547,#33548,#33549,#33550,#33551,#33552,
#33553,#33554,#33555,#33556,#33557,#33558,#33559,#33560,#33561,#33562,#33563,
#33564,#33565,#33566,#33567,#33568,#33569,#33570,#33571,#33572,#33573),
(#33574,#33575,#33576,#33577,#33578,#33579,#33580,#33581,#33582,#33583,
#33584,#33585,#33586,#33587,#33588,#33589,#33590,#33591,#33592,#33593,#33594,
#33595,#33596,#33597,#33598,#33599,#33600,#33601,#33602,#33603,#33604,#33605,
#33606,#33607,#33608,#33609,#33610,#33611,#33612,#33613,#33614,#33615,#33616,
#33617,#33618,#33619,#33620,#33621,#33622),(#33623,#33624,#33625,#33626,
#33627,#33628,#33629,#33630,#33631,#33632,#33633,#33634,#33635,#33636,#33637,
#33638,#33639,#33640,#33641,#33642,#33643,#33644,#33645,#33646,#33647,#33648,
#33649,#33650,#33651,#33652,#33653,#33654,#33655,#33656,#33657,#33658,#33659,
#33660,#33661,#33662,#33663,#33664,#33665,#33666,#33667,#33668,#33669,#33670,
#33671),(#33672,#33673,#33674,#33675,#33676,#33677,#33678,#33679,#33680,
#33681,#33682,#33683,#33684,#33685,#33686,#33687,#33688,#33689,#33690,#33691,
#33692,#33693,#33694,#33695,#33696,#33697,#33698,#33699,#33700,#33701,#33702,
#33703,#33704,#33705,#33706,#33707,#33708,#33709,#33710,#33711,#33712,#33713,
#33714,#33715,#33716,#33717,#33718,#33719,#33720)),.UNSPECIFIED.,.F.,.F.,
 .F.,(4,3,3,3,3,3,3,3,3,3,3,3,3,3,3,3,3,3,3,3,3,3,3,3,3,3,3,3,3,3,3,3,3,
3,3,3,3,3,3,3,4),(4,3,3,3,3,3,3,3,3,3,3,3,3,3,3,3,4),(-1.4142404152185E-5,
-3.89974866163591E-6,-1.33908478899864E-6,-5.87528526800003E-8,1.22157908363864E-6,
6.34290682891319E-6,2.68282178100114E-5,4.73135287911096E-5,6.77988397722078E-5,
8.8284150753306E-5,0.000108769461734404,0.000129254772715502,0.000149740083696601,
0.000190710705658797,0.000231681327620994,0.00027265194958319,0.000313622571545386,
0.000354593193507583,0.000395563815469779,0.000477505059394172,0.000559446303318565,
0.000641387547242958,0.00072332879116735,0.000805270035091743,0.000887211279016136,
0.000969152522940529,0.00113303501078931,0.0012969174986381,0.00146079998648689,
0.00162468247433567,0.00178856496218446,0.00195244745003324,0.00228021242573081,
0.00260797740142839,0.00293574237712596,0.00326350735282353,0.0035912723285211,
0.00391903730421867,0.00424680227991624,0.00457456725561381,0.00528564362278571),
(0.,0.0625,0.125,0.1875,0.25,0.3125,0.375,0.4375,0.5,0.5625,0.625,0.6875,
0.75,0.8125,0.875,0.9375,1.00005554641578),.UNSPECIFIED.);
#194=FACE_BOUND('',#4577,.T.);
#195=FACE_BOUND('',#4579,.T.);
#196=FACE_BOUND('',#4581,.T.);
#197=FACE_BOUND('',#4604,.T.);
#198=FACE_BOUND('',#4623,.T.);
#199=FACE_BOUND('',#4632,.T.);
#200=FACE_BOUND('',#4638,.T.);
#201=FACE_BOUND('',#4639,.T.);
#202=FACE_BOUND('',#4642,.T.);
#203=FACE_BOUND('',#4643,.T.);
#204=FACE_BOUND('',#4645,.T.);
#205=FACE_BOUND('',#4646,.T.);
#206=FACE_BOUND('',#4648,.T.);
#207=FACE_BOUND('',#4652,.T.);
#208=FACE_BOUND('',#4653,.T.);
#209=FACE_BOUND('',#4655,.T.);
#210=FACE_BOUND('',#4662,.T.);
#211=FACE_BOUND('',#4669,.T.);
#212=FACE_BOUND('',#4694,.T.);
#213=FACE_BOUND('',#4696,.T.);
#214=FACE_BOUND('',#4697,.T.);
#215=FACE_BOUND('',#4698,.T.);
#216=FACE_BOUND('',#4700,.T.);
#217=FACE_BOUND('',#4826,.T.);
#218=FACE_BOUND('',#4828,.T.);
#219=FACE_BOUND('',#4832,.T.);
#220=FACE_BOUND('',#4865,.T.);
#221=FACE_BOUND('',#4898,.T.);
#222=FACE_BOUND('',#4899,.T.);
#223=FACE_BOUND('',#4900,.T.);
#224=FACE_BOUND('',#4912,.T.);
#225=FACE_BOUND('',#5012,.T.);
#226=FACE_BOUND('',#5013,.T.);
#227=FACE_BOUND('',#5014,.T.);
#228=FACE_BOUND('',#5015,.T.);
#229=FACE_BOUND('',#5017,.T.);
#230=FACE_BOUND('',#5043,.T.);
#231=FACE_BOUND('',#5050,.T.);
#232=FACE_BOUND('',#5073,.T.);
#233=FACE_BOUND('',#5078,.T.);
#234=FACE_BOUND('',#5113,.T.);
#235=FACE_BOUND('',#5164,.T.);
#236=FACE_BOUND('',#5166,.T.);
#237=FACE_BOUND('',#5176,.T.);
#238=FACE_BOUND('',#5179,.T.);
#239=FACE_BOUND('',#5183,.T.);
#240=FACE_BOUND('',#5187,.T.);
#241=FACE_BOUND('',#5203,.T.);
#242=FACE_BOUND('',#5205,.T.);
#243=FACE_BOUND('',#5207,.T.);
#244=FACE_BOUND('',#5221,.T.);
#245=FACE_BOUND('',#5223,.T.);
#246=FACE_BOUND('',#5224,.T.);
#247=FACE_BOUND('',#5225,.T.);
#248=FACE_BOUND('',#5228,.T.);
#249=FACE_BOUND('',#5229,.T.);
#250=FACE_BOUND('',#5235,.T.);
#251=FACE_BOUND('',#5236,.T.);
#252=FACE_BOUND('',#5237,.T.);
#253=FACE_BOUND('',#5241,.T.);
#254=FACE_BOUND('',#5242,.T.);
#255=FACE_BOUND('',#5246,.T.);
#256=FACE_BOUND('',#5250,.T.);
#257=FACE_BOUND('',#5253,.T.);
#258=FACE_BOUND('',#5265,.T.);
#259=FACE_BOUND('',#5266,.T.);
#260=FACE_BOUND('',#5277,.T.);
#261=FACE_BOUND('',#5278,.T.);
#262=FACE_BOUND('',#5319,.T.);
#263=FACE_BOUND('',#5320,.T.);
#264=FACE_BOUND('',#5321,.T.);
#265=FACE_BOUND('',#5370,.T.);
#266=FACE_BOUND('',#5374,.T.);
#267=FACE_BOUND('',#5378,.T.);
#268=FACE_BOUND('',#5384,.T.);
#269=FACE_BOUND('',#5386,.T.);
#270=FACE_BOUND('',#5387,.T.);
#271=FACE_BOUND('',#5412,.T.);
#272=FACE_BOUND('',#5413,.T.);
#273=FACE_BOUND('',#5448,.T.);
#274=FACE_BOUND('',#5461,.T.);
#275=FACE_BOUND('',#5465,.T.);
#276=FACE_BOUND('',#5467,.T.);
#277=FACE_BOUND('',#5497,.T.);
#278=FACE_BOUND('',#5507,.T.);
#279=PLANE('',#15399);
#280=PLANE('',#15400);
#281=PLANE('',#15401);
#282=PLANE('',#15402);
#283=PLANE('',#15403);
#284=PLANE('',#15404);
#285=PLANE('',#15405);
#286=PLANE('',#15406);
#287=PLANE('',#15407);
#288=PLANE('',#15408);
#289=PLANE('',#15409);
#290=PLANE('',#15410);
#291=PLANE('',#15411);
#292=PLANE('',#15412);
#293=PLANE('',#15413);
#294=PLANE('',#15414);
#295=PLANE('',#15415);
#296=PLANE('',#15416);
#297=PLANE('',#15417);
#298=PLANE('',#15418);
#299=PLANE('',#15419);
#300=PLANE('',#15420);
#301=PLANE('',#15421);
#302=PLANE('',#15422);
#303=PLANE('',#15423);
#304=PLANE('',#15424);
#305=PLANE('',#15425);
#306=PLANE('',#15426);
#307=PLANE('',#15427);
#308=PLANE('',#15428);
#309=PLANE('',#15429);
#310=PLANE('',#15430);
#311=PLANE('',#15431);
#312=PLANE('',#15432);
#313=PLANE('',#15433);
#314=PLANE('',#15434);
#315=PLANE('',#15435);
#316=PLANE('',#15436);
#317=PLANE('',#15437);
#318=PLANE('',#15438);
#319=PLANE('',#15439);
#320=PLANE('',#15440);
#321=PLANE('',#15441);
#322=PLANE('',#15448);
#323=PLANE('',#15452);
#324=PLANE('',#15453);
#325=PLANE('',#15454);
#326=PLANE('',#15455);
#327=PLANE('',#15456);
#328=PLANE('',#15457);
#329=PLANE('',#15458);
#330=PLANE('',#15459);
#331=PLANE('',#15460);
#332=PLANE('',#15461);
#333=PLANE('',#15462);
#334=PLANE('',#15463);
#335=PLANE('',#15464);
#336=PLANE('',#15465);
#337=PLANE('',#15466);
#338=PLANE('',#15467);
#339=PLANE('',#15468);
#340=PLANE('',#15469);
#341=PLANE('',#15470);
#342=PLANE('',#15508);
#343=PLANE('',#15509);
#344=PLANE('',#15510);
#345=PLANE('',#15511);
#346=PLANE('',#15512);
#347=PLANE('',#15513);
#348=PLANE('',#15514);
#349=PLANE('',#15515);
#350=PLANE('',#15516);
#351=PLANE('',#15517);
#352=PLANE('',#15518);
#353=PLANE('',#15519);
#354=PLANE('',#15520);
#355=PLANE('',#15521);
#356=PLANE('',#15522);
#357=PLANE('',#15523);
#358=PLANE('',#15524);
#359=PLANE('',#15525);
#360=PLANE('',#15526);
#361=PLANE('',#15527);
#362=PLANE('',#15528);
#363=PLANE('',#15529);
#364=PLANE('',#15530);
#365=PLANE('',#15607);
#366=PLANE('',#15609);
#367=PLANE('',#15610);
#368=PLANE('',#15612);
#369=PLANE('',#15613);
#370=PLANE('',#15614);
#371=PLANE('',#15615);
#372=PLANE('',#15616);
#373=PLANE('',#15617);
#374=PLANE('',#15618);
#375=PLANE('',#15619);
#376=PLANE('',#15620);
#377=PLANE('',#15621);
#378=PLANE('',#15622);
#379=PLANE('',#15623);
#380=PLANE('',#15624);
#381=PLANE('',#15625);
#382=PLANE('',#15626);
#383=PLANE('',#15627);
#384=PLANE('',#15628);
#385=PLANE('',#15629);
#386=PLANE('',#15630);
#387=PLANE('',#15631);
#388=PLANE('',#15632);
#389=PLANE('',#15633);
#390=PLANE('',#15634);
#391=PLANE('',#15635);
#392=PLANE('',#15636);
#393=PLANE('',#15637);
#394=PLANE('',#15638);
#395=PLANE('',#15639);
#396=PLANE('',#15640);
#397=PLANE('',#15641);
#398=PLANE('',#15642);
#399=PLANE('',#15643);
#400=PLANE('',#15644);
#401=PLANE('',#15645);
#402=PLANE('',#15646);
#403=PLANE('',#15647);
#404=PLANE('',#15648);
#405=PLANE('',#15649);
#406=PLANE('',#15650);
#407=PLANE('',#15651);
#408=PLANE('',#15652);
#409=PLANE('',#15653);
#410=PLANE('',#15654);
#411=PLANE('',#15655);
#412=PLANE('',#15656);
#413=PLANE('',#15657);
#414=PLANE('',#15658);
#415=PLANE('',#15659);
#416=PLANE('',#15660);
#417=PLANE('',#15661);
#418=PLANE('',#15662);
#419=PLANE('',#15663);
#420=PLANE('',#15664);
#421=PLANE('',#15665);
#422=PLANE('',#15666);
#423=PLANE('',#15667);
#424=PLANE('',#15668);
#425=PLANE('',#15669);
#426=PLANE('',#15670);
#427=PLANE('',#15671);
#428=PLANE('',#15673);
#429=PLANE('',#15675);
#430=PLANE('',#15678);
#431=PLANE('',#15698);
#432=PLANE('',#15699);
#433=PLANE('',#15700);
#434=PLANE('',#15701);
#435=PLANE('',#15702);
#436=PLANE('',#15703);
#437=PLANE('',#15704);
#438=PLANE('',#15705);
#439=PLANE('',#15706);
#440=PLANE('',#15707);
#441=PLANE('',#15708);
#442=PLANE('',#15709);
#443=PLANE('',#15710);
#444=PLANE('',#15713);
#445=PLANE('',#15716);
#446=PLANE('',#15717);
#447=PLANE('',#15718);
#448=PLANE('',#15719);
#449=PLANE('',#15720);
#450=PLANE('',#15721);
#451=PLANE('',#15722);
#452=PLANE('',#15723);
#453=PLANE('',#15724);
#454=PLANE('',#15725);
#455=PLANE('',#15726);
#456=PLANE('',#15730);
#457=PLANE('',#15731);
#458=PLANE('',#15738);
#459=PLANE('',#15739);
#460=PLANE('',#15740);
#461=PLANE('',#15744);
#462=PLANE('',#15745);
#463=PLANE('',#15746);
#464=PLANE('',#15747);
#465=PLANE('',#15748);
#466=PLANE('',#15749);
#467=PLANE('',#15753);
#468=PLANE('',#15760);
#469=PLANE('',#15767);
#470=PLANE('',#15774);
#471=PLANE('',#15775);
#472=PLANE('',#15776);
#473=PLANE('',#15777);
#474=PLANE('',#15778);
#475=PLANE('',#15780);
#476=PLANE('',#15781);
#477=PLANE('',#15782);
#478=PLANE('',#15783);
#479=PLANE('',#15784);
#480=PLANE('',#15785);
#481=PLANE('',#15786);
#482=PLANE('',#15787);
#483=PLANE('',#15788);
#484=PLANE('',#15789);
#485=PLANE('',#15790);
#486=PLANE('',#15791);
#487=PLANE('',#15792);
#488=PLANE('',#15793);
#489=PLANE('',#15794);
#490=PLANE('',#15795);
#491=PLANE('',#15796);
#492=PLANE('',#15797);
#493=PLANE('',#15798);
#494=PLANE('',#15804);
#495=PLANE('',#15805);
#496=PLANE('',#15806);
#497=PLANE('',#15807);
#498=PLANE('',#15808);
#499=PLANE('',#15809);
#500=PLANE('',#15816);
#501=PLANE('',#15817);
#502=PLANE('',#15819);
#503=PLANE('',#15820);
#504=PLANE('',#15821);
#505=PLANE('',#15822);
#506=PLANE('',#15823);
#507=PLANE('',#15827);
#508=PLANE('',#15828);
#509=PLANE('',#15829);
#510=PLANE('',#15830);
#511=PLANE('',#15831);
#512=PLANE('',#15832);
#513=PLANE('',#15835);
#514=PLANE('',#15838);
#515=PLANE('',#15843);
#516=PLANE('',#15844);
#517=PLANE('',#15845);
#518=PLANE('',#15846);
#519=PLANE('',#15847);
#520=PLANE('',#15848);
#521=PLANE('',#15849);
#522=PLANE('',#15850);
#523=PLANE('',#15851);
#524=PLANE('',#15852);
#525=PLANE('',#15853);
#526=PLANE('',#15854);
#527=PLANE('',#15855);
#528=PLANE('',#15856);
#529=PLANE('',#15857);
#530=PLANE('',#15986);
#531=PLANE('',#15987);
#532=PLANE('',#15989);
#533=PLANE('',#15990);
#534=PLANE('',#15991);
#535=PLANE('',#15992);
#536=PLANE('',#15993);
#537=PLANE('',#15994);
#538=PLANE('',#15995);
#539=PLANE('',#16014);
#540=PLANE('',#16022);
#541=PLANE('',#16023);
#542=PLANE('',#16024);
#543=PLANE('',#16027);
#544=PLANE('',#16030);
#545=PLANE('',#16031);
#546=PLANE('',#16032);
#547=PLANE('',#16045);
#548=PLANE('',#16046);
#549=PLANE('',#16065);
#550=PLANE('',#16077);
#551=PLANE('',#16078);
#552=PLANE('',#16079);
#553=PLANE('',#16080);
#554=PLANE('',#16099);
#555=PLANE('',#16101);
#556=PLANE('',#16102);
#557=PLANE('',#16107);
#558=PLANE('',#16110);
#559=PLANE('',#16116);
#560=PLANE('',#16119);
#561=PLANE('',#16122);
#562=PLANE('',#16124);
#563=PLANE('',#16140);
#564=PLANE('',#16147);
#565=PLANE('',#16154);
#566=PLANE('',#16155);
#567=PLANE('',#16168);
#568=PLANE('',#16169);
#569=PLANE('',#16170);
#570=PLANE('',#16171);
#571=PLANE('',#16173);
#572=PLANE('',#16174);
#573=PLANE('',#16175);
#574=PLANE('',#16199);
#575=PLANE('',#16200);
#576=PLANE('',#16201);
#577=PLANE('',#16202);
#578=PLANE('',#16203);
#579=PLANE('',#16204);
#580=PLANE('',#16205);
#581=PLANE('',#16206);
#582=PLANE('',#16207);
#583=PLANE('',#16208);
#584=PLANE('',#16209);
#585=PLANE('',#16210);
#586=PLANE('',#16211);
#587=PLANE('',#16212);
#588=PLANE('',#16213);
#589=PLANE('',#16296);
#590=PLANE('',#16297);
#591=PLANE('',#16298);
#592=PLANE('',#16302);
#593=PLANE('',#16303);
#594=PLANE('',#16306);
#595=PLANE('',#16311);
#596=PLANE('',#16312);
#597=PLANE('',#16313);
#598=PLANE('',#16315);
#599=PLANE('',#16316);
#600=PLANE('',#16320);
#601=PLANE('',#16321);
#602=PLANE('',#16323);
#603=PLANE('',#16324);
#604=PLANE('',#16325);
#605=PLANE('',#16327);
#606=PLANE('',#16329);
#607=PLANE('',#16333);
#608=PLANE('',#16334);
#609=PLANE('',#16336);
#610=PLANE('',#16337);
#611=PLANE('',#16338);
#612=PLANE('',#16340);
#613=PLANE('',#16341);
#614=PLANE('',#16342);
#615=PLANE('',#16344);
#616=PLANE('',#16345);
#617=PLANE('',#16349);
#618=PLANE('',#16350);
#619=PLANE('',#16357);
#620=PLANE('',#16358);
#621=PLANE('',#16360);
#622=PLANE('',#16361);
#623=PLANE('',#16362);
#624=PLANE('',#16363);
#625=PLANE('',#16364);
#626=PLANE('',#16365);
#627=PLANE('',#16366);
#628=PLANE('',#16367);
#629=PLANE('',#16371);
#630=PLANE('',#16375);
#631=PLANE('',#16376);
#632=PLANE('',#16381);
#633=PLANE('',#16383);
#634=PLANE('',#16384);
#635=PLANE('',#16385);
#636=PLANE('',#16386);
#637=PLANE('',#16431);
#638=PLANE('',#16432);
#639=PLANE('',#16433);
#640=PLANE('',#16434);
#641=PLANE('',#16435);
#642=PLANE('',#16436);
#643=PLANE('',#16437);
#644=PLANE('',#16438);
#645=PLANE('',#16439);
#646=PLANE('',#16443);
#647=PLANE('',#16447);
#648=PLANE('',#16454);
#649=PLANE('',#16455);
#650=PLANE('',#16456);
#651=PLANE('',#16457);
#652=PLANE('',#16458);
#653=PLANE('',#16459);
#654=PLANE('',#16460);
#655=PLANE('',#16462);
#656=PLANE('',#16463);
#657=PLANE('',#16470);
#658=PLANE('',#16471);
#659=PLANE('',#16472);
#660=PLANE('',#16473);
#661=PLANE('',#16474);
#662=PLANE('',#16477);
#663=PLANE('',#16479);
#664=PLANE('',#16480);
#665=PLANE('',#16481);
#666=PLANE('',#16483);
#667=PLANE('',#16484);
#668=PLANE('',#16485);
#669=PLANE('',#16645);
#670=PLANE('',#16646);
#671=PLANE('',#16647);
#672=PLANE('',#16652);
#673=PLANE('',#16656);
#674=PLANE('',#16659);
#675=PLANE('',#16662);
#676=PLANE('',#16665);
#677=PLANE('',#16675);
#678=PLANE('',#16742);
#679=PLANE('',#16743);
#680=PLANE('',#16745);
#681=PLANE('',#16746);
#682=PLANE('',#16749);
#683=PLANE('',#16754);
#684=PLANE('',#16755);
#685=PLANE('',#16759);
#686=PLANE('',#16765);
#687=PLANE('',#16768);
#688=PLANE('',#16769);
#689=PLANE('',#16779);
#690=PLANE('',#16780);
#691=PLANE('',#16784);
#692=PLANE('',#16790);
#693=PLANE('',#16791);
#694=PLANE('',#16797);
#695=PLANE('',#16798);
#696=PLANE('',#16802);
#697=PLANE('',#16803);
#698=PLANE('',#16804);
#699=PLANE('',#16806);
#700=PLANE('',#16807);
#701=PLANE('',#16808);
#702=PLANE('',#16809);
#703=PLANE('',#16810);
#704=PLANE('',#16812);
#705=PLANE('',#16813);
#706=PLANE('',#16814);
#707=PLANE('',#16841);
#708=PLANE('',#16847);
#709=PLANE('',#16848);
#710=PLANE('',#16849);
#711=PLANE('',#16850);
#712=PLANE('',#16851);
#713=PLANE('',#16855);
#714=PLANE('',#16863);
#715=PLANE('',#16864);
#716=PLANE('',#16878);
#717=PLANE('',#16879);
#718=PLANE('',#16882);
#719=PLANE('',#16883);
#720=PLANE('',#16916);
#721=PLANE('',#16923);
#722=PLANE('',#16928);
#723=PLANE('',#16929);
#724=PLANE('',#16930);
#725=PLANE('',#16931);
#726=PLANE('',#16932);
#727=PLANE('',#16933);
#728=PLANE('',#16934);
#729=PLANE('',#16935);
#730=PLANE('',#16936);
#731=PLANE('',#16937);
#732=PLANE('',#16938);
#733=PLANE('',#16939);
#734=PLANE('',#16940);
#735=ELLIPSE('',#15361,7.42462120254335,5.25000000010882);
#736=ELLIPSE('',#15365,7.42462120245347,5.24999999999376);
#737=ELLIPSE('',#15371,7.42470893119486,5.25007996454306);
#738=ELLIPSE('',#15372,7.42470893118818,5.25007996453788);
#739=ELLIPSE('',#15532,14.9999999999992,14.4999999999993);
#740=ELLIPSE('',#15533,15.0000000000004,14.5000000000004);
#741=ELLIPSE('',#15534,14.9999999999913,14.4999999999828);
#742=ELLIPSE('',#15535,15.0000000000001,14.5000000000001);
#743=ELLIPSE('',#15536,15.,14.5);
#744=ELLIPSE('',#15537,14.9999999999864,14.4999999999732);
#745=ELLIPSE('',#15608,14.9999999999937,14.4999999999875);
#746=ELLIPSE('',#15611,15.0000000000065,14.5000000000128);
#747=ELLIPSE('',#15672,15.0000000000007,14.5000000000006);
#748=ELLIPSE('',#15674,15.0000000000004,14.5000000000003);
#749=ELLIPSE('',#15676,15.0000000000002,14.5000000000001);
#750=ELLIPSE('',#15677,15.0000000000002,14.5000000000002);
#751=ELLIPSE('',#15714,2.022122546197,0.800000000000197);
#752=ELLIPSE('',#15715,5.05530636499052,1.99999999968039);
#753=ELLIPSE('',#15815,5.0553063659433,2.00000000029026);
#754=ELLIPSE('',#15825,2.02212254619594,0.799999999999696);
#755=ELLIPSE('',#15926,24.0416305514422,16.9999999877997);
#756=ELLIPSE('',#15969,0.7071067812592,0.500000000027091);
#757=ELLIPSE('',#15970,0.70710678118732,0.500000000000854);
#758=ELLIPSE('',#16016,1.11803398875074,0.500000000000357);
#759=ELLIPSE('',#16018,1.41421601068422,1.0000094568796);
#760=ELLIPSE('',#16021,1.39479172867192,0.980946657426322);
#761=ELLIPSE('',#16038,0.707106781186665,0.500000000000195);
#762=ELLIPSE('',#16039,1.1180335450767,0.999997604635691);
#763=ELLIPSE('',#16043,1.11805148063465,0.999999766049803);
#764=ELLIPSE('',#16058,1.11803398875087,0.500000000000499);
#765=ELLIPSE('',#16082,1.11810288856955,0.500019557827469);
#766=ELLIPSE('',#16083,1.41330852530877,0.999058658412993);
#767=ELLIPSE('',#16084,1.41330395373969,0.999062064731566);
#768=ELLIPSE('',#16145,0.541196100146381,0.500000000000179);
#769=ELLIPSE('',#16150,0.707106781202788,0.50000000002241);
#770=ELLIPSE('',#16490,0.787132929614446,0.490404666125977);
#771=ELLIPSE('',#16525,11.474561377534,5.80198696989729);
#772=ELLIPSE('',#16570,0.707106781186205,0.500000000000487);
#773=ELLIPSE('',#16578,7.07106781186394,4.99999999999909);
#774=ELLIPSE('',#16581,7.07106781196844,5.00000000004573);
#775=ELLIPSE('',#16584,2.82842712474406,1.99999999999928);
#776=ELLIPSE('',#16607,0.707106781180475,0.49999999999776);
#777=ELLIPSE('',#16694,0.65489735345099,0.499999999998802);
#778=ELLIPSE('',#16701,0.654897353451537,0.499999999999167);
#779=ELLIPSE('',#16706,0.93246545981575,0.499999999999451);
#780=ELLIPSE('',#16708,0.570504795854994,0.499999999999747);
#781=ELLIPSE('',#16729,0.520708654805954,0.500000000000599);
#782=ELLIPSE('',#16741,0.707106781185331,0.499999999999033);
#783=ELLIPSE('',#16748,1.30979470690588,1.00000000000042);
#784=ELLIPSE('',#16751,1.06587697723058,0.998342579493648);
#785=ELLIPSE('',#16756,7.07106781178892,4.99999999996606);
#786=ELLIPSE('',#16758,7.07106781478535,5.00000000116881);
#787=ELLIPSE('',#16766,1.02590924137892,0.995770746428315);
#788=ELLIPSE('',#16782,0.707106781186607,0.499999999999867);
#789=ELLIPSE('',#16788,0.501870829776834,0.499498521952907);
#790=ELLIPSE('',#16789,0.501871930366977,0.4994982286229);
#791=ELLIPSE('',#16793,0.80842845737287,0.499999999999691);
#792=ELLIPSE('',#16796,1.18473126058658,1.00000495319552);
#793=ELLIPSE('',#16831,1.30979470690618,1.00000000000064);
#794=ELLIPSE('',#16852,8.39218913835177,4.49999999999994);
#795=B_SPLINE_CURVE_WITH_KNOTS('',3,(#21423,#21424,#21425,#21426,#21427,
#21428,#21429,#21430,#21431,#21432,#21433,#21434,#21435,#21436,#21437,#21438,
#21439,#21440,#21441,#21442,#21443,#21444),.UNSPECIFIED.,.F.,.F.,(4,2,2,
2,2,2,2,2,2,2,4),(-3.36585159579603,-3.23154274939443,-3.10218229476243,
-2.97282184013043,-2.86647922856163,-2.76013661699283,-2.65379400542402,
-2.54745139385522,-2.41809093922322,-2.28873048459122,-2.15442163818962),
 .UNSPECIFIED.);
#796=B_SPLINE_CURVE_WITH_KNOTS('',3,(#27646,#27647,#27648,#27649,#27650,
#27651,#27652,#27653,#27654,#27655,#27656,#27657,#27658,#27659,#27660,#27661,
#27662,#27663,#27664,#27665,#27666,#27667,#27668,#27669,#27670,#27671,#27672,
#27673,#27674,#27675,#27676,#27677,#27678,#27679,#27680,#27681,#27682,#27683,
#27684,#27685,#27686,#27687,#27688,#27689,#27690,#27691,#27692,#27693,#27694,
#27695,#27696,#27697,#27698,#27699,#27700,#27701,#27702,#27703,#27704,#27705,
#27706,#27707,#27708,#27709,#27710,#27711,#27712,#27713,#27714,#27715,#27716,
#27717,#27718,#27719,#27720,#27721,#27722,#27723,#27724,#27725,#27726,#27727,
#27728,#27729,#27730,#27731,#27732,#27733,#27734,#27735,#27736,#27737,#27738,
#27739,#27740,#27741,#27742,#27743,#27744,#27745,#27746,#27747,#27748,#27749,
#27750,#27751,#27752,#27753,#27754,#27755,#27756,#27757,#27758,#27759,#27760,
#27761,#27762,#27763,#27764,#27765,#27766),.UNSPECIFIED.,.F.,.F.,(4,3,3,
3,3,3,3,3,3,3,3,3,3,3,3,3,3,3,3,3,3,3,3,3,3,3,3,3,3,3,3,3,3,3,3,3,3,3,3,
3,4),(-0.00524423961119122,-0.00523399695570063,-0.00523143629190568,-0.00523015596002173,
-0.00522887562795533,-0.00522375430021003,-0.00520326898922881,-0.00518278367839879,
-0.00516229836726638,-0.00514181305643454,-0.00512132774545271,-0.00510084243447086,
-0.00508035712334152,-0.00503938650152429,-0.00499841587941665,-0.00495744525759613,
-0.00491647463549179,-0.00487550401366842,-0.00483453339170461,-0.00475259214764206,
-0.00467065090384962,-0.00458870965979234,-0.00450676841599483,-0.00442482717194261,
-0.00434288592814021,-0.00426094468409288,-0.00409706219635843,-0.00393317970839343,
-0.00376929722064964,-0.00360541473269398,-0.00344153224494097,-0.00327764975699452,
-0.00294988478137813,-0.00262211980559562,-0.0022943548299611,-0.00196658985425258,
-0.00163882487854402,-0.00131105990279781,-0.000983294927126725,-0.000655529951398905,
0.),.UNSPECIFIED.);
#797=B_SPLINE_CURVE_WITH_KNOTS('',3,(#33721,#33722,#33723,#33724,#33725,
#33726,#33727,#33728,#33729,#33730,#33731,#33732,#33733,#33734,#33735,#33736,
#33737,#33738,#33739,#33740,#33741,#33742,#33743,#33744,#33745,#33746,#33747,
#33748,#33749,#33750,#33751,#33752,#33753,#33754,#33755,#33756,#33757,#33758,
#33759,#33760,#33761,#33762,#33763,#33764,#33765,#33766,#33767,#33768,#33769,
#33770,#33771,#33772,#33773,#33774,#33775,#33776,#33777,#33778,#33779,#33780,
#33781,#33782,#33783,#33784,#33785,#33786,#33787,#33788,#33789,#33790,#33791,
#33792,#33793,#33794,#33795,#33796,#33797,#33798,#33799,#33800,#33801,#33802,
#33803,#33804,#33805,#33806,#33807,#33808,#33809,#33810,#33811,#33812,#33813,
#33814,#33815,#33816,#33817,#33818,#33819,#33820,#33821,#33822,#33823,#33824,
#33825,#33826,#33827,#33828,#33829,#33830,#33831,#33832,#33833,#33834,#33835,
#33836,#33837,#33838,#33839,#33840,#33841),.UNSPECIFIED.,.F.,.F.,(4,3,3,
3,3,3,3,3,3,3,3,3,3,3,3,3,3,3,3,3,3,3,3,3,3,3,3,3,3,3,3,3,3,3,3,3,3,3,3,
3,4),(0.,0.000655529951398911,0.000983294927092821,0.00131105990279782,
0.00163882487848811,0.0019665898541858,0.00229435482988349,0.00262211980559564,
0.00294988478127885,0.00327764975699456,0.00344153224482537,0.00360541473269401,
0.00376929722052302,0.00393317970839347,0.00409706219622063,0.00426094468409292,
0.00434288592799383,0.00442482717194265,0.0045067684158426,0.00458870965979238,
0.00467065090369136,0.00475259214764211,0.00483453339154007,0.00487550401350222,
0.00491647463549184,0.00495744525742651,0.0049984158794167,0.00503938650135109,
0.00508035712334157,0.00510084243429463,0.00512132774527543,0.00514181305625618,
0.00516229836726643,0.00518278367821808,0.00520326898922886,0.00522375430021008,
0.00522887562795538,0.00523015595986631,0.00523143629181281,0.00523399695570069,
0.0052442396111913),.UNSPECIFIED.);
#798=B_SPLINE_CURVE_WITH_KNOTS('',3,(#35181,#35182,#35183,#35184,#35185,
#35186,#35187,#35188,#35189,#35190,#35191,#35192,#35193,#35194,#35195,#35196),
 .UNSPECIFIED.,.F.,.F.,(4,2,2,2,2,2,2,4),(0.559306717359078,0.626396965369611,
0.735567235927107,0.809225982698514,0.832702121898874,0.841751773808283,
0.84754287435266,0.849323156359136),.UNSPECIFIED.);
#799=B_SPLINE_CURVE_WITH_KNOTS('',3,(#35198,#35199,#35200,#35201,#35202,
#35203,#35204,#35205,#35206,#35207,#35208,#35209,#35210,#35211,#35212,#35213,
#35214,#35215,#35216,#35217,#35218,#35219,#35220,#35221,#35222,#35223,#35224,
#35225),.UNSPECIFIED.,.F.,.F.,(4,2,2,1,1,1,2,2,2,1,1,1,2,2,1,1,1,1,4),(0.0040855928878666,
0.00415787795859431,0.00417749059047448,0.00419710322235465,0.004236328486115,
0.00431477901363569,0.00439322954115639,0.00443245480491673,0.00445206743679691,
0.00447168006867708,0.00455013059619778,0.00462858112371847,0.00470703165123916,
0.00472664428311934,0.00474625691499952,0.00478548217875988,0.00486393270628059,
0.0049423832338013,0.00499039171021971),.UNSPECIFIED.);
#800=B_SPLINE_CURVE_WITH_KNOTS('',3,(#35227,#35228,#35229,#35230,#35231,
#35232,#35233,#35234,#35235,#35236,#35237,#35238,#35239,#35240,#35241,#35242,
#35243,#35244,#35245,#35246,#35247,#35248,#35249,#35250,#35251,#35252,#35253,
#35254,#35255,#35256,#35257,#35258,#35259,#35260,#35261,#35262,#35263,#35264),
 .UNSPECIFIED.,.F.,.F.,(4,2,1,1,2,2,1,1,1,2,2,2,1,1,2,1,2,2,1,1,2,2,1,1,
4),(0.00499039171021971,0.00502083376132202,0.00509928428884266,0.0051777348163633,
0.00525618534388394,0.0052757979757641,0.00529541060764426,0.00533463587140458,
0.00541308639892522,0.00549153692644585,0.00551114955832601,0.00553076219020616,
0.00556998745396648,0.00564843798148711,0.00572688850900774,0.00576611377276805,
0.00578572640464821,0.00580533903652836,0.005883789564049,0.00596224009156964,
0.00604069061909029,0.0060799158828506,0.00611914114661092,0.00619759167413156,
0.00623984937653201),.UNSPECIFIED.);
#801=B_SPLINE_CURVE_WITH_KNOTS('',3,(#35266,#35267,#35268,#35269,#35270,
#35271,#35272,#35273,#35274,#35275,#35276,#35277,#35278,#35279,#35280,#35281,
#35282,#35283,#35284,#35285,#35286,#35287,#35288,#35289,#35290,#35291,#35292,
#35293,#35294,#35295,#35296,#35297,#35298,#35299,#35300,#35301,#35302,#35303,
#35304,#35305,#35306,#35307),.UNSPECIFIED.,.F.,.F.,(4,2,2,2,1,1,1,2,2,1,
1,1,2,2,2,1,1,1,2,2,1,1,1,2,2,2,4),(0.00121901561520999,0.00125520844033018,
0.0012944337040905,0.00131404633597066,0.00133365896785082,0.00141210949537145,
0.00149056002289208,0.00156901055041272,0.00158862318229288,0.00160823581417303,
0.00164746107793335,0.00172591160545398,0.00180436213297462,0.00184358739673493,
0.00186320002861509,0.00188281266049525,0.00196126318801588,0.00203971371553651,
0.00211816424305713,0.00213777687493729,0.00215738950681745,0.00219661477057776,
0.00227506529809839,0.00235351582561902,0.00239274108937934,0.00243196635313965,
0.0024802465217231),.UNSPECIFIED.);
#802=B_SPLINE_CURVE_WITH_KNOTS('',3,(#35309,#35310,#35311,#35312,#35313,
#35314,#35315,#35316,#35317,#35318,#35319,#35320,#35321,#35322,#35323,#35324,
#35325,#35326,#35327,#35328,#35329,#35330,#35331,#35332,#35333,#35334,#35335,
#35336,#35337,#35338,#35339,#35340,#35341),.UNSPECIFIED.,.F.,.F.,(4,2,2,
2,1,1,1,2,2,1,1,1,2,2,2,1,1,2,1,2,4),(0.0024802465217231,0.0025104168806603,
0.00254964214442063,0.0025692547763008,0.00258886740818097,0.00266731793570164,
0.00274576846322231,0.00282421899074298,0.00284383162262314,0.00286344425450331,
0.00290266951826364,0.0029811200457843,0.00305957057330496,0.00309879583706529,
0.00311840846894545,0.00313802110082561,0.00321647162834627,0.00329492215586693,
0.00333414741962726,0.00335376005150743,0.00337185540595827),
 .UNSPECIFIED.);
#803=B_SPLINE_CURVE_WITH_KNOTS('',3,(#35342,#35343,#35344,#35345,#35346,
#35347,#35348,#35349,#35350,#35351,#35352,#35353,#35354,#35355,#35356,#35357,
#35358,#35359,#35360),.UNSPECIFIED.,.F.,.F.,(4,2,2,2,2,2,2,3,4),(0.849323156359136,
0.852552467217484,0.858257321208267,0.867642993968765,0.889066342099187,
0.954635992312572,1.05821450691892,1.11775317676601,1.12218737820187),
 .UNSPECIFIED.);
#804=B_SPLINE_CURVE_WITH_KNOTS('',3,(#35370,#35371,#35372,#35373,#35374,
#35375,#35376,#35377,#35378,#35379,#35380,#35381,#35382,#35383,#35384,#35385,
#35386,#35387,#35388,#35389,#35390,#35391,#35392,#35393,#35394,#35395,#35396,
#35397,#35398,#35399,#35400,#35401,#35402,#35403,#35404,#35405,#35406,#35407,
#35408,#35409,#35410,#35411,#35412),.UNSPECIFIED.,.F.,.F.,(4,1,1,2,2,1,
1,1,2,2,2,1,1,1,2,2,1,1,1,2,2,2,1,2,2,2,1,4),(0.00133762907826533,0.00141171783679417,
0.00149014660550492,0.00156857537421566,0.00158818256639335,0.00160778975857103,
0.00164700414292642,0.0017254329116372,0.00180386168034798,0.00184307606470337,
0.00186268325688106,0.00188229044905876,0.00196071921776951,0.00203914798648025,
0.002117576755191,0.00213718394736868,0.00215679113954637,0.00219600552390173,
0.00227443429261245,0.00235286306132317,0.00239207744567853,0.00243129183003388,
0.00250972059874461,0.00258814936745533,0.0026273637518107,0.00266657813616607,
0.00274500690487681,0.00274775444653194),.UNSPECIFIED.);
#805=B_SPLINE_CURVE_WITH_KNOTS('',3,(#35414,#35415,#35416,#35417,#35418,
#35419,#35420,#35421,#35422,#35423,#35424,#35425,#35426,#35427,#35428,#35429,
#35430,#35431,#35432,#35433,#35434,#35435,#35436,#35437,#35438,#35439,#35440,
#35441,#35442,#35443,#35444,#35445,#35446,#35447,#35448,#35449,#35450),
 .UNSPECIFIED.,.F.,.F.,(4,2,2,1,1,1,2,2,2,1,2,1,2,2,1,1,2,2,2,1,1,2,4),
(0.00274775444653194,0.00282343567358756,0.00284304286576525,0.00286265005794293,
0.00290186444229832,0.00298029321100909,0.00305872197971986,0.00309793636407524,
0.00313715074843063,0.00321557951714139,0.00329400828585215,0.00333322267020754,
0.00335282986238522,0.00337243705456291,0.00345086582327365,0.0035292945919844,
0.00360772336069514,0.00362733055287283,0.00364693774505051,0.00368615212940588,
0.00376458089811663,0.00384300966682737,0.00384768372848343),
 .UNSPECIFIED.);
#806=B_SPLINE_CURVE_WITH_KNOTS('',3,(#35452,#35453,#35454,#35455,#35456,
#35457,#35458,#35459,#35460,#35461,#35462,#35463,#35464,#35465,#35466,#35467,
#35468,#35469,#35470,#35471,#35472,#35473,#35474,#35475,#35476,#35477,#35478,
#35479,#35480,#35481,#35482,#35483,#35484,#35485,#35486,#35487,#35488,#35489,
#35490,#35491,#35492,#35493,#35494,#35495,#35496),.UNSPECIFIED.,.F.,.F.,
(4,2,2,1,1,2,2,1,1,1,2,2,2,1,1,1,2,2,1,1,1,2,2,2,2,1,1,2,4),(0.00384768372848343,
0.00388222405118274,0.00392143843553811,0.00399986720424885,0.0040782959729596,
0.00415672474167034,0.00417633193384803,0.00419593912602572,0.0042351535103811,
0.00431358227909184,0.00439201104780258,0.00443122543215796,0.00445083262433565,
0.00447043981651334,0.0045488685852241,0.00462729735393486,0.00470572612264562,
0.00472533331482332,0.00474494050700101,0.00478415489135639,0.00486258366006715,
0.0049410124287779,0.00498022681313327,0.00499983400531096,0.00501944119748865,
0.00509786996619946,0.00517629873491028,0.0052547275036211,0.00525766866554466),
 .UNSPECIFIED.);
#807=B_SPLINE_CURVE_WITH_KNOTS('',3,(#35497,#35498,#35499,#35500,#35501,
#35502,#35503,#35504,#35505,#35506,#35507,#35508,#35509,#35510,#35511,#35512,
#35513,#35514,#35515,#35516,#35517,#35518,#35519,#35520,#35521,#35522,#35523,
#35524,#35525,#35526,#35527,#35528,#35529,#35530,#35531,#35532,#35533,#35534,
#35535,#35536,#35537),.UNSPECIFIED.,.F.,.F.,(4,2,1,1,1,2,2,2,1,1,2,1,2,
2,1,1,2,2,2,1,1,2,2,2,1,4),(0.000238227468056005,0.00025489349831015,0.000274500690487856,
0.000313715074843255,0.000392143843554055,0.000470572612264855,0.000509786996620253,
0.000529394188797954,0.000549001380975655,0.000627430149686458,0.000705858918397262,
0.00074507330275266,0.000764680494930355,0.000784287687108051,0.000862716455818834,
0.000941145224529618,0.0010195739932404,0.00103918118541809,0.00105878837759578,
0.00109800276195116,0.00117643153066191,0.00125486029937267,0.00129407468372805,
0.00131368187590574,0.00133328906808343,0.00133762907826533),
 .UNSPECIFIED.);
#808=B_SPLINE_CURVE_WITH_KNOTS('',3,(#35579,#35580,#35581,#35582,#35583,
#35584,#35585,#35586,#35587,#35588,#35589,#35590),.UNSPECIFIED.,.F.,.F.,
(4,2,2,2,2,4),(-0.479639825472432,-0.462425217556728,-0.422203417432446,
-0.38131877878649,-0.344677987741986,-0.318946577997265),.UNSPECIFIED.);
#809=B_SPLINE_CURVE_WITH_KNOTS('',3,(#35594,#35595,#35596,#35597,#35598,
#35599,#35600,#35601,#35602,#35603,#35604,#35605),.UNSPECIFIED.,.F.,.F.,
(4,2,2,2,2,4),(-0.318946577997265,-0.30962423887292,-0.272340183092938,
-0.230649804158065,-0.19116895139264,-0.158267505542008),.UNSPECIFIED.);
#810=B_SPLINE_CURVE_WITH_KNOTS('',3,(#35626,#35627,#35628,#35629,#35630,
#35631,#35632,#35633,#35634,#35635,#35636,#35637,#35638,#35639,#35640,#35641,
#35642,#35643),.UNSPECIFIED.,.F.,.F.,(4,2,2,2,2,2,2,2,4),(0.191281861861795,
0.215459032327926,0.239636202794058,0.259584872085487,0.279533541376917,
0.299482210668346,0.319430879959776,0.343608050425907,0.367785220892039),
 .UNSPECIFIED.);
#811=B_SPLINE_CURVE_WITH_KNOTS('',3,(#35649,#35650,#35651,#35652,#35653,
#35654,#35655,#35656,#35657,#35658,#35659,#35660,#35661,#35662,#35663,#35664,
#35665,#35666,#35667,#35668,#35669,#35670,#35671,#35672,#35673,#35674,#35675,
#35676,#35677),.UNSPECIFIED.,.F.,.F.,(4,2,2,2,2,2,2,2,1,2,2,2,1,1,2,4),
(6.50521303491303E-19,0.000157845345348291,0.000315690690696581,0.000473536036044871,
0.000552458708719019,0.000631381381393167,0.000789226726741468,0.000947072072089769,
0.00110491741743807,0.00126276276278637,0.00134168543546052,0.00142060810813467,
0.00157845345348297,0.00173629879883127,0.00189414414417957,0.00200452207066376),
 .UNSPECIFIED.);
#812=B_SPLINE_CURVE_WITH_KNOTS('',3,(#35679,#35680,#35681,#35682,#35683,
#35684,#35685,#35686,#35687,#35688,#35689,#35690,#35691,#35692,#35693,#35694,
#35695,#35696,#35697,#35698,#35699,#35700,#35701,#35702,#35703,#35704,#35705,
#35706,#35707,#35708,#35709,#35710,#35711,#35712,#35713,#35714,#35715),
 .UNSPECIFIED.,.F.,.F.,(4,3,3,3,3,3,3,3,3,3,3,3,4),(0.00200452207066376,
0.00220435629196357,0.00220983483487617,0.00236485788351544,0.00236768018022447,
0.0024451673964532,0.00244660285289862,0.00248533519715336,0.00248606418923569,
0.00250542216027589,0.00250579485740423,0.00251566019148849,0.00252552552557276),
 .UNSPECIFIED.);
#813=B_SPLINE_CURVE_WITH_KNOTS('',3,(#35721,#35722,#35723,#35724,#35725,
#35726),.UNSPECIFIED.,.F.,.F.,(4,2,4),(0.349196728876737,0.42160526861445,
0.509180501662979),.UNSPECIFIED.);
#814=B_SPLINE_CURVE_WITH_KNOTS('',3,(#35730,#35731,#35732,#35733,#35734,
#35735,#35736,#35737,#35738,#35739,#35740,#35741,#35742,#35743,#35744,#35745,
#35746,#35747,#35748,#35749,#35750,#35751,#35752,#35753,#35754,#35755,#35756,
#35757,#35758,#35759,#35760,#35761),.UNSPECIFIED.,.F.,.F.,(4,2,2,2,2,2,
2,2,2,2,2,2,2,2,2,4),(7.16841165822491E-9,0.00425984757262436,0.00882897338789379,
0.0181258595954712,0.0305987420002868,0.0373352764230015,0.0407040742822413,
0.0431630789194017,0.043233331588091,0.0457202883506083,0.0491738834305336,
0.055954122831043,0.0681757856187753,0.0771431840484888,0.0815121266890984,
0.0855915470562766),.UNSPECIFIED.);
#815=B_SPLINE_CURVE_WITH_KNOTS('',3,(#35771,#35772,#35773,#35774,#35775,
#35776,#35777,#35778,#35779,#35780,#35781,#35782,#35783,#35784),
 .UNSPECIFIED.,.F.,.F.,(4,2,2,2,2,2,4),(-0.0980600308872719,-0.0842479162203947,
-0.0683859734106203,-0.0469108894184264,-0.0242175938214273,0.,0.000471941323681861),
 .UNSPECIFIED.);
#816=B_SPLINE_CURVE_WITH_KNOTS('',3,(#35787,#35788,#35789,#35790,#35791,
#35792,#35793,#35794,#35795,#35796,#35797,#35798,#35799,#35800),
 .UNSPECIFIED.,.F.,.F.,(4,2,2,2,2,2,4),(-0.196928117070007,-0.196454849983009,
-0.172108534559874,-0.149310110641706,-0.127840368210239,-0.112006418277474,
-0.0982274249914714),.UNSPECIFIED.);
#817=B_SPLINE_CURVE_WITH_KNOTS('',3,(#35806,#35807,#35808,#35809,#35810,
#35811,#35812,#35813,#35814,#35815,#35816,#35817,#35818,#35819),
 .UNSPECIFIED.,.F.,.F.,(4,2,2,2,2,2,4),(0.101628267880583,0.107985189525145,
0.12609609523943,0.147834637699368,0.176750861538421,0.211678254053418,
0.212173672568657),.UNSPECIFIED.);
#818=B_SPLINE_CURVE_WITH_KNOTS('',3,(#35822,#35823,#35824,#35825,#35826,
#35827,#35828,#35829,#35830,#35831,#35832,#35833,#35834,#35835),
 .UNSPECIFIED.,.F.,.F.,(4,2,2,2,2,2,4),(-0.000412787679576289,0.,0.028368264114848,
0.0526479899563425,0.0709415556712408,0.0861626427766698,0.0917971386711219),
 .UNSPECIFIED.);
#819=B_SPLINE_CURVE_WITH_KNOTS('',3,(#35849,#35850,#35851,#35852,#35853,
#35854,#35855,#35856,#35857,#35858,#35859,#35860,#35861,#35862,#35863,#35864,
#35865,#35866,#35867,#35868,#35869,#35870,#35871,#35872,#35873,#35874,#35875,
#35876,#35877,#35878,#35879,#35880,#35881,#35882,#35883,#35884,#35885,#35886,
#35887,#35888,#35889,#35890,#35891,#35892,#35893,#35894,#35895,#35896,#35897,
#35898,#35899,#35900,#35901,#35902,#35903,#35904,#35905,#35906,#35907,#35908,
#35909,#35910,#35911,#35912,#35913,#35914,#35915,#35916,#35917,#35918,#35919,
#35920,#35921,#35922,#35923,#35924,#35925,#35926,#35927,#35928,#35929,#35930),
 .UNSPECIFIED.,.F.,.F.,(4,3,3,3,3,3,3,3,3,3,3,3,3,3,3,3,3,3,3,3,3,3,3,3,
3,3,3,4),(0.,5.46238072139918E-5,5.46768793257778E-5,0.000109353758651556,
0.000109437314960514,0.000218707517303111,0.000219131968308402,0.000328755035108541,
0.000437415034606219,0.000438315027410997,0.000656122551909328,0.000657273966688997,
0.000874830069212436,0.000876055977850079,0.00109353758651554,0.00109465839290278,
0.00131224510381865,0.0013130925134312,0.00153095262112176,0.00153141677949933,
0.00164030637977332,0.00164055507316062,0.00169498325909909,0.00169512122666045,
0.00172232169876198,0.00173599091859343,0.00174282552850915,0.00174966013842488),
 .UNSPECIFIED.);
#820=B_SPLINE_CURVE_WITH_KNOTS('',3,(#35932,#35933,#35934,#35935,#35936,
#35937,#35938,#35939,#35940,#35941,#35942,#35943,#35944,#35945,#35946,#35947,
#35948,#35949,#35950,#35951,#35952,#35953,#35954,#35955,#35956,#35957,#35958,
#35959,#35960,#35961,#35962,#35963,#35964,#35965,#35966,#35967,#35968,#35969,
#35970,#35971,#35972,#35973,#35974,#35975,#35976,#35977,#35978,#35979,#35980,
#35981,#35982,#35983,#35984,#35985,#35986,#35987,#35988,#35989,#35990,#35991,
#35992,#35993,#35994,#35995,#35996,#35997,#35998,#35999,#36000,#36001,#36002,
#36003,#36004,#36005,#36006,#36007,#36008,#36009,#36010,#36011,#36012,#36013),
 .UNSPECIFIED.,.F.,.F.,(4,3,3,3,3,3,3,3,3,3,3,3,3,3,3,3,3,3,3,3,3,3,3,3,
3,3,3,4),(-0.00174966013842491,-0.00174282552850919,-0.00173599091859347,
-0.00172232169876202,-0.00169512122666047,-0.00169498325909913,-0.00164055507316067,
-0.00164030637977336,-0.00153141677949938,-0.0015309526211218,-0.00131309251343127,
-0.00131224510381869,-0.00109465839290291,-0.00109353758651557,-0.000876055977850256,
-0.000874830069212459,-0.000657273966689205,-0.000656122551909345,-0.000438315027411205,
-0.000437415034606232,-0.000328755035108803,-0.000219131968308682,-0.000218707517303118,
-0.000109437314960775,-0.000109353758651561,-5.46768793257806E-5,-5.46238072142483E-5,
0.),.UNSPECIFIED.);
#821=B_SPLINE_CURVE_WITH_KNOTS('',3,(#36017,#36018,#36019,#36020,#36021,
#36022,#36023,#36024,#36025,#36026,#36027,#36028,#36029,#36030,#36031,#36032,
#36033,#36034,#36035,#36036,#36037,#36038,#36039,#36040,#36041,#36042,#36043,
#36044,#36045,#36046,#36047,#36048,#36049,#36050,#36051,#36052,#36053,#36054,
#36055,#36056),.UNSPECIFIED.,.F.,.F.,(4,3,3,3,3,3,3,3,3,3,3,3,3,4),(-0.00117485636691483,
-0.00113814210544875,-0.00110142784398266,-0.00102799932105048,-0.000881142275186127,
-0.000734285229321772,-0.000587428183457417,-0.000440571137593065,-0.000367142614660889,
-0.0003304283531948,-0.000293714091728711,-0.000146857045864357,-7.34285229321804E-5,
-3.03576608295941E-18),.UNSPECIFIED.);
#822=B_SPLINE_CURVE_WITH_KNOTS('',3,(#36062,#36063,#36064,#36065,#36066,
#36067,#36068,#36069,#36070,#36071),.UNSPECIFIED.,.F.,.F.,(4,2,2,2,4),(1.53451257034264E-7,
0.029053924592895,0.0610074471336537,0.12119991311449,0.121660810563458),
 .UNSPECIFIED.);
#823=B_SPLINE_CURVE_WITH_KNOTS('',3,(#36083,#36084,#36085,#36086,#36087,
#36088,#36089,#36090,#36091,#36092,#36093,#36094,#36095,#36096,#36097,#36098,
#36099,#36100),.UNSPECIFIED.,.F.,.F.,(4,2,2,2,2,2,2,2,4),(0.,0.0183029863676503,
0.0369119205731603,0.0559574729187805,0.0754931586326105,0.0951574217307725,
0.114505006447861,0.133267605428501,0.151453893017012),.UNSPECIFIED.);
#824=B_SPLINE_CURVE_WITH_KNOTS('',3,(#36104,#36105,#36106,#36107,#36108,
#36109,#36110,#36111,#36112,#36113,#36114,#36115,#36116,#36117),
 .UNSPECIFIED.,.F.,.F.,(4,2,2,2,2,2,4),(-0.000435818162108814,0.,0.0202992281610604,
0.039554052242145,0.0609562628819672,0.0778728931374231,0.0930628095475932),
 .UNSPECIFIED.);
#825=B_SPLINE_CURVE_WITH_KNOTS('',3,(#36122,#36123,#36124,#36125,#36126,
#36127,#36128,#36129,#36130,#36131,#36132,#36133),.UNSPECIFIED.,.F.,.F.,
(4,2,2,2,2,4),(0.142068886233636,0.167609243368551,0.19603253462721,0.222593243513583,
0.249806989712963,0.263543332734459),.UNSPECIFIED.);
#826=B_SPLINE_CURVE_WITH_KNOTS('',3,(#36161,#36162,#36163,#36164,#36165,
#36166,#36167,#36168,#36169,#36170,#36171,#36172,#36173,#36174,#36175,#36176,
#36177,#36178,#36179,#36180,#36181,#36182,#36183,#36184,#36185,#36186,#36187,
#36188,#36189,#36190,#36191,#36192,#36193,#36194,#36195,#36196,#36197,#36198,
#36199,#36200,#36201,#36202,#36203,#36204,#36205,#36206,#36207,#36208,#36209,
#36210,#36211,#36212,#36213,#36214,#36215,#36216,#36217,#36218,#36219,#36220,
#36221,#36222,#36223,#36224,#36225,#36226,#36227,#36228,#36229,#36230,#36231,
#36232,#36233,#36234,#36235,#36236,#36237,#36238,#36239,#36240,#36241,#36242,
#36243,#36244,#36245,#36246,#36247,#36248,#36249,#36250,#36251,#36252,#36253,
#36254,#36255,#36256,#36257,#36258,#36259,#36260,#36261,#36262,#36263,#36264,
#36265,#36266,#36267,#36268,#36269,#36270,#36271,#36272,#36273,#36274,#36275,
#36276,#36277,#36278,#36279,#36280,#36281,#36282,#36283,#36284,#36285,#36286,
#36287,#36288,#36289,#36290,#36291,#36292,#36293,#36294,#36295,#36296,#36297,
#36298,#36299,#36300,#36301,#36302,#36303,#36304,#36305,#36306,#36307,#36308,
#36309,#36310,#36311,#36312,#36313,#36314,#36315,#36316,#36317,#36318,#36319,
#36320,#36321,#36322,#36323,#36324,#36325,#36326,#36327,#36328,#36329,#36330,
#36331,#36332,#36333,#36334,#36335,#36336,#36337,#36338,#36339,#36340,#36341,
#36342,#36343,#36344),.UNSPECIFIED.,.F.,.F.,(4,3,3,3,3,3,3,3,3,3,3,3,3,
3,3,3,3,3,3,3,3,3,3,3,3,3,3,3,3,3,3,3,3,3,3,3,3,3,3,3,3,3,3,3,3,3,3,3,3,
3,3,3,3,3,3,3,3,3,3,3,3,4),(0.,0.000128793534426601,0.00013962725990874,
0.000201016480722258,0.000209440889863109,0.000237434536323755,0.000244347704840294,
0.000261801112328888,0.000274052527794055,0.000279254519817482,0.00041888177972623,
0.000421647685873793,0.000453788594703417,0.00045883099046583,0.000471242002192011,
0.000488695409680604,0.000496118975663363,0.000558509039634977,0.000570636153253297,
0.000698136299543724,0.000719219607406552,0.00073304311452091,0.000737751289965753,
0.000756269271015657,0.000767949929498096,0.000793191569626417,0.000837763559452467,
0.000866553502704528,0.000939320971633026,0.000975498896073627,0.00097739081936121,
0.000994844226849804,0.00101154198603956,0.0010122976343384,0.00104720444931558,
0.00111701807926996,0.00115415716089184,0.00125664533917869,0.00129450416296831,
0.00132645896913306,0.00132927157967002,0.00136136578411025,0.00136391871428646,
0.00139627259908743,0.00143289627153442,0.00153589985899619,0.00156968013137839,
0.00167552711890494,0.00170498962299591,0.00174534074885932,0.00177210055146248,
0.00178024756383651,0.00180552305617786,0.0018151543788137,0.00183887693334027,
0.00195478163872244,0.00197157657898437,0.00209440889863119,0.00210313115169305,
0.00212931571360838,0.00216422252858556,0.00223403615853994),
 .UNSPECIFIED.);
#827=B_SPLINE_CURVE_WITH_KNOTS('',3,(#36372,#36373,#36374,#36375,#36376,
#36377,#36378,#36379),.UNSPECIFIED.,.F.,.F.,(4,2,2,4),(-0.000445639589289738,
2.41755400420818E-15,0.0218391627722744,0.0289287082360094),
 .UNSPECIFIED.);
#828=B_SPLINE_CURVE_WITH_KNOTS('',3,(#36380,#36381,#36382,#36383,#36384,
#36385,#36386,#36387,#36388,#36389),.UNSPECIFIED.,.F.,.F.,(4,2,2,2,4),(0.411799298598375,
0.425924242071472,0.471726463519739,0.518409691411597,0.519022594153393),
 .UNSPECIFIED.);
#829=B_SPLINE_CURVE_WITH_KNOTS('',3,(#36393,#36394,#36395,#36396),
 .UNSPECIFIED.,.F.,.F.,(4,4),(-0.165567381125288,0.),.UNSPECIFIED.);
#830=B_SPLINE_CURVE_WITH_KNOTS('',3,(#36399,#36400,#36401,#36402,#36403,
#36404,#36405,#36406,#36407,#36408,#36409,#36410,#36411,#36412),
 .UNSPECIFIED.,.F.,.F.,(4,2,2,2,2,2,4),(0.0886615337454204,0.0907389095987879,
0.107041588865597,0.126817625016882,0.151565024549916,0.17449873389057,
0.174855361254283),.UNSPECIFIED.);
#831=B_SPLINE_CURVE_WITH_KNOTS('',3,(#36418,#36419,#36420,#36421,#36422,
#36423,#36424,#36425,#36426,#36427,#36428,#36429,#36430,#36431,#36432,#36433,
#36434,#36435,#36436,#36437,#36438,#36439,#36440,#36441,#36442,#36443,#36444,
#36445,#36446,#36447,#36448,#36449,#36450,#36451,#36452,#36453,#36454,#36455,
#36456,#36457,#36458,#36459,#36460,#36461,#36462,#36463,#36464,#36465,#36466,
#36467,#36468,#36469,#36470,#36471,#36472,#36473,#36474,#36475,#36476,#36477,
#36478,#36479,#36480,#36481,#36482,#36483,#36484,#36485,#36486,#36487,#36488,
#36489,#36490,#36491,#36492,#36493),.UNSPECIFIED.,.F.,.F.,(4,3,3,3,3,3,
3,3,3,3,3,3,3,3,3,3,3,3,3,3,3,3,3,3,3,4),(0.,9.73982238296995E-5,0.00019252004578257,
0.000194796447659399,0.000386060232528244,0.000389592895318797,0.00048315329443271,
0.000486991119148497,0.000531772924316341,0.000535690231063349,0.000560039787020775,
0.000580448963267321,0.000584389342978202,0.000776048112241012,0.000779185790637598,
0.000972895646006936,0.000973982238296993,0.00116877868595639,0.00117078841989245,
0.00126617690978609,0.0012700803416338,0.00131487602170093,0.00131980634716294,
0.00136357513361578,0.00136956336468157,0.00155837158127518),
 .UNSPECIFIED.);
#832=B_SPLINE_CURVE_WITH_KNOTS('',3,(#36494,#36495,#36496,#36497,#36498,
#36499,#36500,#36501,#36502,#36503,#36504,#36505,#36506,#36507,#36508,#36509,
#36510,#36511),.UNSPECIFIED.,.F.,.F.,(4,2,2,2,2,2,2,2,4),(-0.0823451520596356,
-0.0814641421114946,-0.079425143459902,-0.0765099977525957,-0.0745681831222406,
-0.0719848385051725,-0.0616691295558334,-0.0411719274467013,-9.99999319448164E-7),
 .UNSPECIFIED.);
#833=B_SPLINE_CURVE_WITH_KNOTS('',3,(#36513,#36514,#36515,#36516,#36517,
#36518,#36519,#36520,#36521,#36522,#36523,#36524,#36525,#36526,#36527,#36528,
#36529,#36530,#36531,#36532,#36533,#36534,#36535,#36536),.UNSPECIFIED.,
 .F.,.F.,(4,2,2,2,2,2,2,2,2,2,2,4),(-0.0818582793612237,-0.0408986769732426,
-0.0209173548870604,-0.0104500150359698,-0.00782862189102446,-0.00585645230784232,
-0.00289285619024227,-0.00141717783860899,-0.000679168113099727,-0.000303120243851664,
9.19584838832144E-10,7.57349769233838E-5),.UNSPECIFIED.);
#834=B_SPLINE_CURVE_WITH_KNOTS('',3,(#36538,#36539,#36540,#36541,#36542,
#36543,#36544,#36545,#36546,#36547,#36548,#36549,#36550,#36551,#36552,#36553,
#36554,#36555,#36556,#36557,#36558,#36559,#36560,#36561,#36562,#36563,#36564,
#36565,#36566,#36567,#36568,#36569,#36570,#36571,#36572,#36573,#36574,#36575,
#36576,#36577,#36578,#36579,#36580),.UNSPECIFIED.,.F.,.F.,(4,3,3,3,3,3,
3,3,3,3,3,3,3,3,4),(0.,0.000190596447604055,0.00024082472131754,0.00029102168932238,
0.000391254019785099,0.000589924182320116,0.00078656557642682,0.000983206970533523,
0.00100778714479686,0.00103236731906019,0.00108152766758686,0.0011798483646402,
0.00137648975874687,0.0014748104558002,0.00157313115285354),
 .UNSPECIFIED.);
#835=B_SPLINE_CURVE_WITH_KNOTS('',3,(#36586,#36587,#36588,#36589,#36590,
#36591,#36592,#36593,#36594,#36595),.UNSPECIFIED.,.F.,.F.,(4,2,2,2,4),(3.55271367880046E-15,
0.0721202303819016,0.0993400302468658,0.108173654477862,0.117007278708857),
 .UNSPECIFIED.);
#836=B_SPLINE_CURVE_WITH_KNOTS('',3,(#36613,#36614,#36615,#36616,#36617,
#36618,#36619,#36620,#36621,#36622,#36623,#36624,#36625,#36626,#36627,#36628,
#36629,#36630),.UNSPECIFIED.,.F.,.F.,(4,2,2,2,2,2,2,2,4),(-0.235513448497787,
-0.193326783450969,-0.151140118404152,-0.130797807210953,-0.117756724248895,
-0.104715641286835,-0.0843733300936382,-0.0421866650468191,0.),
 .UNSPECIFIED.);
#837=B_SPLINE_CURVE_WITH_KNOTS('',3,(#36636,#36637,#36638,#36639),
 .UNSPECIFIED.,.F.,.F.,(4,4),(0.000727522519127799,1.),.UNSPECIFIED.);
#838=B_SPLINE_CURVE_WITH_KNOTS('',3,(#36641,#36642,#36643,#36644,#36645,
#36646,#36647,#36648,#36649,#36650,#36651,#36652,#36653,#36654,#36655,#36656,
#36657,#36658,#36659,#36660,#36661,#36662,#36663,#36664,#36665,#36666,#36667,
#36668,#36669,#36670,#36671,#36672,#36673),.UNSPECIFIED.,.F.,.F.,(4,2,2,
1,2,2,2,1,1,1,2,2,2,2,2,1,2,2,4),(0.,0.0312500000000692,0.0468750000001036,
0.0546875000001194,0.0585937500001273,0.0625000000001351,0.125000000000152,
0.187500000000169,0.218750000000179,0.234375000000176,0.242187500000173,
0.250000000000169,0.375000000000013,0.437499999999922,0.468749999999877,
0.484374999999857,0.492187499999846,0.499999999999836,1.),.UNSPECIFIED.);
#839=B_SPLINE_CURVE_WITH_KNOTS('',3,(#36681,#36682,#36683,#36684,#36685,
#36686,#36687,#36688,#36689,#36690,#36691,#36692,#36693,#36694),
 .UNSPECIFIED.,.F.,.F.,(4,2,2,2,2,2,4),(-0.000385328305412479,1.70572106786282E-15,
0.0247793867166103,0.0515184272333669,0.0728860150158388,0.090500714324551,
0.092745274890908),.UNSPECIFIED.);
#840=B_SPLINE_CURVE_WITH_KNOTS('',3,(#36703,#36704,#36705,#36706,#36707,
#36708,#36709,#36710,#36711,#36712,#36713,#36714,#36715,#36716),
 .UNSPECIFIED.,.F.,.F.,(4,2,2,2,2,2,4),(-0.188304267635631,-0.187862880607499,
-0.166848428722395,-0.146905071719613,-0.125416885847754,-0.108754500181454,
-0.093931440303973),.UNSPECIFIED.);
#841=B_SPLINE_CURVE_WITH_KNOTS('',3,(#36719,#36720,#36721,#36722,#36723,
#36724,#36725,#36726,#36727,#36728,#36729,#36730,#36731,#36732),
 .UNSPECIFIED.,.F.,.F.,(4,2,2,2,2,2,4),(-0.0941733161862731,-0.079403572048281,
-0.0627829232813007,-0.0412936751319212,-0.02119709561475,0.,0.000443350791763836),
 .UNSPECIFIED.);
#842=B_SPLINE_CURVE_WITH_KNOTS('',3,(#36738,#36739,#36740,#36741,#36742,
#36743,#36744,#36745,#36746,#36747,#36748,#36749),.UNSPECIFIED.,.F.,.F.,
(4,2,2,2,2,4),(-0.000448819179553114,0.,0.0386802167200726,0.0689319278190867,
0.0909429437939334,0.108526726087003),.UNSPECIFIED.);
#843=B_SPLINE_CURVE_WITH_KNOTS('',3,(#36752,#36753,#36754,#36755,#36756,
#36757,#36758,#36759,#36760,#36761,#36762,#36763),.UNSPECIFIED.,.F.,.F.,
(4,2,2,2,2,4),(0.0962258393311769,0.110643300407674,0.128682242640802,0.153430032575363,
0.185007561669907,0.18537469972712),.UNSPECIFIED.);
#844=B_SPLINE_CURVE_WITH_KNOTS('',3,(#38300,#38301,#38302,#38303,#38304,
#38305,#38306,#38307,#38308,#38309,#38310,#38311,#38312,#38313,#38314,#38315,
#38316,#38317,#38318,#38319,#38320,#38321,#38322,#38323,#38324,#38325,#38326,
#38327,#38328,#38329,#38330,#38331,#38332,#38333,#38334,#38335,#38336,#38337,
#38338,#38339,#38340,#38341,#38342,#38343,#38344,#38345,#38346,#38347,#38348,
#38349,#38350,#38351,#38352,#38353,#38354,#38355,#38356,#38357,#38358,#38359,
#38360,#38361,#38362,#38363,#38364,#38365,#38366,#38367,#38368,#38369,#38370,
#38371,#38372,#38373,#38374,#38375,#38376,#38377,#38378,#38379,#38380,#38381,
#38382,#38383,#38384,#38385,#38386,#38387,#38388,#38389,#38390,#38391,#38392,
#38393,#38394,#38395,#38396,#38397,#38398,#38399,#38400,#38401,#38402,#38403,
#38404,#38405,#38406,#38407,#38408,#38409,#38410,#38411,#38412,#38413,#38414,
#38415,#38416,#38417,#38418,#38419,#38420,#38421,#38422,#38423,#38424,#38425,
#38426,#38427,#38428,#38429,#38430,#38431,#38432,#38433,#38434,#38435,#38436,
#38437,#38438,#38439,#38440,#38441,#38442,#38443,#38444,#38445,#38446,#38447,
#38448,#38449,#38450,#38451,#38452,#38453,#38454,#38455,#38456,#38457,#38458,
#38459,#38460,#38461,#38462,#38463,#38464,#38465,#38466,#38467,#38468,#38469,
#38470,#38471,#38472,#38473,#38474,#38475,#38476,#38477,#38478,#38479,#38480,
#38481,#38482,#38483,#38484,#38485,#38486,#38487,#38488,#38489,#38490,#38491,
#38492,#38493,#38494,#38495,#38496,#38497,#38498,#38499,#38500,#38501,#38502,
#38503,#38504,#38505,#38506,#38507,#38508,#38509,#38510,#38511,#38512,#38513),
 .UNSPECIFIED.,.F.,.F.,(4,3,3,3,3,3,3,3,3,3,3,3,3,3,3,3,3,3,3,3,3,3,3,3,
3,3,3,3,3,3,3,3,3,3,3,3,3,3,3,3,3,3,3,3,3,3,3,3,3,3,3,3,3,3,3,3,3,3,3,3,
3,3,3,3,3,3,3,3,3,3,3,4),(0.00181838839577617,0.00182764386550164,0.00184964353720942,
0.00187794335639532,0.00190763520719598,0.00190930945776452,0.00192250723231261,
0.00192422593790331,0.00193742583690015,0.00193914241804209,0.00196897537831967,
0.00199710160830158,0.00199880833859725,0.0020120204119779,0.00201372481873603,
0.00202693953123418,0.00202864129887482,0.00205677738648887,0.00208830721942998,
0.00211645310942199,0.00211814017970755,0.00212391258051836,0.00213137205065051,
0.00213305665984635,0.00214629098961237,0.00214797313998514,0.00217612888023953,
0.00220596674733626,0.00220763906054031,0.0022208856864302,0.0022225555406791,
0.00222834514776207,0.00223580462220084,0.0022374720208179,0.00226730498109548,
0.00229547760561947,0.00232531799373752,0.00232697090165065,0.00234023727065812,
0.00234188738178944,0.00235515613654191,0.00235680386192822,0.00238663682220578,
0.00241483189593419,0.00241646978248335,0.00242975087335353,0.00243138626262213,
0.00244466977649174,0.00244630274276092,0.00247450763036943,0.00250596866331607,
0.00253418361230688,0.00253580162359365,0.0025416420294745,0.00254910146409367,
0.00256402127173024,0.00256563458387123,0.00259385882465156,0.00262369701173162,
0.00262530050442639,0.00263861585880305,0.00264021698456519,0.00265353488839818,
0.00265513346470398,0.00268496642498156,0.00271321069336538,0.00271479938525913,
0.00272812950694487,0.00272971586539792,0.00274304860630799,0.00274463234553671,
0.00277288643986402),.UNSPECIFIED.);
#845=B_SPLINE_CURVE_WITH_KNOTS('',3,(#38962,#38963,#38964,#38965,#38966,
#38967,#38968,#38969,#38970,#38971,#38972,#38973,#38974,#38975,#38976,#38977,
#38978,#38979,#38980,#38981,#38982,#38983,#38984,#38985,#38986,#38987,#38988,
#38989,#38990,#38991,#38992,#38993,#38994,#38995,#38996,#38997,#38998,#38999,
#39000,#39001,#39002,#39003,#39004,#39005,#39006,#39007,#39008,#39009,#39010,
#39011,#39012,#39013,#39014,#39015,#39016,#39017,#39018,#39019,#39020,#39021,
#39022,#39023,#39024,#39025,#39026,#39027,#39028,#39029,#39030,#39031,#39032,
#39033,#39034,#39035,#39036,#39037,#39038,#39039,#39040,#39041,#39042,#39043,
#39044,#39045,#39046,#39047,#39048,#39049,#39050,#39051,#39052,#39053,#39054,
#39055,#39056,#39057,#39058,#39059,#39060,#39061,#39062,#39063,#39064,#39065,
#39066,#39067,#39068,#39069,#39070,#39071,#39072,#39073,#39074,#39075,#39076,
#39077,#39078,#39079,#39080,#39081,#39082,#39083,#39084,#39085,#39086,#39087,
#39088,#39089,#39090,#39091,#39092,#39093,#39094,#39095,#39096,#39097,#39098,
#39099,#39100,#39101,#39102,#39103,#39104,#39105,#39106,#39107,#39108,#39109,
#39110,#39111,#39112,#39113,#39114,#39115,#39116,#39117,#39118,#39119,#39120,
#39121,#39122,#39123,#39124,#39125,#39126,#39127,#39128,#39129,#39130,#39131,
#39132,#39133,#39134,#39135,#39136,#39137,#39138,#39139,#39140,#39141,#39142,
#39143,#39144,#39145,#39146,#39147,#39148,#39149,#39150,#39151,#39152,#39153,
#39154,#39155,#39156,#39157,#39158,#39159,#39160,#39161,#39162,#39163,#39164,
#39165,#39166,#39167,#39168,#39169,#39170,#39171,#39172,#39173,#39174,#39175),
 .UNSPECIFIED.,.F.,.F.,(4,3,3,3,3,3,3,3,3,3,3,3,3,3,3,3,3,3,3,3,3,3,3,3,
3,3,3,3,3,3,3,3,3,3,3,3,3,3,3,3,3,3,3,3,3,3,3,3,3,3,3,3,3,3,3,3,3,3,3,3,
3,3,3,3,3,3,3,3,3,3,3,4),(1.16051834735224E-5,1.493476621997E-5,2.986953243994E-5,
4.14803381536968E-5,5.973906487988E-5,7.13545593270396E-5,8.960859731982E-5,
0.00010122861902708,0.000104543363539795,0.000116165788001039,0.00011947812975977,
0.000131102516262791,0.00017921719463969,0.000190851997707725,0.000209086727079646,
0.000220725563339751,0.000224021493299624,0.000238956259519601,0.000250599218308967,
0.000298695324399528,0.000310347338597952,0.000313630090619511,0.000325284880712085,
0.000328564856839494,0.000340221602554756,0.000358434389279461,0.00037009570634431,
0.000399969818859634,0.000414906878365008,0.000418173454159394,0.000422375399610592,
0.000429843922048107,0.000433108220379377,0.000448042986599361,0.000477912519039327,
0.000489592134427833,0.000507782051479294,0.000519466263512958,0.000522716817699277,
0.000534403777182626,0.00053765158391926,0.000549340376544938,0.000597390648799192,
0.000609090041569225,0.000624026559493112,0.00062726018123916,0.00063896232213999,
0.000642194947459142,0.000657129713679124,0.000668836802496252,0.000716868778559061,
0.000728584194058549,0.000731803544779041,0.000743521593993477,0.00074673831099902,
0.000758459202638857,0.000776607843438971,0.000788333309895947,0.000806477375878921,
0.000818207334889621,0.000821412142098897,0.000833144688766855,0.000836346908318872,
0.000848081531617883,0.000896085973198773,0.000907828831845864,0.000922766520025946,
0.000925955505638724,0.000937704197704619,0.000940890271858694,0.000955825038078664,
0.000967577998166243),.UNSPECIFIED.);
#846=B_SPLINE_CURVE_WITH_KNOTS('',3,(#39182,#39183,#39184,#39185,#39186,
#39187,#39188,#39189,#39190,#39191,#39192,#39193,#39194,#39195,#39196,#39197,
#39198,#39199,#39200,#39201,#39202,#39203,#39204,#39205,#39206,#39207,#39208,
#39209,#39210,#39211,#39212,#39213,#39214,#39215,#39216,#39217,#39218,#39219,
#39220,#39221,#39222,#39223,#39224,#39225,#39226,#39227,#39228,#39229,#39230,
#39231,#39232,#39233,#39234,#39235,#39236,#39237,#39238,#39239,#39240,#39241,
#39242,#39243,#39244,#39245,#39246,#39247,#39248,#39249,#39250,#39251,#39252,
#39253,#39254,#39255,#39256,#39257,#39258,#39259,#39260,#39261,#39262,#39263,
#39264,#39265,#39266,#39267,#39268,#39269,#39270,#39271,#39272,#39273,#39274,
#39275,#39276,#39277,#39278,#39279,#39280,#39281,#39282,#39283,#39284,#39285,
#39286,#39287,#39288,#39289,#39290,#39291,#39292,#39293,#39294,#39295,#39296,
#39297,#39298,#39299,#39300,#39301,#39302,#39303,#39304,#39305,#39306,#39307,
#39308,#39309,#39310,#39311,#39312,#39313,#39314,#39315,#39316,#39317,#39318,
#39319,#39320,#39321,#39322,#39323,#39324,#39325,#39326,#39327,#39328,#39329,
#39330,#39331,#39332,#39333,#39334,#39335,#39336,#39337,#39338,#39339,#39340,
#39341,#39342,#39343,#39344,#39345,#39346,#39347,#39348,#39349,#39350,#39351,
#39352,#39353,#39354,#39355,#39356,#39357,#39358,#39359,#39360,#39361,#39362,
#39363,#39364,#39365,#39366,#39367,#39368,#39369,#39370,#39371,#39372,#39373,
#39374,#39375,#39376,#39377,#39378,#39379,#39380,#39381,#39382,#39383),
 .UNSPECIFIED.,.F.,.F.,(4,3,3,3,3,3,3,3,3,3,3,3,3,3,3,3,3,3,3,3,3,3,3,3,
3,3,3,3,3,3,3,3,3,3,3,3,3,3,3,3,3,3,3,3,3,3,3,3,3,3,3,3,3,3,3,3,3,3,3,3,
3,3,3,3,3,3,3,4),(0.000863576982099504,0.000893415377688714,0.000894988808327375,
0.000908326951236741,0.000923246281154781,0.000954654728882556,0.000982928494721109,
0.000984487689160143,0.00099784771503611,0.000999404169298931,0.00101276621276172,
0.00101432064943772,0.0010426043099559,0.00107398656999286,0.00110228001659828,
0.00110381953027044,0.0011321178395976,0.00113365249054802,0.00116195519971085,
0.00119179359098349,0.00119331841110319,0.00120671253144932,0.00120823489124197,
0.00122163150653409,0.00122315137138076,0.00125298433165833,0.00128130729281906,
0.00128281729193591,0.00129622608400764,0.00129773377207469,0.00131114520917519,
0.00131265025221348,0.00134098306403575,0.00137231617276862,0.0014006587939414,
0.00140214913304619,0.0014081182647691,0.00141557773488575,0.00141706561318497,
0.00143049667390546,0.00143198209332375,0.00146033456285987,0.00149017243153675,
0.00149164801387886,0.00150509127393628,0.00150656449401764,0.00152001034775925,
0.00152148097415642,0.00155131393443396,0.00157968447035871,0.00160952384680422,
0.00161097985498904,0.0016169840698581,0.00162444291082146,0.00162589633512782,
0.00163936182129664,0.00164081281526659,0.00167064577554414,0.00169903758015923,
0.00170047873582169,0.00171395651569461,0.00172887545911729,0.00173031169609923,
0.0017587131784449,0.00178855120104918,0.00178997761665432,0.0018048940967931,
0.00181838839577617),.UNSPECIFIED.);
#847=B_SPLINE_CURVE_WITH_KNOTS('',3,(#39828,#39829,#39830,#39831,#39832,
#39833,#39834,#39835,#39836,#39837,#39838,#39839,#39840,#39841,#39842,#39843,
#39844,#39845,#39846,#39847,#39848,#39849,#39850,#39851,#39852,#39853,#39854,
#39855,#39856,#39857,#39858,#39859,#39860,#39861,#39862,#39863,#39864,#39865,
#39866,#39867,#39868,#39869,#39870,#39871,#39872,#39873,#39874,#39875,#39876,
#39877,#39878,#39879,#39880,#39881,#39882,#39883,#39884,#39885,#39886,#39887,
#39888,#39889,#39890,#39891,#39892,#39893,#39894,#39895,#39896,#39897,#39898,
#39899,#39900,#39901,#39902,#39903,#39904,#39905,#39906,#39907,#39908,#39909,
#39910,#39911,#39912,#39913,#39914,#39915,#39916,#39917,#39918,#39919,#39920,
#39921,#39922,#39923,#39924,#39925,#39926,#39927,#39928,#39929,#39930,#39931,
#39932,#39933,#39934,#39935,#39936,#39937,#39938,#39939,#39940,#39941,#39942,
#39943,#39944,#39945,#39946,#39947,#39948,#39949,#39950,#39951,#39952,#39953,
#39954,#39955,#39956,#39957,#39958,#39959,#39960,#39961,#39962,#39963,#39964,
#39965,#39966,#39967,#39968,#39969,#39970,#39971,#39972,#39973,#39974,#39975,
#39976,#39977,#39978,#39979,#39980,#39981,#39982,#39983,#39984,#39985,#39986,
#39987,#39988,#39989,#39990,#39991,#39992,#39993,#39994,#39995,#39996,#39997,
#39998,#39999,#40000,#40001,#40002,#40003,#40004,#40005,#40006,#40007,#40008,
#40009,#40010,#40011,#40012,#40013,#40014,#40015,#40016,#40017,#40018,#40019,
#40020,#40021,#40022,#40023,#40024,#40025,#40026,#40027,#40028,#40029,#40030,
#40031,#40032,#40033,#40034,#40035,#40036,#40037,#40038),.UNSPECIFIED.,
 .F.,.F.,(4,3,3,3,3,3,3,3,3,3,3,3,3,3,3,3,3,3,3,3,3,3,3,3,3,3,3,3,3,3,3,
3,3,3,3,3,3,3,3,3,3,3,3,3,3,3,3,3,3,3,3,3,3,3,3,3,3,3,3,3,3,3,3,3,3,3,3,
3,3,3,4),(0.000967577998166243,0.000985694570518615,0.000997452104970326,
0.00101238917013626,0.00101556410295857,0.00102732620518103,0.00107530316783846,
0.00108707491923346,0.00110201144791451,0.0011051727002784,0.00110947846831176,
0.00111694691155728,0.00113504223271835,0.00114682263399536,0.00119478129759824,
0.00120657015384326,0.00120971606381822,0.00122150734177849,0.0012246508300382,
0.00123644503461287,0.00125452036247816,0.0012663191435441,0.00128438989491812,
0.00129619324251587,0.00129932466113811,0.00131112984419676,0.00131425942735809,
0.00132606550487095,0.00137399849223803,0.0013858155767176,0.00140075265939606,
0.00140386802467799,0.0014082211872552,0.00141568971683767,0.00141880279089798,
0.00143373755711796,0.00144556379707782,0.00149347662199789,0.00150531189682198,
0.00150841138821788,0.0015202496101457,0.00152334615443786,0.00153518618508574,
0.00155321568687783,0.00156506022979621,0.00159493423161199,0.00160987166971053,
0.00161295475175777,0.00162480857197639,0.00162788951797776,0.00164282428419775,
0.00167269381663772,0.00168455672937543,0.00170256334907769,0.00171443152813003,
0.00171749811529767,0.00172189869624108,0.00172936775988772,0.00173243288151765,
0.00174430495412123,0.00179217194639758,0.00180405320053485,0.00180710671261757,
0.00181898963002168,0.00182204147883755,0.0018339180528411,0.00185191101127753,
0.00186374210842334,0.00189350855411201,0.00191165007615749,0.00192325525963101),
 .UNSPECIFIED.);
#848=B_SPLINE_CURVE_WITH_KNOTS('',3,(#41383,#41384,#41385,#41386,#41387,
#41388,#41389,#41390,#41391,#41392,#41393,#41394,#41395,#41396,#41397,#41398),
 .UNSPECIFIED.,.F.,.F.,(4,2,2,2,2,2,2,4),(-0.00044779014185856,0.,0.0229409691169892,
0.0448607972358344,0.0664784333744104,0.0823924396306553,0.0961964805679204,
0.0962258393298038),.UNSPECIFIED.);
#849=B_SPLINE_CURVE_WITH_KNOTS('',3,(#41401,#41402,#41403,#41404,#41405,
#41406,#41407,#41408,#41409,#41410,#41411,#41412),.UNSPECIFIED.,.F.,.F.,
(4,2,2,2,2,4),(0.0963708477811746,0.110766905123989,0.128787592759141,0.15355503814959,
0.185223004044538,0.185590457789025),.UNSPECIFIED.);
#850=B_SPLINE_CURVE_WITH_KNOTS('',3,(#41417,#41418,#41419,#41420,#41421,
#41422,#41423,#41424,#41425,#41426,#41427,#41428,#41429,#41430),
 .UNSPECIFIED.,.F.,.F.,(4,2,2,2,2,2,4),(-0.0939314403051867,-0.0791083804274454,
-0.062445994760847,-0.0409578088886071,-0.0210144518854656,-2.88935542158697E-14,
0.000441387027557035),.UNSPECIFIED.);
#851=B_SPLINE_CURVE_WITH_KNOTS('',3,(#41433,#41434,#41435,#41436,#41437,
#41438,#41439,#41440,#41441,#41442,#41443,#41444,#41445,#41446),
 .UNSPECIFIED.,.F.,.F.,(4,2,2,2,2,2,4),(-0.188789983926297,-0.188346633130585,
-0.167149537440147,-0.147052957839446,-0.125563709600744,-0.108943060764686,
-0.0941733165652966),.UNSPECIFIED.);
#852=B_SPLINE_CURVE_WITH_KNOTS('',3,(#41454,#41455,#41456,#41457,#41458,
#41459,#41460,#41461,#41462,#41463,#41464,#41465,#41466,#41467),
 .UNSPECIFIED.,.F.,.F.,(4,2,2,2,2,2,4),(-0.210772012984322,-0.210280903065,
-0.177423583499178,-0.148314265031791,-0.126331471038667,-0.108064160223483,
-0.100943721292222),.UNSPECIFIED.);
#853=B_SPLINE_CURVE_WITH_KNOTS('',3,(#41471,#41472,#41473,#41474,#41475,
#41476,#41477,#41478,#41479,#41480,#41481,#41482,#41483,#41484),
 .UNSPECIFIED.,.F.,.F.,(4,2,2,2,2,2,4),(-0.000412787679576566,0.,0.0283682641149075,
0.0526479899564725,0.0709415556714253,0.0861626427768875,0.0917971386713504),
 .UNSPECIFIED.);
#854=B_SPLINE_CURVE_WITH_KNOTS('',3,(#41635,#41636,#41637,#41638,#41639,
#41640,#41641,#41642,#41643,#41644),.UNSPECIFIED.,.F.,.F.,(4,2,2,2,4),(-0.00349842735434734,
-2.74352589257898E-12,0.0521414590439604,0.0796329571011274,0.104846643196789),
 .UNSPECIFIED.);
#855=B_SPLINE_CURVE_WITH_KNOTS('',3,(#41800,#41801,#41802,#41803,#41804,
#41805,#41806,#41807,#41808,#41809,#41810,#41811,#41812,#41813,#41814,#41815,
#41816,#41817,#41818,#41819,#41820,#41821,#41822,#41823,#41824,#41825,#41826,
#41827,#41828,#41829,#41830,#41831,#41832,#41833,#41834,#41835,#41836,#41837,
#41838,#41839,#41840,#41841,#41842,#41843,#41844,#41845,#41846,#41847,#41848,
#41849,#41850,#41851,#41852,#41853,#41854,#41855,#41856,#41857,#41858,#41859,
#41860,#41861,#41862,#41863,#41864,#41865,#41866,#41867,#41868,#41869,#41870,
#41871,#41872,#41873,#41874,#41875,#41876,#41877,#41878,#41879,#41880,#41881,
#41882,#41883,#41884,#41885,#41886,#41887,#41888,#41889,#41890,#41891,#41892,
#41893,#41894,#41895,#41896,#41897,#41898,#41899,#41900,#41901,#41902,#41903,
#41904,#41905,#41906,#41907,#41908,#41909,#41910,#41911,#41912,#41913,#41914,
#41915,#41916,#41917,#41918,#41919,#41920,#41921,#41922,#41923,#41924,#41925,
#41926,#41927,#41928,#41929,#41930,#41931,#41932,#41933,#41934,#41935,#41936,
#41937,#41938,#41939,#41940,#41941,#41942,#41943,#41944,#41945,#41946,#41947,
#41948,#41949,#41950,#41951,#41952,#41953),.UNSPECIFIED.,.F.,.F.,(4,3,3,
3,3,3,3,3,3,3,3,3,3,3,3,3,3,3,3,3,3,3,3,3,3,3,3,3,3,3,3,3,3,3,3,3,3,3,3,
3,3,3,3,3,3,3,3,3,3,3,3,4),(0.,3.75072506682356E-5,6.03395682026754E-5,
7.50145013364712E-5,8.43913140035302E-5,9.37681266705891E-5,0.000112521752004707,
0.000118020145270055,0.000131275377338824,0.000132487485027507,0.000147073827762125,
0.000150029002672942,0.000176606237268957,0.000187536253341185,0.000206289878675303,
0.000225043504009422,0.000237243896542391,0.00024379712934354,0.000253016586246074,
0.000262550754677658,0.000269091009696469,0.000300058005345894,0.000302111818529164,
0.000337565256014129,0.000371377991455727,0.000375072506682365,0.000393826132016483,
0.000407518571944512,0.000412579757350601,0.000444600452064642,0.000450087008018838,
0.000515403930086837,0.000521321544297857,0.000525101509355314,0.00060011601069179,
0.000601142173193074,0.000621551460391748,0.000637623261360026,0.00064212154415199,
0.000675130512028263,0.00068361343341191,0.000750145013364734,0.000767896109444578,
0.000853794321857111,0.000900174016037677,0.000941224992165524,0.000975188517374148,
0.000985498887476787,0.00101269576804238,0.00103003827125258,0.00105020301871062,
0.00120023202138355),.UNSPECIFIED.);
#856=B_SPLINE_CURVE_WITH_KNOTS('',3,(#41971,#41972,#41973,#41974,#41975,
#41976,#41977,#41978,#41979,#41980,#41981,#41982,#41983,#41984),
 .UNSPECIFIED.,.F.,.F.,(4,2,2,2,2,2,4),(0.0886615337472132,0.0907389096006223,
0.107041588867765,0.126817625019457,0.151565024553096,0.174498733894337,
0.174855361258075),.UNSPECIFIED.);
#857=B_SPLINE_CURVE_WITH_KNOTS('',3,(#41986,#41987,#41988,#41989,#41990,
#41991,#41992,#41993,#41994,#41995),.UNSPECIFIED.,.F.,.F.,(4,2,2,2,4),(0.0745079449586904,
0.0933896612732089,0.112173398676393,0.130768592867116,0.149172319853601),
 .UNSPECIFIED.);
#858=B_SPLINE_CURVE_WITH_KNOTS('',3,(#42017,#42018,#42019,#42020,#42021,
#42022,#42023,#42024,#42025,#42026,#42027,#42028,#42029,#42030),
 .UNSPECIFIED.,.F.,.F.,(4,2,2,2,2,2,4),(0.0886615337459981,0.0907389095993787,
0.107041588866303,0.126817625017728,0.151565024551055,0.174498733892164,
0.174855361255883),.UNSPECIFIED.);
#859=B_SPLINE_CURVE_WITH_KNOTS('',3,(#42235,#42236,#42237,#42238,#42239,
#42240,#42241,#42242,#42243,#42244,#42245,#42246,#42247,#42248,#42249,#42250,
#42251,#42252,#42253,#42254,#42255,#42256,#42257,#42258,#42259,#42260,#42261,
#42262,#42263,#42264,#42265,#42266,#42267,#42268,#42269,#42270,#42271,#42272,
#42273,#42274,#42275,#42276,#42277,#42278,#42279,#42280,#42281,#42282,#42283,
#42284,#42285,#42286,#42287,#42288,#42289,#42290,#42291,#42292,#42293,#42294,
#42295,#42296,#42297,#42298,#42299,#42300,#42301,#42302,#42303,#42304,#42305,
#42306,#42307,#42308,#42309,#42310,#42311,#42312,#42313,#42314,#42315,#42316,
#42317,#42318,#42319,#42320,#42321,#42322,#42323,#42324,#42325,#42326,#42327,
#42328,#42329,#42330,#42331,#42332,#42333,#42334,#42335,#42336,#42337,#42338,
#42339,#42340,#42341,#42342,#42343,#42344,#42345,#42346,#42347,#42348,#42349,
#42350,#42351,#42352,#42353,#42354,#42355,#42356,#42357,#42358,#42359,#42360,
#42361,#42362,#42363,#42364,#42365,#42366,#42367,#42368,#42369,#42370,#42371,
#42372,#42373,#42374,#42375,#42376,#42377,#42378,#42379,#42380,#42381,#42382,
#42383,#42384,#42385,#42386,#42387,#42388,#42389,#42390,#42391,#42392,#42393,
#42394,#42395,#42396,#42397),.UNSPECIFIED.,.F.,.F.,(4,3,3,3,3,3,3,3,3,3,
3,3,3,3,3,3,3,3,3,3,3,3,3,3,3,3,3,3,3,3,3,3,3,3,3,3,3,3,3,3,3,3,3,3,3,3,
3,3,3,3,3,3,3,3,4),(0.,0.0340147436347705,0.0796654100921325,0.121150235206392,
0.16258274933431,0.189677904438364,0.227859710016422,0.242187499996718,
0.246836013781419,0.249999999996616,0.288220212410142,0.311288214891701,
0.34470470346921,0.365172426794162,0.371093749995032,0.374999999994983,
0.389696018730405,0.405679200193564,0.409288359158387,0.427230980167802,
0.433593749994273,0.437208894920299,0.437499999994228,0.45349495870215,
0.466556751031909,0.482527649839429,0.49804687499366,0.499999999993643,
0.514675935726806,0.526075117753044,0.542334433873725,0.556301931927462,
0.558593749994405,0.561295009043853,0.562499999994452,0.567510296898257,
0.597538662312543,0.60937499999504,0.619397988471943,0.624837579898199,
0.624999999995238,0.657086602514375,0.68282993630191,0.717724404284978,
0.742187499996745,0.747700569938847,0.749999999996844,0.751088206824535,
0.783457115912507,0.818040475412505,0.860724294573825,0.904220867740056,
0.952110414151086,0.994093280424259,0.999999960562115),.UNSPECIFIED.);
#860=B_SPLINE_CURVE_WITH_KNOTS('',3,(#42399,#42400,#42401,#42402,#42403,
#42404,#42405,#42406),.UNSPECIFIED.,.F.,.F.,(4,2,2,4),(-0.000330927471132683,
-4.60980603380267E-9,0.0122588170368006,0.0209462363748979),
 .UNSPECIFIED.);
#861=B_SPLINE_CURVE_WITH_KNOTS('',3,(#42518,#42519,#42520,#42521,#42522,
#42523,#42524,#42525,#42526,#42527,#42528,#42529,#42530,#42531,#42532,#42533,
#42534,#42535,#42536,#42537,#42538,#42539,#42540,#42541,#42542,#42543,#42544,
#42545,#42546,#42547,#42548,#42549,#42550,#42551,#42552,#42553,#42554,#42555,
#42556,#42557,#42558,#42559,#42560),.UNSPECIFIED.,.F.,.F.,(4,3,3,3,3,3,
3,3,3,3,3,3,3,3,4),(0.,0.083607507194038,0.166803753597019,0.25,0.328236652674478,
0.406218055000426,0.484054848510691,0.5,0.578122914091021,0.656344013643421,
0.734920106325271,0.75,0.834722429329149,0.92066309428102,0.999999651298147),
 .UNSPECIFIED.);
#862=B_SPLINE_CURVE_WITH_KNOTS('',3,(#42643,#42644,#42645,#42646,#42647,
#42648,#42649,#42650,#42651,#42652,#42653,#42654,#42655,#42656,#42657,#42658,
#42659,#42660,#42661,#42662,#42663,#42664,#42665),.UNSPECIFIED.,.F.,.F.,
(4,1,1,1,2,2,2,2,2,1,1,2,2,4),(6.31448876631291E-18,0.000104906811635738,
0.000209813623271469,0.000314720434907201,0.000419627246542932,0.000524534058178664,
0.00057698746399653,0.000629440869814395,0.000734347681450129,0.000786801087267997,
0.000813027790176931,0.000826141141631399,0.00083269781735863,0.000839254493085862),
 .UNSPECIFIED.);
#863=B_SPLINE_CURVE_WITH_KNOTS('',3,(#42666,#42667,#42668,#42669,#42670,
#42671,#42672,#42673,#42674,#42675,#42676,#42677,#42678,#42679,#42680,#42681),
 .UNSPECIFIED.,.F.,.F.,(4,2,2,2,2,2,2,4),(0.,0.000213634091527792,0.00026704261440974,
0.000320451137291689,0.00042726818305558,0.000640902274583368,0.000747719320347264,
0.000854536366111159),.UNSPECIFIED.);
#864=B_SPLINE_CURVE_WITH_KNOTS('',3,(#42764,#42765,#42766,#42767,#42768,
#42769,#42770,#42771,#42772,#42773,#42774,#42775,#42776,#42777,#42778,#42779,
#42780,#42781,#42782,#42783,#42784,#42785,#42786,#42787,#42788,#42789,#42790,
#42791,#42792,#42793,#42794,#42795,#42796,#42797,#42798,#42799,#42800,#42801,
#42802,#42803,#42804,#42805,#42806,#42807,#42808,#42809,#42810,#42811,#42812,
#42813,#42814,#42815,#42816,#42817,#42818,#42819,#42820,#42821,#42822,#42823,
#42824,#42825,#42826,#42827,#42828,#42829,#42830,#42831,#42832,#42833,#42834,
#42835,#42836,#42837,#42838,#42839,#42840,#42841,#42842,#42843,#42844,#42845,
#42846,#42847,#42848),.UNSPECIFIED.,.F.,.F.,(4,3,3,3,3,3,3,3,3,3,3,3,3,
3,3,3,3,3,3,3,3,3,3,3,3,3,3,3,4),(-0.00084007102973227,-0.000833507974812657,
-0.00082694491989287,-0.000813818810053298,-0.000799319178203659,-0.000787566590374158,
-0.000757799963646104,-0.000735062151015878,-0.000673123074247421,-0.000630053272299322,
-0.000586475425630851,-0.000525044393582767,-0.000497658838514586,-0.000472539954224489,
-0.000420035514866211,-0.000335812876675837,-0.000315026636149658,-0.000310877818697253,
-0.000232328685341806,-0.000210017757433106,-0.000137430443904471,-0.000107807929015954,
-0.000105008878716553,-5.25044393582766E-5,-2.62522196791383E-5,-1.31261098395691E-5,
-6.56305491978457E-6,-3.28152745989229E-6,0.),.UNSPECIFIED.);
#865=B_SPLINE_CURVE_WITH_KNOTS('',3,(#42849,#42850,#42851,#42852,#42853,
#42854,#42855,#42856,#42857,#42858,#42859,#42860,#42861,#42862,#42863),
 .UNSPECIFIED.,.F.,.F.,(4,2,2,2,2,2,1,4),(0.,0.000106412085437288,0.000212824170874576,
0.00042564834174915,0.000532060427186437,0.00058526646990508,0.000638472512623723,
0.000851296683498299),.UNSPECIFIED.);
#866=B_SPLINE_CURVE_WITH_KNOTS('',3,(#42869,#42870,#42871,#42872,#42873,
#42874,#42875,#42876,#42877,#42878,#42879,#42880,#42881,#42882,#42883,#42884,
#42885,#42886,#42887,#42888,#42889,#42890,#42891,#42892,#42893,#42894,#42895,
#42896,#42897,#42898,#42899,#42900,#42901,#42902,#42903,#42904,#42905,#42906,
#42907,#42908,#42909,#42910,#42911,#42912,#42913,#42914,#42915,#42916,#42917,
#42918,#42919,#42920,#42921,#42922,#42923,#42924,#42925,#42926,#42927,#42928,
#42929,#42930,#42931,#42932,#42933,#42934,#42935,#42936,#42937,#42938,#42939,
#42940,#42941,#42942,#42943,#42944,#42945,#42946,#42947,#42948,#42949,#42950,
#42951,#42952,#42953,#42954,#42955,#42956,#42957,#42958,#42959,#42960,#42961,
#42962,#42963,#42964,#42965,#42966,#42967,#42968),.UNSPECIFIED.,.F.,.F.,
(4,3,3,3,3,3,3,3,3,3,3,3,3,3,3,3,3,3,3,3,3,3,3,3,3,3,3,3,3,3,3,3,3,4),(-0.00256394233172042,
-0.00254391153225385,-0.00252388073278728,-0.00248381913385415,-0.00240369593598789,
-0.00224344954025536,-0.00192295674879031,-0.00190873837330291,-0.00160246395732526,
-0.00158284541228051,-0.00144221756159274,-0.00141973271419307,-0.00137890325788483,
-0.00136209436372648,-0.00133806214634055,-0.00128197116586021,-0.00125658871715488,
-0.000961478374395163,-0.000933814475721374,-0.000801231978662637,-0.000774027171965909,
-0.000640985582930111,-0.000615098742888476,-0.000575479456072158,-0.000560862385063846,
-0.000535906116609504,-0.000520800786130713,-0.000480739187197579,-0.000457228296741512,
-0.000320492791465053,-0.000302025544602755,-0.000160246395732526,-0.000149632584598168,
0.),.UNSPECIFIED.);
#867=B_SPLINE_CURVE_WITH_KNOTS('',3,(#42973,#42974,#42975,#42976,#42977,
#42978,#42979,#42980,#42981,#42982,#42983,#42984,#42985,#42986),
 .UNSPECIFIED.,.F.,.F.,(4,2,2,2,2,2,4),(-0.0927452748896928,-0.0905007143233686,
-0.0728860150149103,-0.0515184272327515,-0.024779386716326,0.,0.000385328304981227),
 .UNSPECIFIED.);
#868=B_SPLINE_CURVE_WITH_KNOTS('',3,(#43123,#43124,#43125,#43126,#43127,
#43128,#43129,#43130,#43131,#43132),.UNSPECIFIED.,.F.,.F.,(4,2,2,2,4),(0.148156232466478,
0.185223245600188,0.222275576316647,0.259307076631218,0.296319939605705),
 .UNSPECIFIED.);
#869=B_SPLINE_CURVE_WITH_KNOTS('',3,(#43148,#43149,#43150,#43151,#43152,
#43153,#43154,#43155,#43156,#43157,#43158,#43159,#43160,#43161,#43162,#43163,
#43164,#43165,#43166,#43167,#43168,#43169,#43170,#43171,#43172,#43173,#43174,
#43175),.UNSPECIFIED.,.F.,.F.,(4,2,2,1,1,1,1,2,2,2,1,2,2,1,2,1,1,4),(-0.000564130987588538,
-0.000559723714247997,-0.000558621895912863,-0.000557520077577729,-0.000555316440907461,
-0.000546501894226388,-0.000528872800864246,-0.000511243707502104,-0.000493614614139961,
-0.000423098240691392,-0.000352581867242823,-0.000282065493794254,-0.000264436400432113,
-0.000246807307069971,-0.000211549120345689,-0.000141032746897126,-7.0516373448563E-5,
0.),.UNSPECIFIED.);
#870=B_SPLINE_CURVE_WITH_KNOTS('',3,(#43215,#43216,#43217,#43218,#43219,
#43220),.UNSPECIFIED.,.F.,.F.,(4,2,4),(-0.296319939605705,-0.259307076631217,
-0.246794048708148),.UNSPECIFIED.);
#871=B_SPLINE_CURVE_WITH_KNOTS('',3,(#43286,#43287,#43288,#43289,#43290,
#43291,#43292,#43293,#43294,#43295),.UNSPECIFIED.,.F.,.F.,(4,2,2,2,4),(1.85749660968514E-7,
0.0288862347368519,0.0436805225665364,0.0576117094512964,0.0578367161617181),
 .UNSPECIFIED.);
#872=B_SPLINE_CURVE_WITH_KNOTS('',3,(#43352,#43353,#43354,#43355,#43356,
#43357,#43358,#43359,#43360,#43361),.UNSPECIFIED.,.F.,.F.,(4,2,2,2,4),(-0.000222102919063948,
5.84805343767944E-7,0.0138000274043402,0.0285383241859604,0.0573925375846453),
 .UNSPECIFIED.);
#873=B_SPLINE_CURVE_WITH_KNOTS('',3,(#43365,#43366,#43367,#43368,#43369,
#43370,#43371,#43372,#43373,#43374,#43375,#43376,#43377,#43378),
 .UNSPECIFIED.,.F.,.F.,(4,2,2,2,2,2,4),(0.0946327170802488,0.104761312570622,
0.122042430928541,0.143220348291086,0.167141047893638,0.19192929334763,
0.192359096840082),.UNSPECIFIED.);
#874=B_SPLINE_CURVE_WITH_KNOTS('',3,(#43381,#43382,#43383,#43384,#43385,
#43386,#43387,#43388,#43389,#43390,#43391,#43392,#43393,#43394),
 .UNSPECIFIED.,.F.,.F.,(4,2,2,2,2,2,4),(-0.000411443668019523,0.,0.0275273122201118,
0.0519146118706548,0.0703314286321732,0.0856354757935221,0.0916008603165112),
 .UNSPECIFIED.);
#875=B_SPLINE_CURVE_WITH_KNOTS('',3,(#43404,#43405,#43406,#43407,#43408,
#43409,#43410,#43411,#43412,#43413,#43414,#43415,#43416,#43417,#43418,#43419,
#43420,#43421,#43422,#43423,#43424,#43425,#43426,#43427,#43428,#43429,#43430,
#43431,#43432,#43433,#43434,#43435,#43436,#43437,#43438,#43439,#43440,#43441,
#43442,#43443,#43444,#43445,#43446,#43447,#43448,#43449,#43450,#43451,#43452,
#43453,#43454,#43455,#43456,#43457,#43458,#43459,#43460,#43461,#43462,#43463,
#43464,#43465,#43466,#43467,#43468,#43469,#43470,#43471,#43472,#43473,#43474,
#43475,#43476,#43477,#43478,#43479,#43480,#43481,#43482,#43483,#43484,#43485,
#43486,#43487,#43488,#43489,#43490,#43491,#43492,#43493,#43494,#43495,#43496,
#43497,#43498,#43499,#43500,#43501,#43502,#43503,#43504,#43505,#43506,#43507,
#43508,#43509,#43510,#43511,#43512,#43513,#43514,#43515,#43516,#43517,#43518,
#43519,#43520,#43521,#43522,#43523,#43524,#43525,#43526,#43527,#43528,#43529,
#43530,#43531,#43532,#43533,#43534,#43535,#43536,#43537,#43538,#43539,#43540,
#43541,#43542,#43543,#43544,#43545,#43546,#43547,#43548),.UNSPECIFIED.,
 .F.,.F.,(4,3,3,3,3,3,3,3,3,3,3,3,3,3,3,3,3,3,3,3,3,3,3,3,3,3,3,3,3,3,3,
3,3,3,3,3,3,3,3,3,3,3,3,3,3,3,3,3,4),(0.,7.25281274128516E-5,0.000100260712346105,
0.000145056254825703,0.000202140779546393,0.000290112509651402,0.000305551005043421,
0.000326376573357828,0.000331630115588394,0.000357792042008772,0.000362640637064254,
0.000410099908754193,0.000435168764477103,0.000507696891889952,0.000514262478642334,
0.000580225019302801,0.000617529589805025,0.00065275314671565,0.00066867663759029,
0.000689017210422073,0.000694078722306658,0.000719282121091699,0.000725281274128496,
0.000797809401541343,0.000817729131006324,0.00087033752895419,0.000906601592660614,
0.000911548617891743,0.000924733624513829,0.000934113589543727,0.000942865656367043,
0.000956289830416614,0.000979129720073469,0.000999397033360985,0.00101539378377989,
0.00104069347247581,0.00105165784748632,0.00106059531852788,0.00106072386341293,
0.00106978987933953,0.00107035367576909,0.00108001823510808,0.00108792191119275,
0.00111511995897257,0.0011295215242621,0.00113889549736231,0.00114231800675239,
0.00115419999406486,0.0011604500386056),.UNSPECIFIED.);
#876=B_SPLINE_CURVE_WITH_KNOTS('',3,(#43733,#43734,#43735,#43736,#43737,
#43738,#43739,#43740,#43741,#43742),.UNSPECIFIED.,.F.,.F.,(4,2,2,2,4),(-0.112036818610838,
-0.0880588875106408,-0.0481932450937528,0.,0.000430202592559268),
 .UNSPECIFIED.);
#877=B_SPLINE_CURVE_WITH_KNOTS('',3,(#43770,#43771,#43772,#43773,#43774,
#43775,#43776,#43777,#43778,#43779),.UNSPECIFIED.,.F.,.F.,(4,2,2,2,4),(0.299155723157873,
0.33592702742144,0.373117039271119,0.410786177696965,0.448805976438876),
 .UNSPECIFIED.);
#878=B_SPLINE_CURVE_WITH_KNOTS('',3,(#43824,#43825,#43826,#43827,#43828,
#43829,#43830,#43831,#43832,#43833),.UNSPECIFIED.,.F.,.F.,(4,2,2,2,4),(-0.150773602000823,
-0.131921867952132,-0.113070133903442,-0.0942115691388773,-0.0753530043743127),
 .UNSPECIFIED.);
#879=B_SPLINE_CURVE_WITH_KNOTS('',3,(#43834,#43835,#43836,#43837,#43838,
#43839,#43840,#43841,#43842,#43843),.UNSPECIFIED.,.F.,.F.,(4,2,2,2,4),(-0.226162872426322,
-0.207310338477511,-0.1884578045287,-0.169609037891303,-0.150760271253907),
 .UNSPECIFIED.);
#880=B_SPLINE_CURVE_WITH_KNOTS('',3,(#43846,#43847,#43848,#43849,#43850,
#43851,#43852,#43853,#43854,#43855,#43856,#43857),.UNSPECIFIED.,.F.,.F.,
(4,2,2,2,2,4),(-0.185807739244323,-0.185439968351168,-0.153680951419909,
-0.128893958592289,-0.110891637254666,-0.0965169641148303),
 .UNSPECIFIED.);
#881=B_SPLINE_CURVE_WITH_KNOTS('',3,(#43858,#43859,#43860,#43861,#43862,
#43863,#43864,#43865,#43866,#43867,#43868,#43869,#43870,#43871,#43872,#43873),
 .UNSPECIFIED.,.F.,.F.,(4,2,2,2,2,2,2,4),(-0.000448819179353507,2.36681334253586E-15,
0.0230636769571239,0.0450898293250805,0.0666977239398038,0.0825811068581514,
0.096351648403139,0.0963708477819653),.UNSPECIFIED.);
#882=B_SPLINE_CURVE_WITH_KNOTS('',3,(#43876,#43877,#43878,#43879,#43880,
#43881,#43882,#43883,#43884,#43885,#43886,#43887,#43888,#43889),
 .UNSPECIFIED.,.F.,.F.,(4,2,2,2,2,2,4),(0.0936926976814215,0.108568843397411,
0.125272597642247,0.146759187794151,0.166551065492561,0.187385395362841,
0.187824844805022),.UNSPECIFIED.);
#883=B_SPLINE_CURVE_WITH_KNOTS('',3,(#43892,#43893,#43894,#43895,#43896,
#43897,#43898,#43899,#43900,#43901,#43902,#43903,#43904,#43905),
 .UNSPECIFIED.,.F.,.F.,(4,2,2,2,2,2,4),(-0.0939314403057516,-0.079108380427945,
-0.0624459947612743,-0.0409578088889437,-0.021014451885627,0.,0.000441387027955698),
 .UNSPECIFIED.);
#884=B_SPLINE_CURVE_WITH_KNOTS('',3,(#43907,#43908,#43909,#43910,#43911,
#43912),.UNSPECIFIED.,.F.,.F.,(4,2,4),(-0.0864860550818585,-0.0617458959675404,
0.),.UNSPECIFIED.);
#885=B_SPLINE_CURVE_WITH_KNOTS('',3,(#43919,#43920,#43921,#43922,#43923,
#43924,#43925,#43926),.UNSPECIFIED.,.F.,.F.,(4,2,2,4),(0.,0.0332644074051895,
0.0665288148103791,0.0864490647425511),.UNSPECIFIED.);
#886=B_SPLINE_CURVE_WITH_KNOTS('',3,(#43927,#43928,#43929,#43930,#43931,
#43932,#43933,#43934),.UNSPECIFIED.,.F.,.F.,(4,2,2,4),(0.292643145412176,
0.312563395344359,0.345827802749548,0.379092210154738),.UNSPECIFIED.);
#887=B_SPLINE_CURVE_WITH_KNOTS('',3,(#43939,#43940,#43941,#43942,#43943,
#43944,#43945,#43946,#43947,#43948,#43949,#43950,#43951,#43952,#43953,#43954,
#43955,#43956,#43957,#43958,#43959,#43960,#43961,#43962,#43963,#43964,#43965,
#43966,#43967,#43968,#43969,#43970,#43971,#43972,#43973,#43974),
 .UNSPECIFIED.,.F.,.F.,(4,1,2,2,1,1,2,2,2,1,1,1,2,2,1,1,1,2,2,2,1,1,1,4),
(8.26379378955844E-9,9.84772534748752E-5,0.00019695450694975,0.000246193133687188,
0.000295431760424625,0.0003939090138995,0.000492386267374374,0.000541624894111811,
0.000566244207480527,0.000590863520849243,0.000689340774324121,0.000787818027798999,
0.000886295281273877,0.000910914594642603,0.00093553390801133,0.000984772534748781,
0.00108324978822369,0.0011817270416986,0.00123096566843606,0.00125558498180478,
0.00128020429517351,0.00137868154864839,0.00147715880212328,0.00157563605559816),
 .UNSPECIFIED.);
#888=B_SPLINE_CURVE_WITH_KNOTS('',3,(#44219,#44220,#44221,#44222,#44223,
#44224,#44225,#44226,#44227,#44228,#44229,#44230,#44231,#44232),
 .UNSPECIFIED.,.F.,.F.,(4,2,2,2,2,2,4),(0.0980600308863261,0.111872145553039,
0.127734088362621,0.149209172354546,0.171902467951158,0.196120061772115,
0.196592003096005),.UNSPECIFIED.);
#889=B_SPLINE_CURVE_WITH_KNOTS('',3,(#44233,#44234,#44235,#44236,#44237,
#44238,#44239,#44240,#44241,#44242,#44243,#44244,#44245,#44246),
 .UNSPECIFIED.,.F.,.F.,(4,2,2,2,2,2,4),(-0.0919962992060375,-0.0866822297910484,
-0.0715424159762288,-0.0533700787866219,-0.0291975579830104,0.,0.000414145167341223),
 .UNSPECIFIED.);
#890=B_SPLINE_CURVE_WITH_KNOTS('',3,(#44248,#44249,#44250,#44251,#44252,
#44253,#44254,#44255,#44256,#44257,#44258,#44259,#44260,#44261),
 .UNSPECIFIED.,.F.,.F.,(4,2,2,2,2,2,4),(-0.000473267087033522,0.,0.024346315423422,
0.0471447393419604,0.0686144817737718,0.0844484317067967,0.0982274249930373),
 .UNSPECIFIED.);
#891=B_SPLINE_CURVE_WITH_KNOTS('',3,(#44262,#44263,#44264,#44265,#44266,
#44267,#44268,#44269,#44270,#44271,#44272,#44273,#44274,#44275),
 .UNSPECIFIED.,.F.,.F.,(4,2,2,2,2,2,4),(-0.211473737795484,-0.210980472033705,
-0.177081462686025,-0.148068102900271,-0.126207979465772,-0.108019352485251,
-0.101286341673499),.UNSPECIFIED.);
#892=B_SPLINE_CURVE_WITH_KNOTS('',3,(#44363,#44364,#44365,#44366,#44367,
#44368,#44369,#44370,#44371,#44372,#44373,#44374,#44375,#44376),
 .UNSPECIFIED.,.F.,.F.,(4,2,2,2,2,2,4),(-0.19692811707828,-0.196454849991217,
-0.172108534567229,-0.149310110648075,-0.127840368215671,-0.112006418282226,
-0.0982274249956043),.UNSPECIFIED.);
#893=B_SPLINE_CURVE_WITH_KNOTS('',3,(#44377,#44378,#44379,#44380,#44381,
#44382,#44383,#44384,#44385,#44386,#44387,#44388,#44389,#44390),
 .UNSPECIFIED.,.F.,.F.,(4,2,2,2,2,2,4),(-0.0983962336263429,-0.0846504542685971,
-0.0688446450995894,-0.0473804831279508,-0.0244761756223594,0.,0.000474604118846155),
 .UNSPECIFIED.);
#894=B_SPLINE_CURVE_WITH_KNOTS('',3,(#44394,#44395,#44396,#44397,#44398,
#44399,#44400,#44401,#44402,#44403,#44404,#44405,#44406,#44407),
 .UNSPECIFIED.,.F.,.F.,(4,2,2,2,2,2,4),(-0.21147373779364,-0.210980472031872,
-0.177081462684556,-0.148068102899106,-0.126207979464849,-0.108019352484536,
-0.101286341672861),.UNSPECIFIED.);
#895=B_SPLINE_CURVE_WITH_KNOTS('',3,(#44409,#44410,#44411,#44412,#44413,
#44414,#44415,#44416,#44417,#44418,#44419,#44420),.UNSPECIFIED.,.F.,.F.,
(4,2,2,2,2,4),(0.319067164078173,0.339664273857546,0.372500022353856,0.411302550267559,
0.451625546677781,0.452232637057266),.UNSPECIFIED.);
#896=B_SPLINE_CURVE_WITH_KNOTS('',3,(#44539,#44540,#44541,#44542,#44543,
#44544,#44545,#44546,#44547,#44548),.UNSPECIFIED.,.F.,.F.,(4,2,2,2,4),(0.22713486148052,
0.24601821426655,0.264901567052579,0.283737456690072,0.302573346327564),
 .UNSPECIFIED.);
#897=B_SPLINE_CURVE_WITH_KNOTS('',3,(#44552,#44553,#44554,#44555,#44556,
#44557,#44558,#44559,#44560,#44561),.UNSPECIFIED.,.F.,.F.,(4,2,2,2,4),(-0.151286623693373,
-0.132450734062243,-0.113614844431112,-0.0947314916401544,-0.0758481388491969),
 .UNSPECIFIED.);
#898=B_SPLINE_CURVE_WITH_KNOTS('',3,(#44593,#44594,#44595,#44596,#44597,
#44598,#44599,#44600,#44601,#44602),.UNSPECIFIED.,.F.,.F.,(4,2,2,2,4),(0.227134861433275,
0.246018214232104,0.264901567030932,0.283737456679245,0.302573346327559),
 .UNSPECIFIED.);
#899=B_SPLINE_CURVE_WITH_KNOTS('',3,(#44606,#44607,#44608,#44609,#44610,
#44611,#44612,#44613,#44614,#44615),.UNSPECIFIED.,.F.,.F.,(4,2,2,2,4),(-0.151286623693374,
-0.132450734061232,-0.113614844429089,-0.0947314916371198,-0.0758481388451503),
 .UNSPECIFIED.);
#900=B_SPLINE_CURVE_WITH_KNOTS('',3,(#44623,#44624,#44625,#44626,#44627,
#44628,#44629,#44630,#44631,#44632),.UNSPECIFIED.,.F.,.F.,(4,2,2,2,4),(-0.075438484844178,
-0.0565551320532202,-0.0376717792622623,-0.0188358896311301,2.13717932240343E-15),
 .UNSPECIFIED.);
#901=B_SPLINE_CURVE_WITH_KNOTS('',3,(#44636,#44637,#44638,#44639,#44640,
#44641,#44642,#44643,#44644,#44645),.UNSPECIFIED.,.F.,.F.,(4,2,2,2,4),(1.23169706186427E-15,
0.0188358896365198,0.0376717792730385,0.056555132060041,0.0754384848470435),
 .UNSPECIFIED.);
#902=B_SPLINE_CURVE_WITH_KNOTS('',3,(#44665,#44666,#44667,#44668,#44669,
#44670,#44671,#44672,#44673,#44674),.UNSPECIFIED.,.F.,.F.,(4,2,2,2,4),(-0.075438484902782,
-0.0565551320981278,-0.0376717792934735,-0.0188358896467368,0.),
 .UNSPECIFIED.);
#903=B_SPLINE_CURVE_WITH_KNOTS('',3,(#44678,#44679,#44680,#44681,#44682,
#44683,#44684,#44685,#44686,#44687),.UNSPECIFIED.,.F.,.F.,(4,2,2,2,4),(-2.21579007906029E-15,
0.01883588963867,0.0376717792773423,0.0565551320645541,0.0754384848517659),
 .UNSPECIFIED.);
#904=B_SPLINE_CURVE_WITH_KNOTS('',3,(#44704,#44705,#44706,#44707,#44708,
#44709,#44710,#44711,#44712,#44713),.UNSPECIFIED.,.F.,.F.,(4,2,2,2,4),(0.226757476774398,
0.245624555668826,0.264491634563253,0.283327009974748,0.302162385386242),
 .UNSPECIFIED.);
#905=B_SPLINE_CURVE_WITH_KNOTS('',3,(#44717,#44718,#44719,#44720,#44721,
#44722,#44723,#44724,#44725,#44726),.UNSPECIFIED.,.F.,.F.,(4,2,2,2,4),(-0.15108117139346,
-0.132245795981966,-0.113410420570472,-0.0945433416760444,-0.0756762627816166),
 .UNSPECIFIED.);
#906=B_SPLINE_CURVE_WITH_KNOTS('',3,(#44734,#44735,#44736,#44737,#44738,
#44739,#44740,#44741,#44742,#44743),.UNSPECIFIED.,.F.,.F.,(4,2,2,2,4),(-0.226486122604629,
-0.207619043710201,-0.188751964815772,-0.169916589404278,-0.151081213992783),
 .UNSPECIFIED.);
#907=B_SPLINE_CURVE_WITH_KNOTS('',3,(#44747,#44748,#44749,#44750,#44751,
#44752,#44753,#44754,#44755,#44756),.UNSPECIFIED.,.F.,.F.,(4,2,2,2,4),(0.151081213992781,
0.169916589404275,0.18875196481577,0.207619043710198,0.226486122604627),
 .UNSPECIFIED.);
#908=B_SPLINE_CURVE_WITH_KNOTS('',3,(#44765,#44766,#44767,#44768,#44769,
#44770,#44771,#44772,#44773,#44774),.UNSPECIFIED.,.F.,.F.,(4,2,2,2,4),(0.226757476774397,
0.245624555668825,0.264491634563252,0.283327009974748,0.302162385386243),
 .UNSPECIFIED.);
#909=B_SPLINE_CURVE_WITH_KNOTS('',3,(#44778,#44779,#44780,#44781,#44782,
#44783,#44784,#44785,#44786,#44787),.UNSPECIFIED.,.F.,.F.,(4,2,2,2,4),(-0.151081213992782,
-0.132245838581287,-0.113410463169793,-0.0945433842753652,-0.0756763053809372),
 .UNSPECIFIED.);
#910=B_SPLINE_CURVE_WITH_KNOTS('',3,(#44795,#44796,#44797,#44798,#44799,
#44800,#44801,#44802,#44803,#44804),.UNSPECIFIED.,.F.,.F.,(4,2,2,2,4),(-0.226486080005305,
-0.207619001110877,-0.188751922216448,-0.169916546804955,-0.151081171393461),
 .UNSPECIFIED.);
#911=B_SPLINE_CURVE_WITH_KNOTS('',3,(#44808,#44809,#44810,#44811,#44812,
#44813,#44814,#44815,#44816,#44817),.UNSPECIFIED.,.F.,.F.,(4,2,2,2,4),(0.151081171393462,
0.169916546804955,0.188751922216448,0.207619001110876,0.226486080005304),
 .UNSPECIFIED.);
#912=B_SPLINE_CURVE_WITH_KNOTS('',3,(#45182,#45183,#45184,#45185,#45186,
#45187,#45188,#45189,#45190,#45191,#45192,#45193),.UNSPECIFIED.,.F.,.F.,
(4,2,2,2,2,4),(-1.51152287781019,-1.41955557636733,-1.32295309115156,-1.22686541559156,
-1.13077774003156,-1.03807141782941),.UNSPECIFIED.);
#913=B_SPLINE_CURVE_WITH_KNOTS('',3,(#45198,#45199,#45200,#45201,#45202,
#45203,#45204,#45205,#45206,#45207,#45208,#45209,#45210,#45211,#45212,#45213,
#45214,#45215),.UNSPECIFIED.,.F.,.F.,(4,2,2,2,2,2,2,2,4),(-1.03807141782941,
-1.03415356085079,-0.937529381670028,-0.8405054734841,-0.743481565298172,
-0.650733139326691,-0.55798471335521,-0.464768069683676,-0.459883804363485),
 .UNSPECIFIED.);
#914=B_SPLINE_CURVE_WITH_KNOTS('',3,(#45219,#45220,#45221,#45222,#45223,
#45224,#45225,#45226,#45227,#45228,#45229,#45230,#45231,#45232,#45233),
 .UNSPECIFIED.,.F.,.F.,(4,2,2,2,2,3,4),(-0.459883804363485,-0.371551426012142,
-0.278664247294852,-0.185777068577561,-0.0928885342887805,0.,0.0046338852898157),
 .UNSPECIFIED.);
#915=B_SPLINE_CURVE_WITH_KNOTS('',3,(#45236,#45237,#45238,#45239,#45240,
#45241,#45242,#45243,#45244,#45245,#45246,#45247,#45248,#45249,#45250,#45251,
#45252,#45253,#45254,#45255,#45256,#45257,#45258,#45259,#45260,#45261,#45262,
#45263,#45264,#45265,#45266),.UNSPECIFIED.,.F.,.F.,(4,2,2,3,2,2,2,2,2,2,
2,2,2,2,4),(-1.31063818840695,-1.05024518266218,-0.525122591331091,0.,0.312507098746615,
0.468760648119922,0.62501419749323,0.749593994182574,0.874173790871916,
0.966755699602937,1.05933760833396,1.15191951706498,1.244501425796,1.36908122248534,
1.43505508424711),.UNSPECIFIED.);
#916=B_SPLINE_CURVE_WITH_KNOTS('',3,(#45267,#45268,#45269,#45270,#45271,
#45272,#45273,#45274,#45275,#45276,#45277,#45278,#45279,#45280,#45281,#45282,
#45283,#45284,#45285,#45286,#45287,#45288,#45289,#45290,#45291,#45292),
 .UNSPECIFIED.,.F.,.F.,(4,2,2,2,2,2,2,2,2,2,2,2,4),(1.43505508424711,1.49366101917468,
1.64991456854799,1.8061681179213,2.11867521666791,2.64379780799901,3.1689203993301,
3.67271158289934,3.79227940354027,3.91184722418121,4.03141504482215,4.15098286546309,
4.39438104328756),.UNSPECIFIED.);
#917=B_SPLINE_CURVE_WITH_KNOTS('',3,(#45572,#45573,#45574,#45575,#45576,
#45577,#45578,#45579,#45580,#45581,#45582,#45583),.UNSPECIFIED.,.F.,.F.,
(4,2,2,2,2,4),(9.92264902769865E-7,0.0122814154766666,0.0227351808389828,
0.0425013028347888,0.0639899300112591,0.0846625935368686),.UNSPECIFIED.);
#918=B_SPLINE_CURVE_WITH_KNOTS('',3,(#45602,#45603,#45604,#45605,#45606,
#45607,#45608,#45609,#45610,#45611,#45612,#45613,#45614,#45615,#45616,#45617,
#45618,#45619,#45620,#45621,#45622,#45623,#45624,#45625,#45626,#45627,#45628,
#45629,#45630,#45631,#45632,#45633,#45634,#45635,#45636,#45637,#45638,#45639,
#45640,#45641,#45642,#45643,#45644,#45645,#45646,#45647,#45648,#45649,#45650,
#45651,#45652,#45653,#45654,#45655,#45656,#45657,#45658,#45659,#45660,#45661,
#45662,#45663,#45664,#45665,#45666,#45667,#45668,#45669,#45670,#45671,#45672,
#45673,#45674,#45675,#45676,#45677,#45678,#45679,#45680,#45681,#45682,#45683,
#45684,#45685,#45686,#45687,#45688,#45689,#45690,#45691,#45692,#45693,#45694,
#45695,#45696,#45697,#45698,#45699,#45700,#45701,#45702,#45703,#45704,#45705,
#45706,#45707,#45708,#45709,#45710,#45711,#45712,#45713,#45714,#45715,#45716,
#45717,#45718,#45719,#45720,#45721,#45722,#45723,#45724,#45725,#45726,#45727,
#45728,#45729,#45730,#45731,#45732,#45733,#45734,#45735,#45736,#45737,#45738,
#45739,#45740,#45741,#45742,#45743,#45744,#45745,#45746),.UNSPECIFIED.,
 .F.,.F.,(4,3,3,3,3,3,3,3,3,3,3,3,3,3,3,3,3,3,3,3,3,3,3,3,3,3,3,3,3,3,3,
3,3,3,3,3,3,3,3,3,3,3,3,3,3,3,3,3,4),(0.0054539128671712,0.00548380874985591,
0.00565888988694723,0.00577243026300616,0.00591674101958129,0.00595688595087576,
0.00598889639786886,0.00603110776681321,0.00606105177615643,0.00606817280695972,
0.00610520328963597,0.00625299641255915,0.00634967328930671,0.00654698557014318,
0.00663829480245699,0.00683895447912464,0.00692691631560727,0.00707122707218241,
0.00712902509780294,0.00714338245046997,0.00717946013961376,0.0072012572687105,
0.00721553782875754,0.00723732988878856,0.00727337941031582,0.0074173491882449,
0.00750415934190779,0.00770421253731256,0.00779278085505804,0.0079897749319241,
0.00808140236820829,0.00813211305141546,0.00820317794008171,0.00822571312478341,
0.00823868030383458,0.00827417239358472,0.00829786850307098,0.00837002388135854,
0.00855773776014578,0.00865864539450881,0.00884069465909997,0.00894726690765908,
0.00909157766423421,0.00912311752903997,0.00915838665328199,0.00916373304252177,
0.00919361503382806,0.00919981073166556,0.00923588842080934),
 .UNSPECIFIED.);
#919=B_SPLINE_CURVE_WITH_KNOTS('',3,(#45748,#45749,#45750,#45751),
 .UNSPECIFIED.,.F.,.F.,(4,4),(1.4574000303393E-16,0.0113332377793703),
 .UNSPECIFIED.);
#920=B_SPLINE_CURVE_WITH_KNOTS('',3,(#45753,#45754,#45755,#45756,#45757,
#45758,#45759,#45760,#45761,#45762,#45763,#45764,#45765,#45766,#45767,#45768,
#45769,#45770,#45771,#45772,#45773,#45774,#45775,#45776,#45777,#45778,#45779,
#45780,#45781,#45782,#45783,#45784,#45785,#45786,#45787,#45788,#45789,#45790,
#45791,#45792,#45793,#45794,#45795,#45796,#45797,#45798,#45799,#45800,#45801,
#45802,#45803,#45804,#45805,#45806,#45807,#45808,#45809,#45810,#45811,#45812,
#45813,#45814,#45815,#45816,#45817,#45818,#45819,#45820,#45821,#45822,#45823,
#45824,#45825,#45826,#45827,#45828,#45829,#45830,#45831,#45832,#45833,#45834,
#45835,#45836,#45837,#45838,#45839,#45840,#45841,#45842,#45843,#45844,#45845,
#45846,#45847,#45848,#45849,#45850,#45851,#45852,#45853,#45854,#45855,#45856,
#45857,#45858,#45859,#45860,#45861,#45862,#45863,#45864,#45865,#45866,#45867,
#45868,#45869,#45870,#45871,#45872,#45873,#45874,#45875,#45876,#45877,#45878,
#45879,#45880,#45881,#45882,#45883,#45884,#45885,#45886,#45887,#45888,#45889,
#45890,#45891,#45892,#45893,#45894,#45895,#45896,#45897,#45898,#45899,#45900,
#45901,#45902,#45903,#45904,#45905,#45906,#45907,#45908,#45909,#45910,#45911,
#45912,#45913,#45914,#45915,#45916,#45917,#45918,#45919,#45920,#45921,#45922,
#45923,#45924,#45925,#45926,#45927,#45928,#45929,#45930,#45931,#45932,#45933,
#45934,#45935,#45936,#45937,#45938,#45939,#45940,#45941,#45942,#45943,#45944,
#45945,#45946,#45947,#45948,#45949,#45950,#45951,#45952,#45953,#45954,#45955,
#45956,#45957,#45958,#45959,#45960,#45961,#45962,#45963,#45964,#45965,#45966,
#45967,#45968,#45969,#45970,#45971,#45972,#45973,#45974,#45975,#45976,#45977,
#45978,#45979,#45980,#45981,#45982,#45983,#45984,#45985,#45986,#45987,#45988,
#45989,#45990,#45991,#45992,#45993,#45994,#45995,#45996,#45997,#45998,#45999,
#46000,#46001,#46002,#46003,#46004,#46005,#46006,#46007,#46008,#46009,#46010,
#46011,#46012,#46013,#46014,#46015,#46016,#46017,#46018,#46019,#46020,#46021,
#46022,#46023,#46024,#46025,#46026,#46027,#46028,#46029,#46030,#46031,#46032),
 .UNSPECIFIED.,.F.,.F.,(4,3,3,3,3,3,3,3,3,3,3,3,3,3,3,3,3,3,3,3,3,3,3,3,
3,3,3,3,3,3,3,3,3,3,3,3,3,3,3,3,3,3,3,3,3,3,3,3,3,3,3,3,3,3,3,3,3,3,3,3,
3,3,3,3,3,3,3,3,3,3,3,3,3,3,3,3,3,3,3,3,3,3,3,3,3,3,3,3,3,3,3,3,3,4),(0.,
9.06394666082451E-5,9.84186019154758E-5,0.00018127893321649,0.000196344891157804,
0.000271918399824735,0.000293789584677031,0.000317238133128857,0.000339897999780917,
0.000342304633973775,0.000362557866432978,0.000390537263439263,0.000453197333041227,
0.000486049915227595,0.000543836799649477,0.000580320870217935,0.000626990715264167,
0.000634476266257726,0.00065020402445471,0.000657136132909784,0.000673323081798869,
0.000679795999561842,0.000725115732865958,0.000764841371010614,0.000815755199474182,
0.0008548576554711,0.000906394666082406,0.000929054532734454,0.000943371418524607,
0.000951714399386503,0.000997034132690586,0.00103051440248908,0.00108767359929875,
0.0011164662936885,0.00117831306590692,0.00120123217101674,0.001223632799211,
0.00124316188010154,0.00124629266586303,0.00126895253251506,0.00128486511176821,
0.00135959199912321,0.00136785720613342,0.00145023146573136,0.00145030648535944,
0.0014728913323834,0.00149133041292132,0.00149555119903544,0.00151188331859317,
0.00151821106568749,0.001532528558112,0.00154087093233953,0.00161565551529423,
0.00163151039894771,0.00169958627364771,0.00172214986555588,0.00176746959885996,
0.00178431737336985,0.00179012946551201,0.00181278933216405,0.00182701790521884,
0.00187007299327093,0.00190342879877218,0.00195723834581456,0.00199406826538032,
0.00204581493813314,0.00208470773198846,0.00209063844107407,0.00210736759864049,
0.00213002746529252,0.00213582758039994,0.00217534719859659,0.00222729219943231,
0.00226598666520473,0.00232019847227704,0.00235662613181287,0.0023672014340626,
0.00240194586511693,0.00241457759770203,0.00242460573176897,0.00244726559842101,
0.00251014587586458,0.00253790506502916,0.00260663317312218,0.00262854453163731,
0.00270404516267542,0.00271918399824546,0.00272854743294039,0.00274184386489749,
0.00275310480366504,0.00276450373154952,0.00280223551954616,0.00280982346485358,
0.00290046293146171),.UNSPECIFIED.);
#921=B_SPLINE_CURVE_WITH_KNOTS('',3,(#46034,#46035,#46036,#46037),
 .UNSPECIFIED.,.F.,.F.,(4,4),(0.,0.011206889852584),.UNSPECIFIED.);
#922=B_SPLINE_CURVE_WITH_KNOTS('',3,(#46039,#46040,#46041,#46042,#46043,
#46044,#46045,#46046,#46047,#46048,#46049,#46050,#46051,#46052,#46053,#46054,
#46055,#46056,#46057,#46058,#46059,#46060,#46061,#46062,#46063,#46064,#46065,
#46066,#46067,#46068,#46069,#46070,#46071,#46072,#46073,#46074,#46075,#46076,
#46077,#46078,#46079,#46080,#46081,#46082,#46083,#46084),.UNSPECIFIED.,
 .F.,.F.,(4,2,1,2,2,2,2,2,2,1,2,2,2,2,1,1,2,2,2,2,2,2,1,1,2,4),(0.000392395285594788,
0.000660337424393816,0.000794308909059438,0.00086129465139225,0.000928280393725061,
0.00119622336305629,0.00146416633238753,0.00173210930171876,0.00179909504405157,
0.00186608078638437,0.00200005227104998,0.0022679952403812,0.00253593820971242,
0.00256943108087883,0.00260292395204523,0.00266990969437803,0.00280388117904364,
0.00307182414837484,0.00333976711770605,0.00340675286003885,0.00347373860237165,
0.00350723147353805,0.00354072434470446,0.00360771008703726,0.00387565305636847,
0.0040894670158376),.UNSPECIFIED.);
#923=B_SPLINE_CURVE_WITH_KNOTS('',3,(#46090,#46091,#46092,#46093,#46094,
#46095,#46096,#46097),.UNSPECIFIED.,.F.,.F.,(4,3,1,4),(0.000295555998119065,
0.00492308001881893,0.00630130897220404,0.00659646431556111),
 .UNSPECIFIED.);
#924=B_SPLINE_CURVE_WITH_KNOTS('',3,(#46101,#46102,#46103,#46104,#46105,
#46106,#46107,#46108,#46109,#46110),.UNSPECIFIED.,.F.,.F.,(4,3,3,4),(-0.000295155343349986,
1.44198888940572E-17,0.0051169388442874,0.00600575297407752),
 .UNSPECIFIED.);
#925=B_SPLINE_CURVE_WITH_KNOTS('',3,(#46113,#46114,#46115,#46116,#46117,
#46118,#46119,#46120,#46121,#46122,#46123,#46124,#46125,#46126,#46127,#46128,
#46129,#46130,#46131,#46132,#46133,#46134,#46135,#46136,#46137,#46138,#46139,
#46140,#46141,#46142,#46143,#46144,#46145,#46146,#46147,#46148,#46149,#46150,
#46151,#46152,#46153),.UNSPECIFIED.,.F.,.F.,(4,2,2,2,1,2,2,2,2,2,2,1,1,
1,1,1,2,1,2,2,1,1,1,1,2,4),(0.0040894670158376,0.00414359602569968,0.00441153899503089,
0.0044785247373637,0.0045455104796965,0.00467948196436211,0.00494742493369333,
0.00521536790302455,0.00548331087235577,0.00561728235702139,0.00568426809935419,
0.005751253841687,0.00601919681101826,0.00628713978034951,0.00655508274968077,
0.00682302571901203,0.00709096868834328,0.00722494017300891,0.00729192591534172,
0.00735891165767452,0.00762685462700575,0.00789479759633698,0.0081627405656682,
0.00843068353499943,0.00869862650433066,0.00896656947366188),
 .UNSPECIFIED.);
#926=B_SPLINE_CURVE_WITH_KNOTS('',3,(#46155,#46156,#46157,#46158,#46159,
#46160,#46161,#46162,#46163,#46164,#46165,#46166,#46167,#46168,#46169,#46170,
#46171,#46172,#46173,#46174,#46175,#46176,#46177,#46178,#46179,#46180,#46181,
#46182,#46183,#46184,#46185,#46186,#46187,#46188,#46189,#46190,#46191,#46192,
#46193,#46194,#46195,#46196,#46197),.UNSPECIFIED.,.F.,.F.,(4,3,3,3,3,3,
3,3,3,3,3,3,3,3,4),(0.,0.000117052501055883,0.000153349582659865,0.000161023794644849,
0.0002300243739898,0.000239696739155573,0.000268361769654766,0.000317031808608993,
0.000383373956649677,0.000460048747979621,0.000467463358429797,0.000498386143644593,
0.000523040524368854,0.000536723539309575,0.000613398330639558),
 .UNSPECIFIED.);
#927=B_SPLINE_CURVE_WITH_KNOTS('',3,(#46198,#46199,#46200,#46201,#46202,
#46203,#46204,#46205,#46206,#46207,#46208,#46209,#46210,#46211,#46212,#46213,
#46214,#46215,#46216,#46217,#46218,#46219,#46220,#46221,#46222,#46223,#46224,
#46225,#46226,#46227,#46228,#46229,#46230,#46231,#46232,#46233,#46234,#46235,
#46236,#46237,#46238,#46239,#46240,#46241,#46242,#46243,#46244,#46245,#46246,
#46247,#46248,#46249,#46250,#46251,#46252,#46253,#46254,#46255,#46256,#46257,
#46258,#46259,#46260,#46261,#46262,#46263,#46264,#46265,#46266,#46267,#46268,
#46269,#46270,#46271,#46272,#46273,#46274,#46275,#46276,#46277,#46278,#46279,
#46280,#46281,#46282,#46283,#46284,#46285,#46286,#46287,#46288,#46289,#46290,
#46291,#46292,#46293,#46294,#46295,#46296,#46297,#46298,#46299,#46300,#46301,
#46302,#46303,#46304,#46305,#46306,#46307,#46308,#46309,#46310,#46311,#46312,
#46313,#46314,#46315,#46316,#46317,#46318,#46319,#46320,#46321,#46322,#46323,
#46324,#46325,#46326,#46327,#46328,#46329,#46330,#46331,#46332,#46333,#46334,
#46335,#46336,#46337,#46338,#46339),.UNSPECIFIED.,.F.,.F.,(4,3,3,3,3,3,
3,3,3,3,3,3,3,3,3,3,3,3,3,3,3,3,3,3,3,3,3,3,3,3,3,3,3,3,3,3,3,3,3,3,3,3,
3,3,3,3,3,4),(0.,0.000218348361755657,0.000288621513150416,0.000509762429138871,
0.000577243026300831,0.000649398404588435,0.000685476093732232,0.000721553782876029,
0.000757631472019826,0.000793709161163623,0.000865864539451206,0.00106157890238537,
0.00115448605260153,0.00136621152949033,0.00144310756575185,0.00151526294403943,
0.00158741832232702,0.00173172907890218,0.00193773404538904,0.00202035059205251,
0.00224290230807321,0.00230897210520284,0.00238112748349041,0.00245328286177799,
0.00259759361835315,0.00282626847197688,0.00288621513150347,0.00312835477281512,
0.00317483664465379,0.00342364710957266,0.00346345815780411,0.0034995358469479,
0.00353561353609168,0.00360776891437925,0.00375207967095438,0.00400768565379299,
0.00404070118410464,0.0042978895511761,0.00432932269725489,0.00458016139294931,
0.00461794421040514,0.00476225496698027,0.00479833265612405,0.00483441034526783,
0.00490656572355539,0.00516688963479163,0.00519518723670565,0.00545391286716091),
 .UNSPECIFIED.);
#928=B_SPLINE_CURVE_WITH_KNOTS('',3,(#46344,#46345,#46346,#46347,#46348,
#46349,#46350,#46351,#46352,#46353),.UNSPECIFIED.,.F.,.F.,(4,2,2,2,4),(-0.188504168620313,
-0.178198215106625,-0.166932202633752,-0.154946150113528,-0.14212773138048),
 .UNSPECIFIED.);
#929=B_SPLINE_CURVE_WITH_KNOTS('',3,(#46354,#46355,#46356,#46357,#46358,
#46359,#46360,#46361,#46362,#46363),.UNSPECIFIED.,.F.,.F.,(4,2,2,2,4),(-0.0468417359580142,
-0.0340233172249645,-0.0220372647047389,-0.0107712522318653,-0.000465298718183977),
 .UNSPECIFIED.);
#930=B_SPLINE_CURVE_WITH_KNOTS('',3,(#46372,#46373,#46374,#46375,#46376,
#46377,#46378,#46379,#46380,#46381,#46382,#46383,#46384,#46385,#46386,#46387,
#46388,#46389,#46390,#46391,#46392,#46393,#46394,#46395,#46396,#46397,#46398,
#46399,#46400,#46401,#46402,#46403,#46404,#46405,#46406,#46407,#46408,#46409,
#46410,#46411,#46412,#46413,#46414,#46415,#46416,#46417,#46418,#46419,#46420,
#46421,#46422,#46423,#46424,#46425,#46426,#46427,#46428,#46429,#46430,#46431,
#46432,#46433,#46434,#46435,#46436,#46437,#46438,#46439,#46440,#46441,#46442,
#46443,#46444,#46445,#46446,#46447,#46448,#46449,#46450,#46451,#46452,#46453,
#46454,#46455,#46456,#46457,#46458,#46459,#46460,#46461,#46462,#46463,#46464,
#46465,#46466,#46467,#46468,#46469,#46470,#46471,#46472,#46473,#46474,#46475,
#46476,#46477,#46478,#46479,#46480,#46481,#46482,#46483,#46484,#46485,#46486,
#46487,#46488,#46489,#46490,#46491,#46492,#46493,#46494,#46495,#46496,#46497,
#46498,#46499,#46500,#46501,#46502,#46503,#46504,#46505,#46506,#46507,#46508,
#46509,#46510,#46511,#46512,#46513,#46514,#46515,#46516,#46517,#46518,#46519,
#46520,#46521,#46522,#46523,#46524,#46525,#46526,#46527,#46528,#46529,#46530,
#46531,#46532,#46533,#46534,#46535,#46536,#46537,#46538,#46539,#46540,#46541,
#46542,#46543,#46544,#46545,#46546,#46547,#46548,#46549,#46550,#46551,#46552,
#46553,#46554,#46555,#46556,#46557,#46558,#46559,#46560,#46561,#46562,#46563,
#46564,#46565,#46566,#46567,#46568,#46569,#46570,#46571,#46572,#46573,#46574,
#46575,#46576,#46577,#46578,#46579,#46580,#46581,#46582,#46583,#46584,#46585,
#46586,#46587,#46588,#46589,#46590,#46591,#46592,#46593,#46594,#46595,#46596,
#46597,#46598,#46599,#46600,#46601,#46602,#46603,#46604,#46605,#46606,#46607,
#46608,#46609,#46610,#46611,#46612,#46613,#46614,#46615,#46616,#46617,#46618,
#46619,#46620,#46621,#46622,#46623,#46624,#46625,#46626,#46627,#46628,#46629,
#46630,#46631,#46632,#46633,#46634,#46635,#46636,#46637,#46638,#46639,#46640,
#46641,#46642,#46643,#46644,#46645,#46646,#46647,#46648,#46649,#46650,#46651,
#46652,#46653,#46654),.UNSPECIFIED.,.F.,.F.,(4,3,3,3,3,3,3,3,3,3,3,3,3,
3,3,3,3,3,3,3,3,3,3,3,3,3,3,3,3,3,3,3,3,3,3,3,3,3,3,3,3,3,3,3,3,3,3,3,3,
3,3,3,3,3,3,3,3,3,3,3,3,3,3,3,3,3,3,3,3,3,3,3,3,3,3,3,3,3,3,3,3,3,3,3,3,
3,3,3,3,3,3,3,3,3,4),(0.,0.0003242112872066,0.000357261792737838,0.000648422574413201,
0.000713397984116496,0.000972633861619801,0.00106849099687377,0.0012968451488264,
0.00142259046797538,0.001621056436033,0.00177571862495347,0.0017831620796363,
0.00186384905495805,0.00186421490143795,0.00190474131233878,0.0019452677232396,
0.00195192061876334,0.00212790648128734,0.00226947901044622,0.00247923627193231,
0.00259369029765284,0.00282972486348799,0.00291790158485946,0.00317934752697371,
0.00324211287206608,0.00352806077583578,0.0035663241592727,0.00370205576559277,
0.00372842980287601,0.00376895621377683,0.00378895854388717,0.00380948262467766,
0.00387581262257363,0.00389053544647929,0.00421474673368583,0.00422290205403573,
0.00453895802089236,0.00456943462611516,0.0048631693080989,0.00491535430262632,
0.00508806280169499,0.00517434618899021,0.00518738059530543,0.00522790700620624,
0.00526059483948565,0.00526843341710705,0.00534948623890867,0.00551159188251191,
0.00560569480955727,0.00583580316971839,0.00595096223417242,0.00616001445692487,
0.00629637362108293,0.00632212010052811,0.00633956008149765,0.00636264651142892,
0.00638274886077817,0.00640317292232973,0.00646917189092978,0.00648422574413136,
0.00664226599303563,0.00680843703133785,0.00698941739492064,0.00713264831854435,
0.0073378495654889,0.00745685960575085,0.00751255500574631,0.00753791242755247,
0.00757843883845328,0.00760003330101165,0.00761896524935409,0.00768763257202629,
0.00778107089295735,0.00803922882622409,0.00810528218016386,0.00839270938616917,
0.00842949346737037,0.00857015221794751,0.00859159911097363,0.00861458669111193,
0.00865905017453961,0.00867265193277526,0.00874805663922665,0.00875370475457689,
0.00907791604178338,0.00910510377824634,0.00940212732898988,0.00946374650435997,
0.00964367022755659,0.00972633861619637,0.00973375433433046,0.00982383413264779,
0.0100505499034029,0.0101833725565308,0.0103747611906094),.UNSPECIFIED.);
#931=B_SPLINE_CURVE_WITH_KNOTS('',3,(#46658,#46659,#46660,#46661,#46662,
#46663,#46664,#46665,#46666,#46667,#46668,#46669,#46670,#46671,#46672,#46673,
#46674,#46675,#46676,#46677,#46678,#46679),.UNSPECIFIED.,.F.,.F.,(4,2,2,
2,2,2,2,2,2,2,4),(-0.516489735213594,-0.403297365402408,-0.304637803925453,
-0.258291991281017,-0.235867650221037,-0.22650069343662,-0.22227817689503,
-0.203792144791807,-0.176538654710716,-0.119127477076588,-5.65372251348784E-7),
 .UNSPECIFIED.);
#932=B_SPLINE_CURVE_WITH_KNOTS('',3,(#46683,#46684,#46685,#46686,#46687,
#46688,#46689,#46690,#46691,#46692,#46693,#46694,#46695,#46696,#46697,#46698,
#46699,#46700,#46701,#46702,#46703,#46704,#46705,#46706,#46707,#46708,#46709,
#46710,#46711,#46712,#46713,#46714,#46715,#46716,#46717,#46718,#46719,#46720,
#46721,#46722,#46723,#46724,#46725,#46726,#46727,#46728,#46729,#46730,#46731,
#46732,#46733,#46734,#46735,#46736,#46737,#46738,#46739,#46740,#46741,#46742,
#46743,#46744,#46745,#46746,#46747,#46748,#46749,#46750,#46751,#46752,#46753,
#46754,#46755,#46756,#46757,#46758,#46759,#46760,#46761,#46762,#46763,#46764,
#46765,#46766,#46767,#46768,#46769,#46770,#46771,#46772,#46773,#46774,#46775,
#46776,#46777,#46778,#46779,#46780,#46781,#46782,#46783,#46784,#46785,#46786,
#46787,#46788,#46789,#46790,#46791,#46792,#46793,#46794,#46795,#46796,#46797,
#46798,#46799,#46800,#46801,#46802,#46803,#46804,#46805,#46806,#46807,#46808,
#46809,#46810,#46811,#46812,#46813,#46814,#46815,#46816,#46817,#46818,#46819,
#46820,#46821,#46822,#46823,#46824,#46825,#46826,#46827,#46828,#46829,#46830,
#46831,#46832,#46833,#46834,#46835,#46836,#46837,#46838,#46839,#46840,#46841,
#46842,#46843,#46844,#46845,#46846,#46847,#46848,#46849,#46850,#46851,#46852,
#46853,#46854,#46855,#46856,#46857,#46858,#46859,#46860,#46861,#46862,#46863,
#46864,#46865,#46866,#46867,#46868,#46869,#46870,#46871,#46872,#46873,#46874,
#46875,#46876,#46877,#46878,#46879,#46880,#46881,#46882,#46883,#46884,#46885,
#46886,#46887,#46888,#46889,#46890,#46891,#46892,#46893,#46894,#46895,#46896,
#46897,#46898,#46899,#46900,#46901,#46902,#46903,#46904,#46905,#46906,#46907,
#46908,#46909,#46910,#46911,#46912,#46913,#46914,#46915,#46916,#46917,#46918,
#46919,#46920,#46921,#46922,#46923,#46924,#46925,#46926,#46927,#46928,#46929,
#46930,#46931,#46932,#46933,#46934,#46935,#46936,#46937,#46938,#46939,#46940,
#46941,#46942,#46943,#46944,#46945,#46946,#46947,#46948,#46949,#46950,#46951,
#46952,#46953,#46954,#46955,#46956,#46957,#46958,#46959,#46960,#46961,#46962,
#46963,#46964,#46965,#46966,#46967,#46968,#46969,#46970,#46971,#46972,#46973,
#46974,#46975,#46976,#46977,#46978,#46979,#46980,#46981,#46982,#46983,#46984,
#46985,#46986,#46987,#46988,#46989,#46990,#46991,#46992,#46993,#46994,#46995,
#46996,#46997,#46998,#46999,#47000,#47001,#47002,#47003,#47004,#47005,#47006,
#47007,#47008,#47009,#47010,#47011,#47012,#47013,#47014,#47015,#47016,#47017,
#47018,#47019,#47020,#47021,#47022,#47023,#47024,#47025),.UNSPECIFIED.,
 .F.,.F.,(4,3,3,3,3,3,3,3,3,3,3,3,3,3,3,3,3,3,3,3,3,3,3,3,3,3,3,3,3,3,3,
3,3,3,3,3,3,3,3,3,3,3,3,3,3,3,3,3,3,3,3,3,3,3,3,3,3,3,3,3,3,3,3,3,3,3,3,
3,3,3,3,3,3,3,3,3,3,3,3,3,3,3,3,3,3,3,3,3,3,3,3,3,3,3,3,3,3,3,3,3,3,3,3,
3,3,3,3,3,3,3,3,3,3,3,4),(0.,0.000559340172070426,0.00056312127745191,0.00111868034414085,
0.00117480882670147,0.00139835043017606,0.00148111639279807,0.00153818547319366,
0.00160810299470246,0.0016343904416067,0.00167802051621126,0.00178762749494104,
0.00223736068828162,0.00239897267727689,0.00279670086035198,0.00300768662511807,
0.00335604103242234,0.00361373793821833,0.00363571111845751,0.00376481945685295,
0.0037755461614751,0.00384029321466327,0.00384546368298389,0.00391538120449268,
0.00391572188407732,0.00421697465550928,0.00447472137656305,0.00481726522761212,
0.00503406154863342,0.00511629473858952,0.00531373163466861,0.00541456290638466,
0.00559340172070379,0.00571204633238695,0.00573323676372139,0.00580315428523019,
0.00583811304598459,0.00586048502912534,0.00587307180673899,0.00600876663145698,
0.00615274189277417,0.00630500853253195,0.00660082053734943,0.00671208206484454,
0.00689619939885552,0.00719113780032637,0.00727142223691492,0.00741125727993251,
0.00748117480144131,0.00748562537787358,0.0075161335621957,0.0075510923229501,
0.0075591756922752,0.00763271703837717,0.0077798197594622,0.00783076240898527,
0.00807404583962471,0.00811043249502045,0.0083682956412184,0.00839010258105563,
0.00894944275312598,0.0089568174998829,0.00908927779614357,0.00910394297613539,
0.00915919531765236,0.00917751112674336,0.00922911283916116,0.00925109949730556,
0.00950878292519633,0.00954566299720578,0.0100681230972667,0.0101357118688264,
0.010627463269337,0.0107268460053846,0.0107672983123546,0.0108372158338634,
0.0108747847708707,0.0109071333553722,0.0110227987810239,0.0111868034414074,
0.0113191040911945,0.0114664735274426,0.0116063085704602,0.0116157576196813,
0.011676226091969,0.011689973073376,0.0117461436134777,0.0117642110435597,
0.0119127713350278,0.0123054837855481,0.0125080251066784,0.0128648239576184,
0.013104832388234,0.0134241641296888,0.0137030875195115,0.0139835043017591,
0.014302741201141,0.0145428444738295,0.0146030956561195,0.0146826795168471,
0.0147533972581463,0.0148225145598647,0.0149038256869558,0.0151021846458999,
0.0155067400228327,0.0156615248179702,0.0161116197724483,0.0162208649900406,
0.0167185606475561,0.016780205162111,0.0173277427187631,0.0173395453341813,
0.0176334296012555,0.0177861596802748,0.0178988855062517),.UNSPECIFIED.);
#933=B_SPLINE_CURVE_WITH_KNOTS('',3,(#47040,#47041,#47042,#47043,#47044,
#47045,#47046,#47047,#47048,#47049,#47050,#47051,#47052,#47053,#47054,#47055,
#47056,#47057,#47058,#47059,#47060,#47061,#47062,#47063,#47064,#47065,#47066,
#47067,#47068,#47069,#47070,#47071,#47072,#47073,#47074,#47075,#47076,#47077,
#47078,#47079,#47080,#47081,#47082,#47083,#47084,#47085,#47086,#47087,#47088,
#47089,#47090,#47091,#47092,#47093,#47094,#47095,#47096,#47097,#47098,#47099,
#47100,#47101,#47102,#47103,#47104,#47105,#47106,#47107,#47108,#47109,#47110,
#47111,#47112,#47113,#47114,#47115,#47116,#47117,#47118,#47119,#47120,#47121,
#47122,#47123,#47124,#47125,#47126,#47127,#47128,#47129,#47130,#47131,#47132,
#47133,#47134,#47135,#47136,#47137,#47138,#47139,#47140,#47141,#47142,#47143,
#47144,#47145,#47146,#47147,#47148,#47149,#47150,#47151,#47152,#47153,#47154,
#47155,#47156,#47157,#47158,#47159,#47160,#47161,#47162,#47163,#47164,#47165,
#47166,#47167,#47168,#47169,#47170,#47171,#47172,#47173,#47174,#47175,#47176,
#47177,#47178,#47179,#47180,#47181,#47182,#47183,#47184,#47185,#47186,#47187,
#47188,#47189,#47190,#47191,#47192,#47193,#47194,#47195,#47196,#47197,#47198,
#47199,#47200,#47201,#47202,#47203,#47204,#47205,#47206,#47207,#47208,#47209,
#47210,#47211,#47212,#47213,#47214,#47215,#47216,#47217,#47218,#47219,#47220,
#47221,#47222,#47223,#47224,#47225,#47226,#47227,#47228,#47229,#47230,#47231,
#47232,#47233,#47234,#47235,#47236,#47237,#47238,#47239,#47240,#47241,#47242,
#47243,#47244,#47245,#47246,#47247,#47248,#47249,#47250,#47251,#47252,#47253,
#47254,#47255,#47256,#47257,#47258,#47259,#47260,#47261,#47262,#47263,#47264,
#47265,#47266,#47267,#47268,#47269,#47270,#47271,#47272,#47273,#47274,#47275,
#47276,#47277,#47278,#47279,#47280,#47281,#47282,#47283,#47284,#47285,#47286,
#47287,#47288,#47289,#47290,#47291,#47292,#47293,#47294,#47295),
 .UNSPECIFIED.,.F.,.F.,(4,3,3,3,3,3,3,3,3,3,3,3,3,3,3,3,3,3,3,3,3,3,3,3,
3,3,3,3,3,3,3,3,3,3,3,3,3,3,3,3,3,3,3,3,3,3,3,3,3,3,3,3,3,3,3,3,3,3,3,3,
3,3,3,3,3,3,3,3,3,3,3,3,3,3,3,3,3,3,3,3,3,3,3,3,3,4),(0.,1.47382713762708E-5,
8.1640167161615E-5,0.000113040897811508,0.000162304556226174,0.00016328033432323,
0.000211569726454149,0.00032656066864646,0.000605462375354082,0.000653121337292909,
0.000979682005939359,0.000998956362101892,0.00130624267458581,0.00139206000816881,
0.00158846721825144,0.00163280334323226,0.00168663405119503,0.00171444351039387,
0.00173570554393496,0.00178475826250593,0.00179608367755548,0.0019593640118787,
0.0021764066902377,0.00228592468052514,0.00256676504196455,0.00261248534917158,
0.00293904601781802,0.00295591148826027,0.00310232635214124,0.00315005096599843,
0.00318396651930285,0.00322478660288365,0.00324700883855564,0.00326560668646445,
0.00334387779966514,0.00359216735511088,0.00373044383356633,0.00391872802375731,
0.00411563875046019,0.00424528869240374,0.00449954862961719,0.00457184936105017,
0.00488223509352117,0.0048984100296966,0.00522497069834303,0.00526373999263159,
0.0053589350810355,0.00538825103266625,0.00545405001538152,0.00555153136698946,
0.00564409445256484,0.00587809203563587,0.00602336155693145,0.00604137236995909,
0.0061180115657291,0.00612301253712069,0.0062046527042823,0.00621259546927448,
0.00640159142864471,0.00653121337292871,0.0067789487108179,0.00685777404157513,
0.00715546455766113,0.00718433471022155,0.00751089537886797,0.00753114977976008,
0.00783745604751438,0.00790600171572738,0.0081640167161608,0.00828000681041783,
0.00846668442947774,0.00849057738480722,0.00855994046092843,0.00857221755196882,
0.00861303763554962,0.00865314855613666,0.00865385771913043,0.00881713805345364,
0.00914369872210006,0.0093982633178075,0.00947025939074649,0.00977046583129307,
0.00979682005939291,0.0101233807280393,0.0101424271025616,0.0104499413966858),
 .UNSPECIFIED.);
#934=B_SPLINE_CURVE_WITH_KNOTS('',3,(#47297,#47298,#47299,#47300,#47301,
#47302,#47303,#47304,#47305,#47306,#47307,#47308,#47309,#47310,#47311,#47312,
#47313,#47314,#47315,#47316,#47317,#47318,#47319,#47320,#47321,#47322,#47323,
#47324,#47325,#47326,#47327,#47328,#47329,#47330,#47331,#47332,#47333,#47334,
#47335,#47336,#47337,#47338,#47339,#47340,#47341,#47342,#47343,#47344,#47345,
#47346,#47347,#47348,#47349,#47350,#47351,#47352,#47353,#47354,#47355,#47356,
#47357,#47358,#47359,#47360,#47361,#47362,#47363,#47364,#47365,#47366,#47367,
#47368,#47369,#47370,#47371,#47372,#47373,#47374,#47375,#47376,#47377,#47378,
#47379,#47380,#47381,#47382,#47383,#47384,#47385,#47386,#47387,#47388,#47389,
#47390,#47391,#47392,#47393,#47394,#47395,#47396,#47397,#47398,#47399,#47400,
#47401,#47402,#47403,#47404,#47405,#47406,#47407,#47408,#47409,#47410,#47411,
#47412,#47413,#47414,#47415,#47416,#47417,#47418,#47419,#47420,#47421,#47422,
#47423,#47424,#47425,#47426,#47427,#47428,#47429,#47430,#47431,#47432,#47433,
#47434,#47435,#47436,#47437,#47438,#47439,#47440,#47441,#47442,#47443,#47444,
#47445,#47446,#47447,#47448,#47449,#47450,#47451,#47452,#47453,#47454,#47455,
#47456,#47457,#47458,#47459,#47460,#47461,#47462,#47463,#47464,#47465,#47466,
#47467,#47468,#47469,#47470,#47471,#47472,#47473,#47474,#47475,#47476,#47477,
#47478,#47479,#47480,#47481,#47482,#47483,#47484,#47485,#47486,#47487,#47488,
#47489,#47490,#47491,#47492,#47493,#47494,#47495,#47496,#47497,#47498,#47499,
#47500,#47501,#47502,#47503,#47504,#47505,#47506,#47507,#47508,#47509,#47510,
#47511,#47512,#47513,#47514,#47515,#47516,#47517,#47518,#47519,#47520,#47521,
#47522,#47523,#47524,#47525,#47526,#47527,#47528,#47529,#47530,#47531,#47532,
#47533,#47534,#47535,#47536,#47537,#47538,#47539,#47540,#47541,#47542,#47543,
#47544,#47545,#47546,#47547,#47548,#47549,#47550,#47551,#47552,#47553,#47554,
#47555,#47556,#47557,#47558,#47559,#47560,#47561,#47562,#47563,#47564,#47565,
#47566,#47567,#47568,#47569,#47570,#47571,#47572,#47573,#47574,#47575,#47576,
#47577,#47578,#47579,#47580,#47581,#47582,#47583,#47584,#47585,#47586,#47587,
#47588,#47589,#47590,#47591,#47592,#47593,#47594,#47595,#47596,#47597,#47598,
#47599,#47600,#47601,#47602,#47603,#47604,#47605,#47606,#47607,#47608,#47609,
#47610,#47611,#47612,#47613,#47614,#47615,#47616,#47617,#47618,#47619,#47620,
#47621,#47622,#47623,#47624,#47625,#47626,#47627,#47628,#47629,#47630,#47631,
#47632,#47633,#47634,#47635,#47636,#47637,#47638,#47639,#47640,#47641,#47642,
#47643,#47644,#47645,#47646,#47647,#47648,#47649,#47650,#47651,#47652,#47653,
#47654,#47655,#47656,#47657,#47658,#47659,#47660,#47661,#47662,#47663,#47664,
#47665,#47666,#47667,#47668,#47669,#47670,#47671,#47672,#47673,#47674,#47675,
#47676,#47677,#47678,#47679,#47680,#47681,#47682,#47683,#47684,#47685,#47686,
#47687,#47688,#47689,#47690,#47691,#47692,#47693,#47694,#47695,#47696,#47697,
#47698,#47699,#47700,#47701,#47702,#47703,#47704,#47705,#47706,#47707,#47708,
#47709,#47710,#47711,#47712,#47713,#47714,#47715,#47716,#47717,#47718,#47719,
#47720,#47721,#47722,#47723,#47724,#47725,#47726,#47727,#47728,#47729,#47730,
#47731,#47732,#47733,#47734,#47735,#47736,#47737,#47738,#47739,#47740,#47741,
#47742,#47743,#47744,#47745,#47746,#47747,#47748,#47749,#47750,#47751,#47752,
#47753,#47754,#47755,#47756,#47757,#47758,#47759,#47760,#47761,#47762,#47763,
#47764,#47765,#47766,#47767,#47768,#47769,#47770,#47771,#47772,#47773,#47774,
#47775,#47776,#47777,#47778,#47779,#47780,#47781,#47782,#47783,#47784,#47785,
#47786,#47787,#47788,#47789,#47790,#47791,#47792,#47793,#47794,#47795,#47796,
#47797,#47798,#47799,#47800,#47801,#47802,#47803,#47804,#47805,#47806,#47807,
#47808,#47809,#47810,#47811,#47812,#47813,#47814,#47815,#47816,#47817,#47818,
#47819,#47820,#47821,#47822,#47823,#47824,#47825,#47826,#47827,#47828,#47829,
#47830,#47831,#47832,#47833,#47834,#47835,#47836,#47837,#47838,#47839,#47840,
#47841,#47842,#47843,#47844,#47845,#47846,#47847,#47848,#47849,#47850,#47851,
#47852,#47853,#47854,#47855,#47856,#47857,#47858,#47859,#47860,#47861,#47862,
#47863,#47864,#47865,#47866,#47867,#47868,#47869,#47870,#47871,#47872,#47873,
#47874,#47875,#47876,#47877,#47878,#47879,#47880,#47881,#47882,#47883,#47884,
#47885,#47886,#47887,#47888,#47889,#47890,#47891,#47892,#47893,#47894,#47895,
#47896,#47897,#47898,#47899,#47900,#47901,#47902,#47903,#47904,#47905,#47906,
#47907,#47908,#47909,#47910,#47911,#47912,#47913,#47914,#47915,#47916,#47917,
#47918,#47919,#47920,#47921,#47922,#47923,#47924,#47925,#47926,#47927,#47928,
#47929,#47930,#47931,#47932,#47933,#47934,#47935,#47936,#47937,#47938,#47939,
#47940,#47941,#47942,#47943,#47944,#47945,#47946,#47947,#47948,#47949,#47950,
#47951,#47952,#47953,#47954,#47955,#47956,#47957,#47958,#47959,#47960,#47961,
#47962,#47963,#47964,#47965,#47966,#47967,#47968,#47969,#47970,#47971,#47972,
#47973,#47974,#47975,#47976,#47977,#47978,#47979,#47980,#47981,#47982,#47983,
#47984,#47985,#47986,#47987,#47988,#47989,#47990,#47991,#47992,#47993,#47994,
#47995,#47996,#47997,#47998,#47999,#48000,#48001,#48002,#48003,#48004,#48005,
#48006,#48007,#48008,#48009,#48010,#48011,#48012,#48013,#48014,#48015,#48016,
#48017,#48018,#48019,#48020,#48021,#48022,#48023,#48024,#48025,#48026,#48027,
#48028,#48029,#48030,#48031,#48032,#48033,#48034,#48035,#48036,#48037,#48038,
#48039,#48040,#48041,#48042,#48043,#48044,#48045,#48046,#48047,#48048,#48049,
#48050,#48051,#48052,#48053,#48054,#48055,#48056,#48057,#48058,#48059,#48060,
#48061,#48062,#48063,#48064,#48065,#48066,#48067,#48068,#48069,#48070,#48071,
#48072,#48073,#48074,#48075,#48076,#48077,#48078,#48079,#48080,#48081,#48082,
#48083,#48084,#48085,#48086,#48087,#48088,#48089,#48090,#48091,#48092,#48093,
#48094,#48095,#48096,#48097,#48098,#48099,#48100,#48101,#48102,#48103,#48104,
#48105,#48106,#48107,#48108,#48109,#48110,#48111,#48112,#48113,#48114,#48115,
#48116,#48117,#48118,#48119,#48120,#48121,#48122,#48123,#48124,#48125,#48126,
#48127,#48128,#48129,#48130,#48131,#48132,#48133,#48134,#48135,#48136,#48137,
#48138,#48139,#48140,#48141,#48142,#48143,#48144,#48145,#48146,#48147,#48148,
#48149,#48150,#48151,#48152,#48153,#48154,#48155,#48156,#48157,#48158,#48159,
#48160,#48161,#48162,#48163,#48164,#48165,#48166,#48167,#48168,#48169,#48170,
#48171,#48172,#48173,#48174,#48175,#48176,#48177,#48178,#48179,#48180,#48181,
#48182,#48183,#48184,#48185,#48186,#48187,#48188,#48189,#48190,#48191,#48192,
#48193,#48194),.UNSPECIFIED.,.F.,.F.,(4,3,3,3,3,3,3,3,3,3,3,3,3,3,3,3,3,
3,3,3,3,3,3,3,3,3,3,3,3,3,3,3,3,3,3,3,3,3,3,3,3,3,3,3,3,3,3,3,3,3,3,3,3,
3,3,3,3,3,3,3,3,3,3,3,3,3,3,3,3,3,3,3,3,3,3,3,3,3,3,3,3,3,3,3,3,3,3,3,3,
3,3,3,3,3,3,3,3,3,3,3,3,3,3,3,3,3,3,3,3,3,3,3,3,3,3,3,3,3,3,3,3,3,3,3,3,
3,3,3,3,3,3,3,3,3,3,3,3,3,3,3,3,3,3,3,3,3,3,3,3,3,3,3,3,3,3,3,3,3,3,3,3,
3,3,3,3,3,3,3,3,3,3,3,3,3,3,3,3,3,3,3,3,3,3,3,3,3,3,3,3,3,3,3,3,3,3,3,3,
3,3,3,3,3,3,3,3,3,3,3,3,3,3,3,3,3,3,3,3,3,3,3,3,3,3,3,3,3,3,3,3,3,3,3,3,
3,3,3,3,3,3,3,3,3,3,3,3,3,3,3,3,3,3,3,3,3,3,3,3,3,3,3,3,3,3,3,3,3,3,3,3,
3,3,3,3,3,3,3,3,3,3,3,3,3,3,3,3,3,3,3,3,3,3,3,3,3,3,3,3,3,3,4),(1.35130087435845E-15,
0.000427333961361783,0.000452399919294745,0.000904799838588138,0.00135719975788153,
0.00137425621759972,0.00180959967717493,0.00185103340846359,0.00203579963682163,
0.00209026025768216,0.00214889961664498,0.00221006611721062,0.00226199959646833,
0.00232994525493375,0.00271439951576174,0.00316679943505514,0.00329151263938818,
0.00361919935434855,0.00407159927364195,0.00425769262375026,0.00452399919293536,
0.004742581270083,0.00497639911222876,0.00522872838875649,0.00542879903152217,
0.00547229268389153,0.00559420535263831,0.00565499899116887,0.00571154898108054,
0.00571619320255349,0.00576809897099221,0.00588119895081556,0.00620467062394714,
0.006333598870109,0.00678599878940244,0.00718388137198869,0.00723839870869588,
0.00769079862798932,0.00814319854728276,0.00816621717001466,0.00841231680488797,
0.0085354464035452,0.0085955984665762,0.00865214845648787,0.00865861451015506,
0.00870869844639954,0.00882179842622286,0.00904799838586948,0.00915120921437489,
0.00950039830516272,0.00995279822445595,0.0101355902621457,0.0104051981437492,
0.0108575980630424,0.0111189149255724,0.0113099979823357,0.0113645824124405,
0.0114873943974255,0.0115361979419823,0.0115927479318939,0.011610181923162,
0.0116492979218056,0.0117623979016288,0.0121006755023117,0.012214797820922,
0.0126671977402151,0.0130783720079958,0.0131195976595082,0.0135719975788014,
0.0140243974980945,0.0140519386107737,0.0142505974577411,0.0142947100135889,
0.0143636974375644,0.0144159988972164,0.0144767974173877,0.014537210921105,
0.0149291973366808,0.015021231024896,0.015381597255974,0.0158339971752671,
0.0159855037164582,0.0162863970945603,0.0167387970138534,0.0169449728021871,
0.0171911969331465,0.0174173968927931,0.0174229451715688,0.0175304968726164,
0.017542255502331,0.0176435968524397,0.017661493031398,0.0178997543853799,
0.0180959967717328,0.0185483966910259,0.0188499922611146,0.019000796610319,
0.0194531965296122,0.0197958007633236,0.0199055964489053,0.0203579963681984,
0.0207371351958851,0.0208103962874915,0.0209234962673148,0.0209717468832201,
0.0210365962471381,0.0210889332304238,0.0212060192761904,0.0212627962067846,
0.0216733657645927,0.0217151961260777,0.0221675960453708,0.0226033011190297,
0.0226199959646638,0.0230723958839569,0.02352479580325,0.0235268185559895,
0.0236378957830733,0.0236944457729849,0.0237509957628965,0.0239771957225431,
0.0239870003329634,0.0242033956821896,0.0242182941868268,0.0243164956620129,
0.0243343114281531,0.0244295956418361,0.0244504496828121,0.0248819955611292,
0.0249151395533867,0.0253343954804223,0.0253800487757404,0.0257867953997154,
0.0258451744241752,0.0262391953190085,0.0263105151891527,0.0266915952383015,
0.0267760697666888,0.0270089229795263,0.0271253799242098,0.0271439951575946,
0.0272005451475063,0.0272418465555986,0.0272570951374179,0.0273701951172412,
0.0275963950768877,0.0277082392254462,0.0280487949961807,0.0281755795546116,
0.0285011949154738,0.0289535948347668,0.0291130107793379,0.0294059947540599,
0.029858394673353,0.0300540403436757,0.0302898597551073,0.030310794592646,
0.0304078553652295,0.0304238945724693,0.0305259116030602,0.0305369945522925,
0.030763194511939,0.0309988867607011,0.031215594431232,0.031667994350525,
0.0319483580710528,0.032120394269818,0.0325727941891111,0.032902491485125,
0.0330251941084041,0.0333813343952388,0.0334775940276971,0.0335906940075203,
0.0336212117526858,0.033647243997432,0.0337037939873436,0.0337412639505102,
0.0338613888123318,0.0339299939469901,0.0343823938662831,0.0348248994526247,
0.0348347937855762,0.0352871937048692,0.0357395936241622,0.035792980893805,
0.0361919935434553,0.0362788063756478,0.0366443934627483,0.0367658817816997,
0.0370967933820413,0.0372098933618646,0.0372542658321182,0.0373229933416879,
0.03749888830684,0.0375491933013344,0.0377436804253305,0.0380015932206275,
0.0384539931399206,0.0387245633800817,0.0389063930592137,0.0393587929785068,
0.0397082869870636,0.0398111928977999,0.0399546805469956,0.0400373928574464,
0.0400779528497158,0.0401504928372697,0.040201261975522,0.0402070428271813,
0.040263592817093,0.0406943510040045,0.0407159927363861,0.0411683926556793,
0.0416207925749724,0.0416794507159706,0.0420731924942656,0.0425255924135587,
0.0426631474812632,0.0429088555037357,0.0429779923328519,0.0430316764271511,
0.0430910923126752,0.0431544637395062,0.0432041922924984,0.0434303922521449,
0.043644905175834,0.043882792171438,0.0443351920907311,0.0446223981991244,
0.0447875920100241,0.0452399919293172,0.0455956456638855,0.0456923918486102,
0.0458054918284335,0.0458383181596209,0.0459185918082567,0.0459595566553906,
0.0460807118303458,0.0461447917679033,0.046564511684252,0.0465971916871963,
0.0470495916064894,0.0475019915257824,0.0475283529694127,0.0479543914450755,
0.0484067913643685,0.0484873842239486,0.0488591912836615,0.0489651292319899,
0.0489722912634848,0.0490843814225022,0.0490853912433081,0.0492035625454086,
0.0493115912029546,0.0494417143659409,0.0497639911222476,0.0502163910415407,
0.0503915617699481,0.0506687909608337,0.0511211908801268,0.0513370475099055,
0.0515735907994198,0.0520259907187128,0.0522781180849262,0.0524783906380059,
0.052512674995964,0.0525349406279175,0.0525914906178291,0.0526298364378429,
0.0527045905976524,0.0527469056214694,0.0529307905572989,0.0532142274876769,
0.0533831904765919,0.053835590395885,0.0541443207096413,0.054287990315178,
0.054740390234471,0.0550682858845152,0.0551927901537641,0.0552493401436757,
0.0553058901335873,0.0554189901134106,0.055528729013877,0.0556451900730571,
0.0557582900528804,0.0557601597824457,0.0558181936376942,0.0558713900327036,
0.0558762162462772,0.055992094547227,0.0560975899923501,0.0564548298442276,
0.0565499899116432,0.0569164222442635,0.0570023898309362,0.0573768793379545,
0.0574547897502292,0.057836211703915,0.0579071896695223),.UNSPECIFIED.);
#935=B_SPLINE_CURVE_WITH_KNOTS('',3,(#48196,#48197,#48198,#48199,#48200,
#48201,#48202,#48203,#48204,#48205,#48206,#48207,#48208,#48209,#48210,#48211,
#48212,#48213,#48214,#48215,#48216,#48217,#48218,#48219,#48220,#48221,#48222,
#48223,#48224,#48225,#48226,#48227),.UNSPECIFIED.,.F.,.F.,(4,1,1,1,2,2,
2,1,2,2,2,1,1,1,1,1,2,2,1,1,1,4),(0.00150858273324743,0.00182098751393329,
0.00213339229461915,0.00244579707530502,0.00275820185599088,0.00283630305116235,
0.00291440424633382,0.00307060663667675,0.00338301141736263,0.00353921380770556,
0.0036954161980485,0.00400782097873437,0.00432022575942025,0.00463263054010612,
0.00494503532079199,0.00525744010147787,0.00556984488216374,0.00564794607733521,
0.00572604727250669,0.00588224966284963,0.00619465444353553,0.00650705856419875),
 .UNSPECIFIED.);
#936=B_SPLINE_CURVE_WITH_KNOTS('',3,(#48231,#48232,#48233,#48234,#48235,
#48236,#48237,#48238,#48239,#48240,#48241,#48242,#48243,#48244,#48245,#48246,
#48247,#48248,#48249,#48250,#48251,#48252,#48253,#48254,#48255,#48256,#48257,
#48258,#48259,#48260,#48261,#48262,#48263,#48264,#48265,#48266,#48267,#48268,
#48269,#48270,#48271,#48272,#48273,#48274,#48275,#48276,#48277,#48278,#48279,
#48280,#48281,#48282,#48283,#48284,#48285,#48286,#48287,#48288,#48289,#48290,
#48291,#48292,#48293,#48294,#48295,#48296,#48297,#48298,#48299,#48300,#48301,
#48302,#48303,#48304,#48305,#48306,#48307,#48308,#48309,#48310,#48311,#48312,
#48313,#48314,#48315,#48316,#48317,#48318,#48319,#48320,#48321,#48322,#48323,
#48324,#48325,#48326,#48327,#48328,#48329,#48330,#48331,#48332,#48333,#48334,
#48335,#48336,#48337,#48338,#48339,#48340,#48341),.UNSPECIFIED.,.F.,.F.,
(4,2,2,2,1,1,1,1,2,1,2,2,1,1,1,1,1,2,2,1,1,1,1,2,2,2,1,1,1,2,2,2,1,1,1,
1,1,2,2,1,1,1,1,1,1,2,2,2,1,2,2,2,1,1,1,1,1,2,2,1,1,1,1,1,2,1,2,2,1,1,1,
1,2,2,1,1,1,1,1,4),(0.,0.000327684171192303,0.000409605213990379,0.000491526256788455,
0.000655368342384606,0.000983052513576909,0.00131073668476921,0.00163842085596152,
0.00196610502715382,0.00212994711274997,0.002170907634149,0.00221186815554804,
0.0022937891983461,0.0026214733695384,0.00294915754073069,0.00327684171192298,
0.00360452588311527,0.00393221005430756,0.00401413109710564,0.00409605213990371,
0.00425989422549987,0.00458757839669218,0.0049152625678845,0.00524294673907681,
0.00540678882467297,0.00557063091026913,0.00589831508146146,0.00622599925265378,
0.00655368342384611,0.00688136759503843,0.0070452096806346,0.00712713072343267,
0.00720905176623075,0.00753673593742304,0.00786442010861533,0.00819210427980761,
0.0085197884509999,0.00884747262219219,0.00892939366499025,0.00901131470778832,
0.00917515679338446,0.00950284096457672,0.00983052513576899,0.0101582093069613,
0.0104858934781535,0.0108135776493458,0.0108954986921438,0.0109774197349419,
0.011141261820538,0.0114689459917303,0.0116327880773264,0.0117147091201244,
0.0117966301629225,0.0121243143341147,0.012451998505307,0.0127796826764992,
0.0131073668476915,0.0134350510188837,0.0135169720616818,0.0135988931044798,
0.0137627351900759,0.0140904193612682,0.0144181035324604,0.0147457877036527,
0.0150734718748449,0.015237313960441,0.0153192350032391,0.0154011560460371,
0.0157288402172293,0.0160565243884215,0.0163842085596138,0.016711892730806,
0.0170395769019982,0.0170805374233972,0.0171214979447962,0.0172034189875943,
0.0173672610731904,0.0176949452443827,0.018022629415575,0.0180959256708578),
 .UNSPECIFIED.);
#937=B_SPLINE_CURVE_WITH_KNOTS('',3,(#48343,#48344,#48345,#48346,#48347,
#48348,#48349,#48350,#48351,#48352,#48353,#48354,#48355,#48356,#48357,#48358,
#48359,#48360,#48361,#48362,#48363,#48364,#48365),.UNSPECIFIED.,.F.,.F.,
(4,1,2,1,2,2,1,1,1,1,1,2,2,2,4),(0.0180959256708578,0.0183503135867672,
0.0186779977579595,0.0188418398435556,0.0188828003649547,0.0189237608863537,
0.0190056819291518,0.019333366100344,0.0196610502715362,0.0199887344427285,
0.0203164186139207,0.020644102785113,0.020726023827911,0.0208079448707091,
0.0209717869563052),.UNSPECIFIED.);
#938=B_SPLINE_CURVE_WITH_KNOTS('',3,(#48373,#48374,#48375,#48376,#48377,
#48378,#48379,#48380,#48381,#48382,#48383,#48384,#48385,#48386,#48387,#48388,
#48389,#48390,#48391,#48392,#48393,#48394,#48395,#48396),.UNSPECIFIED.,
 .F.,.F.,(4,2,2,2,1,1,1,1,1,2,2,2,1,2,4),(0.,0.000404302057260319,0.000606453085890479,
0.000656990843048018,0.000707528600205558,0.000808604114520648,0.00121290617178103,
0.00161720822904141,0.00202151028630179,0.00242581234356217,0.00247635010071971,
0.00252688785787726,0.00262796337219236,0.00283011440082255,0.00287050024670353),
 .UNSPECIFIED.);
#939=B_SPLINE_CURVE_WITH_KNOTS('',3,(#48402,#48403,#48404,#48405,#48406,
#48407,#48408,#48409,#48410,#48411,#48412,#48413,#48414,#48415,#48416,#48417,
#48418,#48419,#48420,#48421,#48422,#48423,#48424,#48425,#48426,#48427,#48428,
#48429,#48430,#48431,#48432,#48433,#48434,#48435,#48436,#48437,#48438,#48439,
#48440,#48441,#48442,#48443,#48444,#48445,#48446,#48447,#48448,#48449,#48450,
#48451,#48452,#48453,#48454,#48455,#48456,#48457,#48458,#48459,#48460,#48461,
#48462,#48463,#48464,#48465,#48466,#48467,#48468,#48469,#48470,#48471,#48472,
#48473,#48474,#48475,#48476,#48477,#48478,#48479,#48480,#48481,#48482,#48483,
#48484,#48485,#48486,#48487,#48488,#48489,#48490,#48491,#48492,#48493,#48494,
#48495,#48496,#48497,#48498,#48499,#48500,#48501,#48502,#48503,#48504,#48505,
#48506,#48507,#48508,#48509,#48510,#48511,#48512,#48513,#48514,#48515,#48516,
#48517,#48518,#48519,#48520,#48521,#48522,#48523,#48524,#48525,#48526,#48527,
#48528,#48529,#48530,#48531,#48532,#48533,#48534,#48535,#48536,#48537,#48538,
#48539,#48540,#48541,#48542,#48543,#48544,#48545,#48546,#48547,#48548,#48549,
#48550,#48551,#48552,#48553,#48554,#48555,#48556,#48557,#48558,#48559,#48560,
#48561,#48562,#48563,#48564),.UNSPECIFIED.,.F.,.F.,(4,3,3,3,3,3,3,3,3,3,
3,3,3,3,3,3,3,3,3,3,3,3,3,3,3,3,3,3,3,3,3,3,3,3,3,3,3,3,3,3,3,3,3,3,3,3,
3,3,3,3,3,3,3,3,4),(0.,3.18639464890314E-5,6.37278929780629E-5,6.41210145326926E-5,
0.000127455785956126,0.000128345084208553,0.000254911571912252,0.000256986082187868,
0.00031863946489032,0.000321403032292237,0.000350503411379359,0.000353635933676641,
0.000382367357868398,0.000385879972497687,0.000509823143824565,0.00051482305046768,
0.000637278929780732,0.00064371589233994,0.000675940606633055,0.000701006822758811,
0.000708139232281018,0.000764734715736889,0.000772510059645793,0.000892190501693046,
0.000900992059381932,0.0010196462876492,0.00102913438127321,0.00105151023413824,
0.00106111543219135,0.00108337418062729,0.00109306546511644,0.00114710207360537,
0.00115687341539025,0.00127455785956153,0.00128412906516313,0.0013382857525396,
0.0013475774277107,0.00137014969902864,0.00137925494612773,0.00138608167227316,
0.00140201364551768,0.00141090288465876,0.00152946943147388,0.00153723730022466,
0.00165692521743007,0.00166315794950942,0.00168878916391913,0.00169457239304465,
0.00172065311040818,0.001725963985598,0.00178438100338628,0.00178871072439317,
0.0019118367893425,0.00191408283353941,0.00203929257529871),
 .UNSPECIFIED.);
#940=B_SPLINE_CURVE_WITH_KNOTS('',3,(#48568,#48569,#48570,#48571,#48572,
#48573,#48574,#48575,#48576,#48577,#48578,#48579,#48580,#48581,#48582,#48583,
#48584,#48585,#48586,#48587,#48588,#48589,#48590,#48591,#48592,#48593,#48594,
#48595,#48596,#48597,#48598,#48599,#48600,#48601,#48602,#48603,#48604,#48605,
#48606,#48607,#48608,#48609,#48610,#48611,#48612,#48613,#48614,#48615,#48616,
#48617,#48618,#48619,#48620,#48621,#48622,#48623,#48624,#48625,#48626,#48627,
#48628,#48629,#48630,#48631,#48632,#48633,#48634,#48635,#48636,#48637,#48638,
#48639,#48640,#48641,#48642,#48643,#48644,#48645,#48646,#48647,#48648,#48649,
#48650,#48651,#48652,#48653,#48654,#48655,#48656,#48657,#48658,#48659,#48660,
#48661,#48662,#48663,#48664,#48665,#48666,#48667,#48668,#48669,#48670,#48671,
#48672,#48673,#48674,#48675,#48676,#48677,#48678,#48679,#48680,#48681,#48682,
#48683,#48684,#48685,#48686,#48687,#48688,#48689,#48690,#48691,#48692,#48693,
#48694,#48695,#48696,#48697,#48698,#48699,#48700,#48701,#48702,#48703,#48704,
#48705,#48706,#48707,#48708,#48709,#48710,#48711,#48712,#48713,#48714,#48715,
#48716,#48717,#48718,#48719,#48720,#48721,#48722,#48723,#48724,#48725,#48726,
#48727,#48728,#48729,#48730,#48731,#48732,#48733,#48734,#48735,#48736,#48737,
#48738,#48739,#48740,#48741,#48742,#48743,#48744,#48745,#48746,#48747,#48748,
#48749,#48750,#48751,#48752,#48753,#48754,#48755,#48756,#48757,#48758,#48759,
#48760,#48761,#48762,#48763,#48764,#48765,#48766,#48767,#48768,#48769,#48770,
#48771,#48772,#48773,#48774,#48775,#48776,#48777,#48778,#48779,#48780,#48781,
#48782,#48783,#48784,#48785,#48786,#48787,#48788,#48789,#48790,#48791,#48792,
#48793,#48794,#48795,#48796,#48797,#48798,#48799,#48800,#48801,#48802,#48803,
#48804,#48805,#48806,#48807,#48808,#48809,#48810,#48811,#48812,#48813,#48814,
#48815,#48816,#48817,#48818,#48819,#48820,#48821,#48822,#48823,#48824,#48825,
#48826,#48827,#48828,#48829,#48830,#48831,#48832,#48833,#48834,#48835,#48836,
#48837,#48838,#48839,#48840,#48841,#48842,#48843,#48844,#48845,#48846,#48847,
#48848,#48849,#48850,#48851,#48852,#48853,#48854,#48855,#48856,#48857,#48858,
#48859,#48860,#48861,#48862,#48863,#48864,#48865,#48866,#48867,#48868,#48869,
#48870,#48871,#48872,#48873,#48874,#48875,#48876,#48877,#48878,#48879,#48880,
#48881,#48882,#48883,#48884,#48885,#48886,#48887,#48888,#48889,#48890,#48891,
#48892,#48893,#48894,#48895,#48896,#48897,#48898,#48899,#48900,#48901,#48902,
#48903,#48904),.UNSPECIFIED.,.F.,.F.,(4,3,3,3,3,3,3,3,3,3,3,3,3,3,3,3,3,
3,3,3,3,3,3,3,3,3,3,3,3,3,3,3,3,3,3,3,3,3,3,3,3,3,3,3,3,3,3,3,3,3,3,3,3,
3,3,3,3,3,3,3,3,3,3,3,3,3,3,3,3,3,3,3,3,3,3,3,3,3,3,3,3,3,3,3,3,3,3,3,3,
3,3,3,3,3,3,3,3,3,3,3,3,3,3,3,3,3,3,3,3,3,3,3,4),(0.000508896922368124,
0.00062679268456143,0.000694215802633637,0.000722273925456762,0.000770115844337078,
0.000786875242766394,0.000817979061112908,0.00087953468289915,0.00119981935441286,
0.00125017244343018,0.00157976306645661,0.0016208102039612,0.00195781302661255,
0.00199144796449223,0.00200493413523007,0.00203777768455861,0.00205203895394171,
0.00208410740462498,0.00214614867439737,0.00217676684475773,0.00233394447481585,
0.00236208572502323,0.00270788036409555,0.00273272348555424,0.00307964429810653,
0.00310336124608524,0.00326471182245848,0.00328868012635075,0.00331089450480051,
0.00333500984641712,0.00335704244288744,0.00338133956648349,0.00344925827006305,
0.00347399900661624,0.00381721458198522,0.00384463676714722,0.00418375979341684,
0.0042152745276782,0.00454893518005286,0.00458591228820918,0.00473101305800698,
0.00477123116847467,0.00477647916606545,0.00481756088854104,0.00482192941622211,
0.00486389060860741,0.0049128277143484,0.00495655004874015,0.00527642614332629,
0.00532718780927112,0.00564003173827683,0.00569782556980208,0.00600364422750113,
0.00606846333033304,0.00618545305026818,0.00625378221059853,0.0062763590005516,
0.00632181397973453,0.00634644165073127,0.00636726387109635,0.00643910109086401,
0.00673150520028908,0.00680973885139497,0.00709682934653332,0.00718037661192593,
0.00746321783764368,0.0075510143724569,0.00773633325272238,0.00782899269285512,
0.00783068046334138,0.00787532241292148,0.00792165213298785,0.00792272840334262,
0.00801488016841674,0.00819949185806941,0.00829228989351877,0.00856996656715454,
0.00866292765404969,0.00894215245343001,0.00903356541458061,0.00912622485471334,
0.00912891711519763,0.0091725545747797,0.00921888429484607,0.00922247490999389,
0.00931615226136386,0.00940420317511152,0.00969206179812406,0.00977484093564244,
0.0100699886879928,0.0101454786961734,0.0101648047219716,0.0102122670821918,
0.0102381381363061,0.0102597607703787,0.0102844678563724,0.0103307975764388,
0.0104499952267052,0.0105161164567042,0.0108316606729338,0.0108867542172351,
0.0112149921303994,0.011257391977766,0.0112630319454068,0.0113110990680315,
0.0113500514178987,0.0114072584462233,0.0114427108580314,0.0115996012232503,
0.0116280297382968,0.0119843864839696,0.0119986674988277,0.0123693052593585),
 .UNSPECIFIED.);
#941=B_SPLINE_CURVE_WITH_KNOTS('',3,(#48913,#48914,#48915,#48916,#48917,
#48918,#48919,#48920,#48921,#48922,#48923,#48924,#48925,#48926,#48927,#48928,
#48929,#48930,#48931,#48932,#48933,#48934,#48935,#48936,#48937,#48938,#48939,
#48940,#48941,#48942,#48943,#48944,#48945,#48946,#48947,#48948,#48949,#48950,
#48951,#48952,#48953,#48954,#48955,#48956,#48957,#48958,#48959,#48960,#48961,
#48962,#48963,#48964,#48965,#48966,#48967,#48968,#48969,#48970,#48971,#48972,
#48973,#48974,#48975,#48976,#48977,#48978,#48979,#48980,#48981,#48982,#48983,
#48984,#48985,#48986,#48987,#48988,#48989,#48990,#48991,#48992,#48993,#48994,
#48995,#48996,#48997,#48998,#48999,#49000,#49001,#49002,#49003,#49004,#49005,
#49006,#49007,#49008,#49009,#49010,#49011,#49012,#49013,#49014,#49015,#49016,
#49017,#49018,#49019,#49020,#49021,#49022,#49023,#49024,#49025,#49026,#49027,
#49028,#49029,#49030,#49031,#49032,#49033,#49034,#49035,#49036,#49037,#49038,
#49039,#49040,#49041,#49042),.UNSPECIFIED.,.F.,.F.,(4,3,3,3,3,3,3,3,3,3,
3,3,3,3,3,3,3,3,3,3,3,3,3,3,3,3,3,3,3,3,3,3,3,3,3,3,3,3,3,3,3,3,3,4),(0.,
0.000143006486471262,0.000286213476805868,0.000357892947021547,0.00036795089748439,
0.00039375248651578,0.00040474598723283,0.000429627568206775,0.00044154107698127,
0.000573487553939991,0.00058872143597501,0.000717955417591896,0.00073590179496875,
0.000863039500904423,0.000883082153962491,0.000899407029589682,0.000919877243710927,
0.000935823910690361,0.000956672333459362,0.00100881580072779,0.00103026251295622,
0.00115543610824654,0.00117744287194994,0.0013029129807526,0.00132462323094365,
0.00136141832069209,0.00137697769414036,0.00139821341044052,0.00141409436919456,
0.00145125851741666,0.00147180358993741,0.00160037565935921,0.00161898394893119,
0.00175023704203193,0.00176616430792498,0.00182545039553862,0.00183975448742187,
0.00186312708189405,0.0018765495771703,0.00190084390658505,0.00191334466691873,
0.00205189593230952,0.00220324218187337,0.00235488574389977),
 .UNSPECIFIED.);
#942=B_SPLINE_CURVE_WITH_KNOTS('',3,(#49048,#49049,#49050,#49051,#49052,
#49053,#49054,#49055,#49056,#49057,#49058,#49059,#49060,#49061,#49062,#49063,
#49064,#49065,#49066,#49067,#49068,#49069,#49070,#49071,#49072,#49073,#49074,
#49075,#49076,#49077,#49078,#49079,#49080,#49081,#49082,#49083,#49084,#49085,
#49086,#49087,#49088,#49089,#49090,#49091,#49092,#49093,#49094,#49095,#49096,
#49097,#49098,#49099,#49100,#49101,#49102,#49103,#49104,#49105,#49106,#49107,
#49108,#49109,#49110,#49111,#49112,#49113,#49114,#49115,#49116,#49117,#49118,
#49119,#49120,#49121,#49122,#49123,#49124,#49125,#49126,#49127,#49128,#49129,
#49130,#49131,#49132,#49133,#49134,#49135,#49136,#49137,#49138,#49139,#49140,
#49141,#49142,#49143,#49144,#49145,#49146,#49147,#49148,#49149,#49150,#49151,
#49152,#49153,#49154,#49155,#49156,#49157,#49158,#49159,#49160,#49161,#49162,
#49163,#49164,#49165,#49166,#49167,#49168,#49169,#49170,#49171,#49172,#49173,
#49174,#49175,#49176,#49177,#49178,#49179,#49180,#49181,#49182,#49183,#49184,
#49185,#49186,#49187,#49188,#49189,#49190,#49191,#49192,#49193,#49194,#49195,
#49196,#49197,#49198,#49199,#49200,#49201,#49202,#49203,#49204,#49205,#49206,
#49207,#49208,#49209,#49210,#49211,#49212,#49213,#49214,#49215,#49216,#49217,
#49218,#49219,#49220,#49221,#49222,#49223,#49224,#49225,#49226,#49227,#49228,
#49229,#49230,#49231,#49232,#49233,#49234,#49235,#49236,#49237,#49238,#49239,
#49240,#49241,#49242,#49243,#49244,#49245,#49246,#49247,#49248,#49249,#49250,
#49251,#49252,#49253,#49254,#49255,#49256,#49257,#49258,#49259,#49260,#49261,
#49262,#49263,#49264,#49265,#49266,#49267,#49268,#49269,#49270,#49271,#49272,
#49273,#49274,#49275,#49276,#49277,#49278,#49279,#49280,#49281,#49282,#49283,
#49284,#49285,#49286,#49287,#49288,#49289,#49290,#49291,#49292,#49293,#49294,
#49295,#49296,#49297,#49298,#49299,#49300,#49301,#49302,#49303,#49304,#49305,
#49306,#49307,#49308,#49309,#49310,#49311,#49312,#49313,#49314,#49315,#49316,
#49317,#49318,#49319,#49320,#49321,#49322,#49323,#49324,#49325,#49326,#49327,
#49328,#49329,#49330,#49331,#49332,#49333,#49334,#49335,#49336,#49337,#49338,
#49339,#49340,#49341,#49342,#49343,#49344,#49345,#49346,#49347,#49348,#49349,
#49350,#49351,#49352,#49353,#49354,#49355,#49356,#49357,#49358,#49359,#49360,
#49361,#49362,#49363,#49364,#49365,#49366,#49367,#49368,#49369,#49370,#49371,
#49372,#49373,#49374,#49375,#49376,#49377,#49378,#49379,#49380,#49381,#49382,
#49383,#49384,#49385,#49386,#49387,#49388,#49389,#49390,#49391,#49392,#49393,
#49394,#49395,#49396,#49397,#49398,#49399,#49400,#49401,#49402,#49403,#49404,
#49405,#49406,#49407,#49408,#49409,#49410,#49411,#49412,#49413,#49414,#49415,
#49416,#49417,#49418,#49419,#49420,#49421,#49422,#49423,#49424,#49425,#49426,
#49427,#49428,#49429,#49430,#49431,#49432,#49433,#49434,#49435,#49436,#49437,
#49438,#49439,#49440,#49441,#49442,#49443,#49444,#49445,#49446,#49447,#49448,
#49449,#49450,#49451,#49452,#49453,#49454,#49455,#49456,#49457,#49458,#49459,
#49460,#49461,#49462,#49463,#49464,#49465,#49466,#49467,#49468),
 .UNSPECIFIED.,.F.,.F.,(4,3,3,3,3,3,3,3,3,3,3,3,3,3,3,3,3,3,3,3,3,3,3,3,
3,3,3,3,3,3,3,3,3,3,3,3,3,3,3,3,3,3,3,3,3,3,3,3,3,3,3,3,3,3,3,3,3,3,3,3,
3,3,3,3,3,3,3,3,3,3,3,3,3,3,3,3,3,3,3,3,3,3,3,3,3,3,3,3,3,3,3,3,3,3,3,3,
3,3,3,3,3,3,3,3,3,3,3,3,3,3,3,3,3,3,3,3,3,3,3,3,3,3,3,3,3,3,3,3,3,3,3,3,
3,3,3,3,3,3,3,3,4),(0.0206553117127684,0.0206652454314341,0.020977754093757,
0.0209932652001871,0.0210342676712812,0.0210584056073977,0.0210752701423753,
0.0211390602079718,0.0211572750845636,0.0213003887218439,0.0213212849689401,
0.0216231006468298,0.021649304737693,0.0219458804428054,0.021977324506446,
0.0222687230927608,0.022305344275199,0.0223873492173872,0.0224693541595754,
0.0225513591017637,0.0225921303763807,0.0226333640439519,0.0226734259721932,
0.0227547651406014,0.0229175515000403,0.0229613838127049,0.0232435588607619,
0.0232894035814578,0.0235700957719074,0.0236174233502108,0.0238971166937416,
0.0239454431189638,0.0242734628877167,0.024552476688935,0.0246014826564697,
0.0246834875986579,0.0247165657485061,0.0247654925408462,0.0248807370535453,
0.0249295024252226,0.0252092956009399,0.0252575221939756,0.0255855419627286,
0.0258672170688867,0.0262415815002346,0.0265261212738976,0.0268976210377406,
0.0271859382610359,0.0275536605752466,0.0278466298598623,0.0278816803439996,
0.0279800382563648,0.0280119405217654,0.028045690228376,0.0281772804766694,
0.0282097001127526,0.0285080316106845,0.0288657396502586,0.0291697976252322,
0.0295217791877647,0.0298319150904524,0.0301778187252707,0.0304943913353953,
0.0308338582627768,0.0311572425264474,0.0314888172862714,0.0314898978002828,
0.0315719027424711,0.0316539076846594,0.031654635200809,0.0318179175690359,
0.031820437092583,0.032145937337789,0.0324834414874758,0.0328019768752952,
0.0331461052792798,0.0334580164128014,0.0337860361815545,0.0338084021110293,
0.0341140559503076,0.0341394015335586,0.0342780658346841,0.03430486008473,
0.0343600707768724,0.0343875772698666,0.0344420757190606,0.0344702734924882,
0.0347700954878137,0.0351310507499728,0.0354261350253198,0.0357541547940729,
0.0357903626390529,0.036082174562826,0.036410194331579,0.0364480861093856,
0.0364921992737673,0.0365301816915314,0.0365742042159556,0.0366122412866671,
0.0367382141003321,0.0367762502272079,0.0370662338690852,0.0371038366868402,
0.0373942536378383,0.0377222734065914,0.0377572542435978,0.0380502931753445,
0.0380830589309606,0.0382143030597211,0.0382457257725544,0.0382553055308152,
0.0382963080019093,0.0383783129440976,0.0384082492712995,0.0387063327128507,
0.0390343524816037,0.0390570819824594,0.0393623722503567,0.0393807475270067,
0.0396903920191098,0.0397039097155817,0.0398544019034863,0.0398652996031417,
0.0399459546746198,0.0400184117878628,0.0400265578380655,0.0403464315566159,
0.0403488907999544,0.0406710878644882,0.0406744513253689,0.0409931525516835,
0.041002471094122,0.0413150852190492,0.041330490862875,0.0414760016616697,
0.0414945007472516,0.0415564472644614,0.0415765056894398,0.0415966652495433,
0.041617508160534,0.0416368845266418),.UNSPECIFIED.);
#943=B_SPLINE_CURVE_WITH_KNOTS('',3,(#49471,#49472,#49473,#49474,#49475,
#49476,#49477,#49478,#49479,#49480,#49481,#49482,#49483,#49484,#49485,#49486,
#49487,#49488,#49489,#49490,#49491,#49492,#49493,#49494,#49495,#49496,#49497,
#49498,#49499,#49500,#49501,#49502,#49503,#49504,#49505,#49506,#49507,#49508,
#49509,#49510,#49511,#49512,#49513,#49514,#49515,#49516,#49517,#49518,#49519,
#49520,#49521,#49522,#49523,#49524,#49525,#49526,#49527,#49528,#49529,#49530,
#49531,#49532,#49533,#49534,#49535,#49536,#49537,#49538,#49539,#49540,#49541,
#49542,#49543,#49544,#49545,#49546,#49547,#49548,#49549,#49550,#49551,#49552,
#49553,#49554,#49555,#49556,#49557,#49558,#49559,#49560,#49561,#49562,#49563,
#49564,#49565,#49566,#49567,#49568,#49569,#49570,#49571,#49572,#49573,#49574,
#49575,#49576,#49577,#49578,#49579,#49580,#49581,#49582,#49583,#49584,#49585,
#49586,#49587,#49588,#49589,#49590,#49591,#49592,#49593,#49594,#49595,#49596,
#49597,#49598,#49599,#49600,#49601,#49602,#49603,#49604,#49605,#49606,#49607,
#49608,#49609,#49610,#49611,#49612,#49613,#49614,#49615,#49616,#49617,#49618,
#49619,#49620,#49621,#49622,#49623,#49624,#49625,#49626,#49627,#49628,#49629,
#49630,#49631,#49632,#49633,#49634,#49635,#49636,#49637,#49638,#49639,#49640,
#49641,#49642,#49643,#49644,#49645,#49646,#49647,#49648,#49649,#49650,#49651,
#49652,#49653,#49654,#49655,#49656,#49657,#49658,#49659,#49660,#49661,#49662,
#49663,#49664,#49665,#49666,#49667,#49668,#49669,#49670,#49671,#49672,#49673,
#49674,#49675,#49676,#49677,#49678,#49679,#49680,#49681,#49682,#49683,#49684,
#49685,#49686,#49687,#49688,#49689,#49690,#49691,#49692,#49693,#49694,#49695,
#49696,#49697,#49698,#49699,#49700,#49701,#49702,#49703,#49704,#49705,#49706,
#49707,#49708,#49709,#49710,#49711,#49712,#49713,#49714,#49715,#49716,#49717,
#49718,#49719,#49720,#49721,#49722,#49723,#49724,#49725,#49726,#49727,#49728,
#49729,#49730,#49731,#49732,#49733,#49734,#49735,#49736,#49737,#49738,#49739,
#49740,#49741,#49742,#49743,#49744,#49745,#49746,#49747,#49748,#49749,#49750,
#49751,#49752,#49753,#49754,#49755,#49756,#49757,#49758,#49759,#49760,#49761,
#49762,#49763,#49764,#49765,#49766,#49767,#49768,#49769,#49770,#49771,#49772,
#49773,#49774,#49775,#49776,#49777,#49778,#49779,#49780,#49781,#49782,#49783,
#49784,#49785,#49786,#49787,#49788,#49789,#49790,#49791,#49792,#49793,#49794,
#49795,#49796,#49797,#49798,#49799,#49800,#49801,#49802,#49803,#49804,#49805,
#49806,#49807,#49808,#49809,#49810,#49811,#49812,#49813,#49814,#49815,#49816,
#49817,#49818,#49819,#49820,#49821,#49822,#49823,#49824,#49825,#49826,#49827,
#49828,#49829,#49830,#49831,#49832,#49833,#49834,#49835,#49836,#49837,#49838,
#49839,#49840,#49841,#49842,#49843,#49844,#49845,#49846,#49847,#49848,#49849,
#49850,#49851,#49852,#49853,#49854,#49855,#49856,#49857,#49858,#49859,#49860,
#49861),.UNSPECIFIED.,.F.,.F.,(4,3,3,3,3,3,3,3,3,3,3,3,3,3,3,3,3,3,3,3,
3,3,3,3,3,3,3,3,3,3,3,3,3,3,3,3,3,3,3,3,3,3,3,3,3,3,3,3,3,3,3,3,3,3,3,3,
3,3,3,3,3,3,3,3,3,3,3,3,3,3,3,3,3,3,3,3,3,3,3,3,3,3,3,3,3,3,3,3,3,3,3,3,
3,3,3,3,3,3,3,3,3,3,3,3,3,3,3,3,3,3,3,3,3,3,3,3,3,3,3,3,3,3,3,3,3,3,3,3,
3,3,4),(0.041957164410437,0.0419580282593461,0.0419865304003811,0.0422778480319385,
0.0423145501691341,0.042598747472383,0.042642569937887,0.0429207530509651,
0.04297058970664,0.0430821721477515,0.0431345995910165,0.0431629890966594,
0.0432166045332047,0.0432438666760118,0.0432986094753929,0.0435677751170178,
0.0436266292441459,0.0439546490128989,0.0442172193461882,0.0442826687816519,
0.0445427409092368,0.0446106885504049,0.0447057005683472,0.0447746984347814,
0.0447872307357854,0.0448400446384891,0.0448567033769696,0.0448687931306013,
0.0449387083191578,0.0452667280879107,0.0455225904419517,0.0455947478566636,
0.0459227676254165,0.046178592821652,0.0462507873941694,0.0465074031590051,
0.0465788071629223,0.0465896703494642,0.0466719689207823,0.0468366677402474,
0.0469068269316752,0.0472348467004281,0.0474963684871569,0.0478908862379339,
0.0481574787691429,0.0482189060066868,0.0483829158910632,0.0484649208332514,
0.048488535463458,0.0485469257754396,0.0485713483333225,0.0486541709718429,
0.0488198358119608,0.0488749455441925,0.0492029653129454,0.0494827516683778,
0.0498590048504511,0.0501460513738034,0.0505150443879569,0.0508097071743785,
0.0511710839254627,0.0514736994554526,0.0514991036942155,0.0515811086364038,
0.0516397419533068,0.051663113578592,0.0518057633287904,0.0518271234629685,
0.0521377210298803,0.0524831630004743,0.0528013150691172,0.0531392025379801,
0.0534644977760899,0.053795242075486,0.0541272802645444,0.0544512816129918,
0.0547896633480624,0.0551073211504977,0.0554353409192506,0.0554516373676069,
0.0555173458614388,0.0555343525719785,0.0555993508036271,0.0556170522770077,
0.0557633606880035,0.0557824062888781,0.0561129301282526,0.0564194002255094,
0.0567732198580588,0.0570754397630152,0.0574034595317682,0.0574324401050507,
0.0577314793005211,0.058059499069274,0.0580904787336963,0.0582235089536505,
0.0582547858893481,0.0583055138958387,0.058375815716685,0.0584189997464737,
0.0587155386067799,0.0587471023565642,0.0590435583755328,0.0590747344055545,
0.0593715781442858,0.0594018599075076,0.0596995979130387,0.0597284330635356,
0.0598636077974152,0.0598914947728063,0.0599456127396034,0.059972965839742,
0.0599866152106975,0.0600276176817916,0.0600543950381653,0.0603556374505446,
0.0603797504464674,0.0606836572192975,0.0607044891413336,0.0610116769880505,
0.061028559959805,0.0611756868724269,0.0611903246948573,0.0612576918146152,
0.0612711334768389,0.0612986942857093,0.0613396967568034,0.0613519093639181,
0.0616677165255564,0.0616748080368333,0.0619121248264431),.UNSPECIFIED.);
#944=B_SPLINE_CURVE_WITH_KNOTS('',3,(#49864,#49865,#49866,#49867,#49868,
#49869,#49870,#49871,#49872,#49873,#49874,#49875,#49876,#49877,#49878,#49879,
#49880,#49881,#49882,#49883,#49884,#49885,#49886,#49887,#49888,#49889,#49890,
#49891,#49892,#49893,#49894,#49895,#49896,#49897,#49898,#49899,#49900,#49901,
#49902,#49903,#49904,#49905,#49906,#49907,#49908,#49909,#49910,#49911,#49912,
#49913,#49914,#49915,#49916,#49917,#49918,#49919,#49920,#49921,#49922,#49923,
#49924,#49925,#49926,#49927,#49928,#49929,#49930,#49931,#49932,#49933,#49934,
#49935,#49936,#49937,#49938,#49939,#49940,#49941,#49942,#49943,#49944,#49945,
#49946,#49947,#49948,#49949,#49950,#49951,#49952,#49953,#49954,#49955,#49956,
#49957,#49958,#49959,#49960,#49961,#49962,#49963,#49964,#49965,#49966,#49967,
#49968,#49969,#49970,#49971,#49972,#49973,#49974,#49975,#49976,#49977,#49978,
#49979,#49980,#49981),.UNSPECIFIED.,.F.,.F.,(4,2,1,1,1,1,1,2,2,1,1,1,2,
2,2,1,1,1,1,1,2,2,2,1,1,1,1,1,1,1,2,1,1,1,1,1,1,1,1,1,2,2,1,1,1,1,1,1,1,
1,2,2,1,1,1,1,1,1,2,2,1,1,1,1,1,1,2,2,2,1,1,1,1,1,2,2,1,1,1,1,1,1,2,1,2,
2,1,1,1,1,1,4),(0.0551992890963671,0.0552052082809216,0.0553145255250422,
0.0555331600132834,0.0557517945015246,0.0558611117456452,0.0559157703677055,
0.0559635966620083,0.0559704289897659,0.0564076979662487,0.0568449669427315,
0.0572822359192143,0.0577195048956971,0.0579381393839385,0.0580474566280592,
0.0581567738721799,0.0585940428486627,0.0590313118251455,0.0594685808016283,
0.0599058497781111,0.0603431187545939,0.0605617532428353,0.0606164118648956,
0.0606710704869559,0.0607803877310766,0.0612176567075593,0.061654925684042,
0.0620921946605247,0.0625294636370074,0.0629667326134901,0.0634040015899728,
0.0634586602120332,0.0635133188340935,0.0636226360782142,0.0638412705664556,
0.0642785395429383,0.0647158085194211,0.0651530774959038,0.0655903464723866,
0.0660276154488694,0.0664648844253521,0.0665195430474125,0.0665742016694728,
0.0666835189135935,0.0669021534018348,0.0673394223783175,0.0677766913548003,
0.068213960331283,0.0686512293077657,0.0690884982842484,0.0695257672607311,
0.0696350845048518,0.0697444017489724,0.0699630362372138,0.0704003052136965,
0.0708375741901792,0.0712748431666619,0.0717121121431446,0.0721493811196273,
0.0722040397416877,0.072258698363748,0.0723680156078687,0.07258665009611,
0.0730239190725927,0.0734611880490754,0.0738984570255581,0.0743357260020407,
0.0745543604902821,0.0747729949785234,0.0752102639550061,0.0756475329314888,
0.0760848019079715,0.0765220708844541,0.0769593398609368,0.0773966088374195,
0.0776152433256608,0.0778338778139022,0.0782711467903849,0.0787084157668675,
0.0791456847433502,0.0795829537198329,0.0800202226963156,0.0804574916727983,
0.0806761261610396,0.0807854434051603,0.0808947606492809,0.0813320296257635,
0.0817692986022461,0.0822065675787287,0.0826438365552113,0.0830811055316939,
0.0831743481010765),.UNSPECIFIED.);
#945=B_SPLINE_CURVE_WITH_KNOTS('',3,(#49982,#49983,#49984,#49985,#49986,
#49987,#49988,#49989,#49990,#49991,#49992,#49993,#49994,#49995,#49996,#49997,
#49998,#49999,#50000,#50001,#50002,#50003,#50004,#50005,#50006,#50007,#50008,
#50009,#50010,#50011,#50012,#50013,#50014,#50015,#50016,#50017,#50018,#50019,
#50020,#50021,#50022,#50023,#50024,#50025,#50026,#50027,#50028,#50029,#50030,
#50031,#50032,#50033,#50034,#50035,#50036,#50037,#50038,#50039,#50040,#50041,
#50042,#50043,#50044,#50045,#50046,#50047,#50048,#50049,#50050,#50051,#50052,
#50053,#50054,#50055,#50056,#50057,#50058,#50059,#50060,#50061,#50062,#50063,
#50064,#50065,#50066,#50067,#50068,#50069,#50070,#50071,#50072,#50073,#50074,
#50075,#50076,#50077,#50078,#50079,#50080,#50081,#50082,#50083,#50084,#50085,
#50086,#50087,#50088,#50089,#50090,#50091,#50092,#50093,#50094,#50095,#50096,
#50097,#50098,#50099,#50100,#50101,#50102,#50103,#50104,#50105,#50106),
 .UNSPECIFIED.,.F.,.F.,(4,2,1,1,2,2,1,2,2,2,1,1,1,1,1,2,1,1,2,2,1,1,1,1,
1,2,1,2,2,1,1,1,1,1,1,2,1,2,2,1,1,1,1,1,1,2,1,2,2,1,1,1,1,1,2,2,2,1,1,1,
1,1,2,2,2,1,1,1,1,2,1,2,2,1,1,1,1,1,1,2,1,1,2,2,1,1,1,1,1,1,2,4),(0.0272039191113106,
0.0275479455184106,0.0277665800066519,0.0278758972507726,0.0279305558728329,
0.0279852144948932,0.0284224834713757,0.0288597524478581,0.0289690696919787,
0.0290783869360993,0.0292970214243406,0.029734290400823,0.0301715593773054,
0.0306088283537878,0.0310460973302702,0.0314833663067526,0.0317020007949938,
0.0318113180391144,0.0318659766611747,0.031920635283235,0.0323579042597174,
0.0327951732361998,0.0332324422126821,0.0336697111891645,0.0341069801656468,
0.0345442491421292,0.0346535663862498,0.0347082250083101,0.0347628836303704,
0.0349815181186115,0.0354187870950939,0.0358560560715762,0.0362933250480586,
0.0367305940245409,0.0371678630010232,0.0376051319775056,0.0377144492216262,
0.0377691078436864,0.0378237664657467,0.0380424009539879,0.0384796699304703,
0.0389169389069527,0.039354207883435,0.0397914768599174,0.0402287458363998,
0.0406660148128821,0.0407753320570027,0.040829990679063,0.0408846493011233,
0.0411032837893645,0.0415405527658469,0.0419778217423292,0.0424150907188116,
0.042852359695294,0.0432896286717764,0.0435082631600175,0.0436175804041381,
0.0437268976482587,0.0441641666247411,0.0446014356012235,0.0450387045777058,
0.0454759735541882,0.0459132425306706,0.0461318770189118,0.0463505115071529,
0.0467877804836353,0.0472250494601177,0.0476623184366001,0.0480995874130824,
0.0485368563895648,0.048755490877806,0.0488648081219266,0.0489194667439869,
0.0489741253660472,0.0494113943425296,0.049848663319012,0.0502859322954944,
0.0507232012719768,0.0511604702484592,0.0515977392249416,0.0518163737131828,
0.0519256909573034,0.0519803495793637,0.0520350082014241,0.0524722771779065,
0.0529095461543889,0.0533468151308713,0.0537840841073537,0.0542213530838361,
0.0546586220603186,0.055095891036801,0.0551992890963671),.UNSPECIFIED.);
#946=B_SPLINE_CURVE_WITH_KNOTS('',3,(#50114,#50115,#50116,#50117,#50118,
#50119),.UNSPECIFIED.,.F.,.F.,(4,1,1,4),(0.00380072940365624,0.00412124310825456,
0.00444175681285289,0.00448635962221661),.UNSPECIFIED.);
#947=B_SPLINE_CURVE_WITH_KNOTS('',3,(#50121,#50122,#50123,#50124,#50125,
#50126,#50127,#50128,#50129,#50130,#50131,#50132,#50133,#50134,#50135,#50136,
#50137,#50138,#50139,#50140,#50141,#50142,#50143,#50144,#50145,#50146,#50147,
#50148,#50149,#50150,#50151,#50152,#50153,#50154,#50155,#50156,#50157,#50158,
#50159,#50160,#50161,#50162,#50163,#50164,#50165,#50166,#50167,#50168,#50169,
#50170,#50171,#50172,#50173,#50174,#50175,#50176,#50177,#50178,#50179,#50180,
#50181,#50182,#50183,#50184,#50185,#50186,#50187,#50188,#50189,#50190,#50191,
#50192,#50193,#50194,#50195,#50196,#50197,#50198,#50199,#50200,#50201,#50202,
#50203,#50204,#50205,#50206,#50207,#50208,#50209,#50210,#50211,#50212,#50213,
#50214,#50215,#50216,#50217,#50218,#50219,#50220,#50221,#50222,#50223,#50224,
#50225,#50226,#50227,#50228,#50229,#50230,#50231,#50232,#50233,#50234,#50235,
#50236,#50237,#50238),.UNSPECIFIED.,.F.,.F.,(4,3,3,3,3,3,3,3,3,3,3,3,3,
3,3,3,3,3,3,3,3,3,3,3,3,3,3,3,3,3,3,3,3,3,3,3,3,3,3,4),(0.00448635962221661,
0.00473358542950409,0.00476227051745122,0.00480233473052602,0.00482691085287281,
0.00484239894360081,0.00492023496407616,0.00508278422204955,0.00510688429789094,
0.00540329792664787,0.005480183189725,0.00572381163124619,0.00585348292348728,
0.00604432533584451,0.00622678424286061,0.00636483904044283,0.00641343584205939,
0.0064449674665924,0.00650676142924672,0.00652509589274198,0.00660008754740501,
0.00668535274504114,0.0069734073638536,0.00700586644963945,0.00706674043229878,
0.00708599487578904,0.00716007751974228,0.00732638015423778,0.00734684552356649,
0.00764689385883611,0.00772082703711819,0.00796740756343444,0.00809541822331551,
0.00828792126803276,0.0084706476028549,0.00860843497263109,0.00865852771923415,
0.00875251842491186,0.00884627452670677,0.00892894867722942),
 .UNSPECIFIED.);
#948=B_SPLINE_CURVE_WITH_KNOTS('',3,(#50246,#50247,#50248,#50249,#50250,
#50251,#50252,#50253,#50254,#50255,#50256,#50257,#50258,#50259,#50260,#50261,
#50262,#50263,#50264,#50265,#50266,#50267,#50268,#50269,#50270,#50271,#50272,
#50273,#50274,#50275,#50276,#50277,#50278,#50279,#50280,#50281,#50282,#50283,
#50284,#50285,#50286,#50287,#50288,#50289,#50290,#50291,#50292,#50293,#50294,
#50295,#50296,#50297,#50298,#50299,#50300,#50301,#50302,#50303,#50304,#50305,
#50306,#50307,#50308),.UNSPECIFIED.,.F.,.F.,(4,2,2,1,1,1,1,1,1,2,1,2,2,
1,1,1,1,1,1,2,2,2,1,2,2,2,1,1,1,1,1,2,2,2,1,1,1,2,2,1,1,1,1,1,4),(8.54252242016652E-18,
0.000160194806869816,0.000240292210304721,0.000320389613739627,0.000640779227479243,
0.000961168841218859,0.00128155845495848,0.00160194806869809,0.00192233768243771,
0.00224272729617732,0.00232282469961223,0.00236287340132968,0.00240292210304713,
0.00256311690991691,0.00288350652365649,0.00320389613739606,0.00352428575113563,
0.0038446753648752,0.00416506497861477,0.00448545459235434,0.00456555199578923,
0.00464564939922412,0.00480584420609392,0.00512623381983351,0.00528642862670331,
0.00536652603013821,0.00544662343357311,0.00576701304731269,0.00608740266105227,
0.00640779227479185,0.00672818188853143,0.00704857150227101,0.0072087663091408,
0.00728886371257569,0.00736896111601059,0.00768935072975016,0.00800974034348972,
0.00833012995722929,0.00849032476409908,0.00853037346581653,0.00857042216753398,
0.00865051957096888,0.00897090918470849,0.0092912987984481,0.00956209106146699),
 .UNSPECIFIED.);
#949=B_SPLINE_CURVE_WITH_KNOTS('',3,(#50310,#50311,#50312,#50313,#50314,
#50315,#50316,#50317,#50318,#50319,#50320,#50321,#50322,#50323,#50324,#50325,
#50326,#50327,#50328,#50329,#50330,#50331),.UNSPECIFIED.,.F.,.F.,(4,3,3,
3,3,3,3,4),(0.00956209106146699,0.00961168841218771,0.00976759725391833,
0.00980857291316444,0.00984954064048262,0.00993152890309068,0.0100957710509459,
0.0102524676396669),.UNSPECIFIED.);
#950=B_SPLINE_CURVE_WITH_KNOTS('',3,(#50332,#50333,#50334,#50335,#50336,
#50337,#50338,#50339,#50340,#50341,#50342,#50343,#50344,#50345,#50346,#50347,
#50348,#50349,#50350,#50351,#50352,#50353,#50354,#50355,#50356,#50357,#50358,
#50359,#50360,#50361,#50362,#50363,#50364,#50365,#50366,#50367,#50368,#50369,
#50370,#50371,#50372,#50373,#50374,#50375,#50376,#50377,#50378,#50379,#50380,
#50381,#50382,#50383,#50384,#50385,#50386,#50387,#50388,#50389,#50390,#50391,
#50392,#50393,#50394,#50395,#50396,#50397,#50398,#50399,#50400,#50401,#50402,
#50403,#50404,#50405,#50406,#50407,#50408,#50409,#50410,#50411,#50412,#50413,
#50414,#50415,#50416,#50417,#50418,#50419,#50420,#50421,#50422,#50423,#50424,
#50425,#50426,#50427,#50428,#50429,#50430,#50431,#50432,#50433,#50434,#50435,
#50436,#50437,#50438,#50439,#50440,#50441,#50442,#50443,#50444,#50445,#50446,
#50447,#50448,#50449,#50450,#50451,#50452,#50453,#50454,#50455,#50456,#50457,
#50458,#50459,#50460,#50461,#50462,#50463,#50464,#50465,#50466,#50467,#50468,
#50469,#50470,#50471,#50472,#50473,#50474,#50475,#50476,#50477,#50478,#50479,
#50480,#50481,#50482,#50483,#50484,#50485,#50486,#50487,#50488,#50489,#50490,
#50491,#50492,#50493,#50494,#50495,#50496,#50497,#50498,#50499,#50500,#50501,
#50502,#50503,#50504,#50505,#50506,#50507,#50508,#50509,#50510,#50511,#50512,
#50513,#50514,#50515,#50516,#50517,#50518,#50519,#50520,#50521,#50522,#50523,
#50524,#50525,#50526,#50527,#50528,#50529,#50530,#50531,#50532,#50533,#50534,
#50535,#50536,#50537,#50538,#50539,#50540,#50541,#50542,#50543,#50544,#50545,
#50546,#50547,#50548,#50549,#50550,#50551,#50552,#50553,#50554,#50555,#50556,
#50557,#50558,#50559,#50560,#50561,#50562,#50563,#50564,#50565,#50566,#50567,
#50568,#50569,#50570,#50571,#50572,#50573,#50574,#50575,#50576,#50577,#50578,
#50579,#50580,#50581,#50582,#50583,#50584,#50585,#50586,#50587,#50588,#50589,
#50590,#50591,#50592,#50593,#50594,#50595,#50596,#50597,#50598,#50599,#50600,
#50601,#50602,#50603,#50604,#50605,#50606,#50607,#50608,#50609,#50610,#50611,
#50612,#50613,#50614,#50615,#50616,#50617,#50618,#50619,#50620,#50621,#50622,
#50623,#50624,#50625,#50626,#50627,#50628,#50629,#50630,#50631,#50632,#50633,
#50634,#50635,#50636,#50637,#50638,#50639,#50640,#50641,#50642,#50643,#50644,
#50645,#50646,#50647,#50648,#50649,#50650,#50651,#50652,#50653,#50654,#50655,
#50656,#50657,#50658,#50659,#50660,#50661,#50662,#50663,#50664,#50665,#50666,
#50667,#50668,#50669,#50670,#50671,#50672,#50673,#50674,#50675,#50676,#50677,
#50678,#50679,#50680,#50681,#50682,#50683,#50684,#50685,#50686,#50687,#50688,
#50689,#50690,#50691,#50692,#50693,#50694,#50695,#50696,#50697,#50698,#50699,
#50700,#50701),.UNSPECIFIED.,.F.,.F.,(4,3,3,3,3,3,3,3,3,3,3,3,3,3,3,3,3,
3,3,3,3,3,3,3,3,3,3,3,3,3,3,3,3,3,3,3,3,3,3,3,3,3,3,3,3,3,3,3,3,3,3,3,3,
3,3,3,3,3,3,3,3,3,3,3,3,3,3,3,3,3,3,3,3,3,3,3,3,3,3,3,3,3,3,3,3,3,3,3,3,
3,3,3,3,3,3,3,3,3,3,3,3,3,3,3,3,3,3,3,3,3,3,3,3,3,3,3,3,3,3,3,3,3,3,4),
(2.59922340967641E-10,0.000262388289418012,0.000329189181563099,0.000467357547817636,
0.000524776578836023,0.000590373651190526,0.000605976118520986,0.00065597072354503,
0.000883792457061135,0.00104955315767209,0.00144104403044228,0.00157432973650817,
0.00200001764535897,0.00209910631534426,0.00256029609833201,0.00262388289418034,
0.00312154984340054,0.00314865947301643,0.00326198305548787,0.00327985361772545,
0.00334545069007997,0.00340244081200927,0.00341104776243449,0.00367343605185254,
0.00368317018991879,0.00419821263068866,0.00424371040228981,0.00472298920952478,
0.00480285009820333,0.0052477657883609,0.00536037435326884,0.00577254236719702,
0.00591605037941538,0.00603493065661509,0.00605465039573207,0.00612389765881176,
0.00616612480132412,0.00619309863725878,0.00629731894603315,0.00646939602860005,
0.0067448599582135,0.00682209552486926,0.0068822653254087,0.00695328966957829,
0.00701944169990729,0.00708448381428732,0.00734687210370539,0.00756558389005768,
0.00787164868254153,0.0081074466846592,0.0081340369719596,0.00837667669017726,
0.00839642526137767,0.00844379880569796,0.00846202233373219,0.00851084615263126,
0.0085276194060867,0.00864473211587614,0.00865881355079574,0.00892120184021382,
0.00917757482779576,0.0091835901296319,0.00944234903430452,0.00944597841904998,
0.00970599790514705,0.00970836670846806,0.00983739163427776,0.00983956085317709,
0.00990297905228762,0.00990515792553161,0.00993795646170887,0.00996850338831347,
0.00997075499788612,0.0102302598050392,0.0104914878165698,0.0104955315767223,
0.0107521972284278,0.0107579198661403,0.0110123944037893,0.0110203081555584,
0.0112720829688689,0.0112826964449765,0.011348293517331,0.0113810920535082,
0.0114017360867843,0.0114138905896855,0.0115313481146533,0.0115450847343945,
0.0117907037577083,0.0118074730238126,0.0120502249089893,0.0120698613132307,
0.0123098994004552,0.0123322496026488,0.0125946378920669,0.012829666102776,
0.012857026181485,0.0129882203261941,0.0130538173985486,0.013089795720895,
0.0131194144709031,0.0131550420289316,0.0132203550964659,0.0133511192354543,
0.0133818027603212,0.0136441910497393,0.0138755852809746,0.0139065793391574,
0.0141689676285755,0.0144021169982843,0.0146937442074117,0.0149304527077196,
0.0149561324968298,0.0150217295691844,0.0150627981915921,0.0150873266415389,
0.015195189240927,0.0152185207862479,0.0154599955937371,0.0157432973650841,
0.0159896040980766,0.0162680739439203,0.016519074845501,0.0167928505227559),
 .UNSPECIFIED.);
#951=B_SPLINE_CURVE_WITH_KNOTS('',3,(#51506,#51507,#51508,#51509,#51510,
#51511,#51512,#51513,#51514,#51515,#51516,#51517,#51518,#51519,#51520,#51521,
#51522,#51523,#51524,#51525,#51526,#51527,#51528,#51529,#51530,#51531,#51532,
#51533,#51534,#51535,#51536,#51537,#51538,#51539,#51540,#51541,#51542,#51543,
#51544,#51545,#51546,#51547,#51548,#51549,#51550,#51551,#51552,#51553,#51554,
#51555,#51556,#51557,#51558,#51559,#51560,#51561,#51562,#51563,#51564,#51565,
#51566,#51567,#51568,#51569,#51570,#51571,#51572,#51573,#51574,#51575,#51576,
#51577,#51578,#51579,#51580,#51581,#51582,#51583,#51584,#51585,#51586,#51587,
#51588,#51589,#51590,#51591,#51592,#51593,#51594,#51595,#51596,#51597,#51598,
#51599,#51600,#51601,#51602,#51603,#51604,#51605,#51606,#51607,#51608,#51609,
#51610,#51611,#51612,#51613,#51614,#51615,#51616,#51617,#51618,#51619,#51620,
#51621,#51622,#51623,#51624),.UNSPECIFIED.,.F.,.F.,(4,2,1,1,1,1,1,1,2,2,
2,1,2,1,1,1,1,1,2,1,2,2,1,1,1,1,1,2,2,2,1,1,1,1,1,1,2,2,2,1,1,1,1,1,1,2,
2,2,1,1,1,1,1,1,2,2,2,1,1,1,1,1,1,2,1,2,2,1,1,1,1,1,2,2,2,1,1,1,1,1,1,2,
1,2,2,1,1,4),(0.000691744478869641,0.000711184477407308,0.00081278225989404,
0.00121917338984095,0.00162556451978785,0.00203195564973476,0.00243834677968166,
0.00284473790962857,0.00325112903957547,0.00335272682206222,0.00345432460454896,
0.0035559223870357,0.00365752016952244,0.00406391129946942,0.00447030242941641,
0.00487669355936339,0.00528308468931038,0.00568947581925736,0.00609586694920435,
0.00629906251417784,0.00640066029666459,0.00650225807915134,0.00690864920909835,
0.00731504033904536,0.00772143146899237,0.00812782259893938,0.00853421372888639,
0.0089406048588334,0.00904220264132015,0.00909300153256353,0.00914380042380691,
0.00934699598878044,0.00975338711872751,0.0101597782486746,0.0105661693786217,
0.0109725605085687,0.0113789516385158,0.0114805494210026,0.0115313483122459,
0.0115821472034893,0.0117853427684629,0.0121917338984099,0.012598125028357,
0.0130045161583041,0.0134109072882511,0.0138172984181982,0.0140204939831718,
0.0141220917656585,0.0142236895481453,0.0146300806780924,0.0150364718080394,
0.0154428629379865,0.0158492540679336,0.0162556451978807,0.0166620363278277,
0.0168652318928013,0.016966829675288,0.0170684274577748,0.0174748185877219,
0.017881209717669,0.0182876008476161,0.0186939919775632,0.0191003831075103,
0.0195067742374574,0.0197099698024309,0.0198115675849177,0.0199131653674045,
0.0203195564973515,0.0207259476272986,0.0211323387572457,0.0215387298871928,
0.0219451210171399,0.022351512147087,0.0224531099295737,0.0225039088208171,
0.0225547077120605,0.0227579032770339,0.0231642944069809,0.0235706855369278,
0.0239770766668748,0.0243834677968217,0.0247898589267687,0.0249930544917421,
0.0250946522742289,0.0251454511654722,0.0251962500567156,0.0256026411866625,
0.0259925502271156),.UNSPECIFIED.);
#952=B_SPLINE_CURVE_WITH_KNOTS('',3,(#51628,#51629,#51630,#51631,#51632,
#51633,#51634,#51635,#51636,#51637,#51638,#51639),.UNSPECIFIED.,.F.,.F.,
(4,2,2,2,2,4),(0.193494937972427,0.221478557046408,0.257021340074901,0.304852388878296,
0.36775906785294,0.368268523654839),.UNSPECIFIED.);
#953=B_SPLINE_CURVE_WITH_KNOTS('',3,(#51648,#51649,#51650,#51651,#51652,
#51653,#51654,#51655,#51656,#51657,#51658,#51659,#51660,#51661,#51662,#51663,
#51664,#51665,#51666,#51667,#51668,#51669,#51670,#51671,#51672,#51673,#51674,
#51675,#51676,#51677,#51678,#51679,#51680,#51681,#51682,#51683,#51684,#51685,
#51686,#51687,#51688,#51689,#51690,#51691,#51692,#51693,#51694,#51695,#51696,
#51697,#51698,#51699,#51700,#51701,#51702,#51703,#51704,#51705,#51706,#51707,
#51708,#51709,#51710,#51711,#51712,#51713,#51714,#51715,#51716,#51717,#51718,
#51719,#51720,#51721,#51722,#51723,#51724,#51725,#51726,#51727,#51728,#51729,
#51730,#51731,#51732,#51733,#51734,#51735,#51736,#51737,#51738,#51739,#51740,
#51741,#51742,#51743,#51744,#51745,#51746,#51747,#51748,#51749,#51750,#51751,
#51752,#51753,#51754,#51755,#51756,#51757,#51758,#51759,#51760,#51761,#51762,
#51763,#51764,#51765,#51766,#51767,#51768,#51769,#51770,#51771,#51772,#51773),
 .UNSPECIFIED.,.F.,.F.,(4,1,1,1,1,2,2,2,2,2,1,1,1,1,1,1,1,2,2,2,1,1,1,1,
1,1,2,1,2,2,1,1,1,1,2,1,2,2,1,1,1,1,1,1,2,2,1,1,1,1,1,1,2,1,1,2,2,1,1,1,
1,1,1,2,2,2,1,1,1,1,1,1,2,1,2,2,1,1,1,1,1,2,2,2,1,1,1,1,2,1,1,1,2,4),(0.0267086453492391,
0.0268218145765036,0.0272282057064507,0.0276345968363977,0.0280409879663448,
0.0284473790962919,0.0286505746612654,0.0287521724437522,0.0288537702262389,
0.0289553680087257,0.0290569657912125,0.029260161356186,0.029666552486133,
0.0300729436160801,0.0304793347460271,0.0308857258759742,0.0312921170059213,
0.0316985081358683,0.0317493070271117,0.0318001059183551,0.0319017037008419,
0.0321048992658154,0.0325112903957626,0.0329176815257097,0.0333240726556568,
0.0337304637856039,0.0341368549155511,0.0343400504805246,0.0344416482630114,
0.0345432460454982,0.0349496371754453,0.0353560283053924,0.0357624194353395,
0.0361688105652867,0.0365752016952338,0.0367783972602073,0.0368799950426941,
0.0369307939339375,0.0369815928251809,0.0373879839551279,0.037794375085075,
0.0382007662150221,0.0386071573449691,0.0390135484749162,0.0394199396048632,
0.03952153738735,0.0396231351698367,0.0398263307348103,0.0402327218647573,
0.0406391129947044,0.0410455041246514,0.0414518952545985,0.0418582863845456,
0.0420614819495191,0.0421630797320059,0.0422138786232492,0.0422646775144926,
0.0426710686444397,0.0430774597743867,0.0434838509043337,0.0438902420342808,
0.0442966331642278,0.0447030242941749,0.0451094154241219,0.0451602143153653,
0.0452110132066086,0.0453126109890954,0.0455158065540689,0.0459221976840159,
0.0463285888139629,0.04673497994391,0.047141371073857,0.047547762203804,
0.0477509577687775,0.0478017566600209,0.0478525555512643,0.047954153333751,
0.0483605444636982,0.0487669355936454,0.0491733267235925,0.0495797178535397,
0.0499861089834869,0.0501893045484605,0.0502401034397039,0.0502909023309472,
0.050392500113434,0.0507988912433812,0.0512052823733283,0.0516116735032755,
0.051814869068249,0.0519164668507358,0.0519672657419792,0.0520053649104118,
0.0520180646332226),.UNSPECIFIED.);
#954=B_SPLINE_CURVE_WITH_KNOTS('',3,(#51778,#51779,#51780,#51781,#51782,
#51783,#51784,#51785,#51786,#51787,#51788,#51789,#51790,#51791,#51792,#51793,
#51794,#51795,#51796,#51797,#51798,#51799,#51800,#51801,#51802,#51803,#51804,
#51805,#51806,#51807,#51808,#51809,#51810,#51811,#51812,#51813,#51814,#51815,
#51816,#51817,#51818,#51819,#51820,#51821,#51822,#51823,#51824,#51825,#51826,
#51827,#51828,#51829,#51830,#51831,#51832,#51833,#51834,#51835,#51836,#51837,
#51838,#51839,#51840,#51841,#51842,#51843,#51844,#51845,#51846,#51847,#51848),
 .UNSPECIFIED.,.F.,.F.,(4,1,1,1,1,1,2,2,1,1,1,1,1,1,1,2,2,2,1,2,2,1,1,1,
1,1,1,2,2,2,1,1,1,1,1,1,2,1,2,2,1,1,1,1,2,1,2,2,1,1,1,1,4),(2.81851621706032E-10,
0.000430383770082051,0.000860767540164102,0.00129115131024615,0.0017215350803282,
0.00215191885041026,0.00258230262049231,0.00263610059175256,0.00268989856301282,
0.00279749450553333,0.00301268639057435,0.0034430701606564,0.00387345393073844,
0.00430383770082048,0.00473422147090253,0.00516460524098457,0.00537979712602559,
0.0054873930685461,0.00559498901106661,0.00581018089610763,0.00602537278114865,
0.00645575655123069,0.00688614032131272,0.00731652409139476,0.0077469078614768,
0.00817729163155883,0.00860767540164087,0.00903805917172291,0.00909185714298317,
0.00914565511424342,0.00925325105676395,0.00946844294180499,0.00989882671188708,
0.0103292104819692,0.0107595942520513,0.0111899780221333,0.0116203617922154,
0.0118355536772565,0.011943149619777,0.0120507455622975,0.0124811293323796,
0.0129115131024617,0.0133418968725438,0.013772280642626,0.0142026644127081,
0.0144178562977491,0.0145254522402697,0.0146330481827902,0.0150634319528723,
0.0154938157229543,0.0159241994930364,0.0163545832631185,0.0167022853636743),
 .UNSPECIFIED.);
#955=B_SPLINE_CURVE_WITH_KNOTS('',3,(#51850,#51851,#51852,#51853,#51854,
#51855,#51856,#51857,#51858,#51859,#51860,#51861,#51862,#51863,#51864,#51865,
#51866,#51867,#51868,#51869,#51870,#51871,#51872,#51873,#51874,#51875,#51876,
#51877,#51878,#51879,#51880,#51881,#51882,#51883,#51884,#51885,#51886,#51887,
#51888,#51889,#51890,#51891,#51892,#51893,#51894,#51895,#51896,#51897,#51898,
#51899,#51900,#51901,#51902,#51903,#51904,#51905,#51906,#51907,#51908,#51909,
#51910,#51911,#51912,#51913,#51914,#51915,#51916,#51917,#51918,#51919,#51920,
#51921,#51922,#51923,#51924,#51925,#51926,#51927,#51928,#51929,#51930,#51931,
#51932,#51933,#51934,#51935,#51936,#51937,#51938,#51939,#51940,#51941,#51942,
#51943,#51944,#51945,#51946,#51947,#51948,#51949,#51950,#51951,#51952,#51953,
#51954,#51955,#51956,#51957,#51958,#51959,#51960,#51961,#51962,#51963,#51964,
#51965,#51966,#51967,#51968,#51969,#51970,#51971),.UNSPECIFIED.,.F.,.F.,
(4,2,1,1,2,2,1,1,1,1,1,2,1,1,1,1,1,1,2,2,2,1,1,1,1,1,1,2,1,2,2,1,1,1,1,
1,1,2,1,2,2,1,1,1,1,1,1,2,2,1,1,1,1,1,1,1,1,2,2,2,1,1,1,1,1,1,2,2,2,1,1,
1,1,1,1,2,1,2,2,1,1,1,1,2,1,2,2,1,1,1,1,1,4),(0.0167022853636743,0.0167849670332005,
0.0170001589182416,0.0171077548607621,0.0171615528320224,0.0172153508032826,
0.0176457345733647,0.0180761183434467,0.0185065021135288,0.0189368858836108,
0.0193672696536929,0.0197976534237749,0.020228037193857,0.020658420963939,
0.0210888047340211,0.0215191885041031,0.0219495722741852,0.0223799560442672,
0.0228103398143493,0.0230255316993903,0.0231331276419108,0.0232407235844313,
0.0236711073545133,0.0241014911245954,0.0245318748946774,0.0249622586647594,
0.0253926424348414,0.0258230262049235,0.0260382180899645,0.0260920160612247,
0.026145814032485,0.0262534099750055,0.0266837937450876,0.0271141775151697,
0.0275445612852518,0.0279749450553339,0.028405328825416,0.0288357125954981,
0.0290509044805392,0.0291047024517994,0.0291585004230597,0.0292660963655802,
0.0296964801356624,0.0301268639057445,0.0305572476758266,0.0309876314459087,
0.0314180152159908,0.0318483989860729,0.0319021969573332,0.0319559949285935,
0.032063590871114,0.0322787827561551,0.0327091665262372,0.0331395502963193,
0.0335699340664014,0.0340003178364836,0.0344307016065657,0.0348610853766478,
0.0350762772616889,0.0352914691467299,0.0357218529168121,0.0361522366868942,
0.0365826204569763,0.0370130042270585,0.0374433879971406,0.0378737717672227,
0.0383041555373048,0.0383579535085651,0.0384117514798254,0.0385193474223459,
0.038734539307387,0.0391649230774692,0.0395953068475513,0.0400256906176335,
0.0404560743877157,0.0408864581577978,0.0411016500428389,0.0412092459853594,
0.0413168419278799,0.0417472256979621,0.0421776094680442,0.0426079932381263,
0.0430383770082085,0.0434687607782906,0.0436839526633316,0.0437377506345919,
0.0437915486058522,0.0438991445483727,0.0443295283184549,0.044759912088537,
0.0451902958586192,0.0456206796287013,0.0457216170362868),.UNSPECIFIED.);
#956=B_SPLINE_CURVE_WITH_KNOTS('',3,(#51973,#51974,#51975,#51976,#51977,
#51978,#51979,#51980,#51981,#51982,#51983,#51984,#51985,#51986,#51987,#51988,
#51989,#51990,#51991,#51992,#51993,#51994,#51995,#51996,#51997,#51998,#51999,
#52000,#52001,#52002,#52003,#52004,#52005,#52006,#52007,#52008,#52009,#52010,
#52011,#52012,#52013,#52014,#52015,#52016,#52017,#52018,#52019,#52020,#52021,
#52022,#52023,#52024,#52025,#52026,#52027,#52028,#52029,#52030,#52031,#52032,
#52033,#52034,#52035,#52036,#52037,#52038,#52039,#52040,#52041,#52042,#52043,
#52044,#52045,#52046,#52047,#52048,#52049,#52050,#52051,#52052,#52053,#52054,
#52055,#52056,#52057,#52058,#52059,#52060,#52061,#52062,#52063,#52064,#52065,
#52066,#52067,#52068,#52069,#52070,#52071,#52072,#52073,#52074,#52075,#52076,
#52077,#52078,#52079,#52080,#52081,#52082,#52083,#52084,#52085,#52086,#52087,
#52088,#52089,#52090,#52091,#52092,#52093,#52094,#52095,#52096,#52097,#52098,
#52099,#52100,#52101,#52102,#52103,#52104,#52105,#52106,#52107,#52108,#52109,
#52110,#52111,#52112,#52113,#52114,#52115,#52116,#52117),.UNSPECIFIED.,
 .F.,.F.,(4,3,3,3,3,3,3,3,3,3,3,3,3,3,3,3,3,3,3,3,3,3,3,3,3,3,3,3,3,3,3,
3,3,3,3,3,3,3,3,3,3,3,3,3,3,3,3,3,4),(0.0457216170362868,0.0459525676539145,
0.0460510633987835,0.0462662552838245,0.046373851226345,0.0463932769063991,
0.0464814471688656,0.0465034399505402,0.0466136393573502,0.046834101971899,
0.0469118309389477,0.0473422147090298,0.0477171542116892,0.047772598479112,
0.0482029822491941,0.0486019149928958,0.0486333660192762,0.0490448701065293,
0.0490637497893583,0.0491175477606186,0.0491556645204495,0.0491713457318789,
0.0492664939120745,0.0492789416743994,0.0494882446468033,0.0499245173295227,
0.0503549010996049,0.0503763267500335,0.0507852848696871,0.0512156686397693,
0.0512657528394623,0.0516460524098514,0.0520764361799336,0.0521560599808391,
0.0522673906331406,0.0522916280649747,0.0523787273298763,0.0523992240074953,
0.0525068199500158,0.0526013663393763,0.052937203720098,0.05304644767749,
0.0533675874901802,0.0537979712602624,0.0539356438209761,0.0542283550303446,
0.0546587388004268,0.0548232174784346,0.055089122570509),.UNSPECIFIED.);
#957=B_SPLINE_CURVE_WITH_KNOTS('',3,(#52126,#52127,#52128,#52129,#52130,
#52131),.UNSPECIFIED.,.F.,.F.,(4,2,4),(-0.349779142867042,-0.290997733300589,
-0.252766120019253),.UNSPECIFIED.);
#958=B_SPLINE_CURVE_WITH_KNOTS('',3,(#52145,#52146,#52147,#52148,#52149,
#52150,#52151,#52152,#52153,#52154,#52155,#52156,#52157,#52158,#52159,#52160,
#52161,#52162),.UNSPECIFIED.,.F.,.F.,(4,2,2,2,2,2,2,2,4),(-1.81830740171076,
-1.66679770229951,-1.51528800288825,-1.36374646868162,-1.21220493447498,
-1.06066340026809,-0.909121866061206,-0.757612166650203,-0.606102467239199),
 .UNSPECIFIED.);
#959=B_SPLINE_CURVE_WITH_KNOTS('',3,(#52163,#52164,#52165,#52166,#52167,
#52168,#52169,#52170,#52171,#52172,#52173,#52174,#52175,#52176,#52177,#52178,
#52179,#52180,#52181),.UNSPECIFIED.,.F.,.F.,(4,2,2,2,3,2,2,2,4),(-0.606102467239199,
-0.454592767826692,-0.303083068414184,-0.151541534207092,0.,0.151541534207344,
0.303083068414688,0.454592767826944,0.6061024672392),.UNSPECIFIED.);
#960=B_SPLINE_CURVE_WITH_KNOTS('',3,(#52184,#52185,#52186,#52187,#52188,
#52189,#52190,#52191,#52192,#52193,#52194,#52195,#52196,#52197,#52198,#52199,
#52200,#52201,#52202),.UNSPECIFIED.,.F.,.F.,(4,2,2,2,3,2,2,2,4),(1.81830740171076,
1.96981710112327,2.12132680053578,2.27286833474287,2.42440986894996,2.57595140315705,
2.72749293736415,2.87900263677665,3.03051233618916),.UNSPECIFIED.);
#961=B_SPLINE_CURVE_WITH_KNOTS('',3,(#52203,#52204,#52205,#52206,#52207,
#52208,#52209,#52210,#52211,#52212,#52213,#52214,#52215,#52216,#52217,#52218,
#52219,#52220),.UNSPECIFIED.,.F.,.F.,(4,2,2,2,2,2,2,2,4),(3.03051233618916,
3.18202203560017,3.33353173501117,3.48507326921806,3.63661480342494,3.78815633763183,
3.93969787183872,4.09120757124972,4.24271727066072),.UNSPECIFIED.);
#962=B_SPLINE_CURVE_WITH_KNOTS('',3,(#53022,#53023,#53024,#53025,#53026,
#53027,#53028,#53029,#53030,#53031,#53032,#53033,#53034,#53035,#53036,#53037,
#53038,#53039,#53040,#53041,#53042,#53043,#53044,#53045,#53046,#53047,#53048,
#53049,#53050,#53051,#53052,#53053,#53054,#53055,#53056,#53057,#53058,#53059,
#53060,#53061,#53062,#53063,#53064,#53065,#53066,#53067,#53068,#53069,#53070,
#53071,#53072,#53073,#53074,#53075,#53076,#53077,#53078,#53079,#53080,#53081,
#53082,#53083,#53084,#53085,#53086,#53087,#53088,#53089,#53090,#53091,#53092,
#53093,#53094,#53095,#53096,#53097,#53098,#53099,#53100,#53101,#53102,#53103,
#53104,#53105,#53106,#53107,#53108,#53109,#53110,#53111,#53112,#53113,#53114,
#53115,#53116,#53117,#53118,#53119,#53120,#53121,#53122,#53123,#53124,#53125,
#53126,#53127,#53128,#53129,#53130,#53131,#53132,#53133,#53134,#53135,#53136,
#53137,#53138,#53139,#53140,#53141,#53142,#53143,#53144,#53145,#53146,#53147,
#53148,#53149,#53150,#53151,#53152,#53153,#53154,#53155,#53156,#53157,#53158,
#53159,#53160,#53161,#53162,#53163,#53164,#53165,#53166,#53167,#53168,#53169,
#53170,#53171,#53172,#53173,#53174,#53175,#53176,#53177,#53178,#53179,#53180,
#53181,#53182,#53183,#53184,#53185,#53186,#53187,#53188,#53189,#53190,#53191,
#53192,#53193,#53194,#53195,#53196,#53197,#53198,#53199,#53200,#53201,#53202,
#53203,#53204,#53205,#53206,#53207,#53208,#53209,#53210,#53211,#53212,#53213,
#53214,#53215,#53216,#53217,#53218,#53219,#53220,#53221,#53222,#53223,#53224,
#53225,#53226,#53227,#53228,#53229,#53230,#53231,#53232,#53233,#53234,#53235,
#53236,#53237,#53238,#53239,#53240,#53241,#53242,#53243,#53244,#53245,#53246,
#53247,#53248,#53249,#53250,#53251,#53252,#53253,#53254,#53255,#53256,#53257,
#53258,#53259,#53260,#53261,#53262,#53263,#53264,#53265,#53266,#53267,#53268,
#53269,#53270,#53271,#53272,#53273,#53274,#53275,#53276,#53277,#53278,#53279,
#53280,#53281,#53282,#53283,#53284,#53285,#53286,#53287,#53288,#53289,#53290,
#53291,#53292,#53293,#53294,#53295,#53296,#53297,#53298,#53299,#53300,#53301,
#53302,#53303,#53304,#53305,#53306,#53307,#53308,#53309,#53310,#53311,#53312,
#53313,#53314,#53315,#53316,#53317,#53318,#53319,#53320,#53321,#53322,#53323,
#53324,#53325,#53326,#53327,#53328,#53329,#53330,#53331,#53332,#53333,#53334,
#53335,#53336,#53337,#53338,#53339,#53340,#53341,#53342,#53343,#53344,#53345,
#53346,#53347,#53348,#53349,#53350,#53351,#53352,#53353,#53354,#53355,#53356,
#53357,#53358,#53359,#53360,#53361,#53362,#53363,#53364,#53365,#53366,#53367,
#53368,#53369,#53370,#53371,#53372,#53373,#53374,#53375,#53376,#53377,#53378,
#53379,#53380,#53381,#53382,#53383,#53384,#53385,#53386,#53387,#53388,#53389,
#53390,#53391,#53392,#53393,#53394,#53395,#53396,#53397,#53398,#53399,#53400,
#53401,#53402,#53403,#53404,#53405,#53406,#53407,#53408,#53409,#53410,#53411,
#53412,#53413,#53414,#53415,#53416,#53417,#53418),.UNSPECIFIED.,.F.,.F.,
(4,3,3,3,3,3,3,3,3,3,3,3,3,3,3,3,3,3,3,3,3,3,3,3,3,3,3,3,3,3,3,3,3,3,3,
3,3,3,3,3,3,3,3,3,3,3,3,3,3,3,3,3,3,3,3,3,3,3,3,3,3,3,3,3,3,3,3,3,3,3,3,
3,3,3,3,3,3,3,3,3,3,3,3,3,3,3,3,3,3,3,3,3,3,3,3,3,3,3,3,3,3,3,3,3,3,3,3,
3,3,3,3,3,3,3,3,3,3,3,3,3,3,3,3,3,3,3,3,3,3,3,3,3,4),(0.000484419199971794,
0.000627975952031815,0.000633556641722834,0.000937055221123302,0.000941963928047723,
0.00124047713506422,0.00125595190406363,0.0015438228113822,0.00156993988007954,
0.00172693386808749,0.00180543086209147,0.00184712765684463,0.00188392785609545,
0.0019231050380993,0.00199911452758639,0.00215120575891999,0.00219791583211137,
0.00245570735767525,0.00251190380812729,0.00276063659439479,0.00282589178414321,
0.00313987976015913,0.00337182000724591,0.00345386773617505,0.00352490446840894,
0.00353236473017903,0.00361086172418301,0.00367813944513374,0.00376785571219098,
0.00398516274434557,0.0040818436882069,0.00439583166422282,0.00460142477316655,
0.00470981964023874,0.00491068197299154,0.00502380761625467,0.00506559805970609,
0.005143130947568,0.00518080160426262,0.00522005010126462,0.00522070868137605,
0.00525929859826661,0.00565178356828666,0.00584312899461437,0.00596577154430269,
0.00627975952031873,0.00646865865529118,0.00690773547235079,0.00709724487102262,
0.00717602996170373,0.00722172344836684,0.00725485607089141,0.00730022044237085,
0.00737871743637487,0.00741262727130941,0.00753571142438291,0.00772857997468013,
0.00816368737641506,0.00836205996678017,0.00879166332844721,0.00899754377132439,
0.00941963928047937,0.0096349306909179,0.00973362725649546,0.00979456994957919,
0.0098906212445035,0.00995430020341104,0.0100476152325115,0.010273940467961,
0.0106755911845437,0.0109137046578717,0.0113035671365759,0.0115540605555347,
0.0119315430886081,0.0121949278647927,0.0125595190406403,0.0128362231911716,
0.0131570039176619,0.0131874949926725,0.0133174226179354,0.0133444889806806,
0.0134778312741732,0.0135014829686886,0.0138154709447047,0.0141189436345339,
0.0144434468967369,0.0147591048294073,0.0150714228487691,0.0153981466426708,
0.0156993988008013,0.0160133867768174,0.0160358430959,0.0163273747528335,
0.0163540945915774,0.0164843687408416,0.0165130520803898,0.0165628657348456,
0.0166413627288497,0.0166718779414906,0.0169553507048658,0.0172693386808819,
0.0173052583666035,0.0175833266568981,0.0176206583646067,0.0178973146329142,
0.0179350856965279,0.0182113026089303,0.0182484317842081,0.0184046583785325,
0.0184826536878379,0.0185252905849465,0.0185605610228719,0.0185645390819485,
0.0186037875789505,0.0186822845729545,0.0188392785609626,0.0188708516293508,
0.0191532665369787,0.0191787177616934,0.0194672545129949,0.0194839639398301,
0.0196242485010029,0.019663496998005,0.019702745495007,0.019781242489011,
0.019786707220997,0.0199382364770191,0.0199386450109174,0.0200149458360611,
0.0200167334710231,0.0200913742141244,0.0200952304650272,0.0203967023487183),
 .UNSPECIFIED.);
#963=B_SPLINE_CURVE_WITH_KNOTS('',3,(#53436,#53437,#53438,#53439,#53440,
#53441,#53442,#53443,#53444,#53445),.UNSPECIFIED.,.F.,.F.,(4,2,2,2,4),(-0.0798726046250498,
-0.058584918995045,-0.0372972333650401,-0.0186486166825216,-3.09474668114262E-15),
 .UNSPECIFIED.);
#964=B_SPLINE_CURVE_WITH_KNOTS('',3,(#53449,#53450,#53451,#53452,#53453,
#53454,#53455,#53456,#53457,#53458),.UNSPECIFIED.,.F.,.F.,(4,2,2,2,4),(0.,
0.0191590048998788,0.0383180097997576,0.0590954157667988,0.07987282173384),
 .UNSPECIFIED.);
#965=B_SPLINE_CURVE_WITH_KNOTS('',3,(#53462,#53463,#53464,#53465,#53466,
#53467,#53468,#53469,#53470,#53471),.UNSPECIFIED.,.F.,.F.,(4,2,2,2,4),(-0.0798726046250503,
-0.0585849189950454,-0.0372972333650404,-0.0186486166825219,-3.33066907387547E-15),
 .UNSPECIFIED.);
#966=B_SPLINE_CURVE_WITH_KNOTS('',3,(#53474,#53475,#53476,#53477,#53478,
#53479,#53480,#53481,#53482,#53483),.UNSPECIFIED.,.F.,.F.,(4,2,2,2,4),(-0.329829240504479,
-0.311180623821963,-0.292532007139446,-0.271244321509442,-0.249956635879439),
 .UNSPECIFIED.);
#967=B_SPLINE_CURVE_WITH_KNOTS('',3,(#53493,#53494,#53495,#53496,#53497,
#53498,#53499,#53500,#53501,#53502,#53503,#53504,#53505,#53506),
 .UNSPECIFIED.,.F.,.F.,(4,2,2,2,2,1,1,4),(0.,0.000277353300508432,0.000554706601016864,
0.000693383251271085,0.000728052413834634,0.000762721576398184,0.000832059901525293,
0.00110941320203372),.UNSPECIFIED.);
#968=B_SPLINE_CURVE_WITH_KNOTS('',3,(#53508,#53509,#53510,#53511,#53512,
#53513,#53514,#53515,#53516,#53517,#53518,#53519,#53520,#53521,#53522,#53523,
#53524,#53525,#53526,#53527,#53528,#53529,#53530,#53531,#53532,#53533,#53534,
#53535),.UNSPECIFIED.,.F.,.F.,(4,3,3,3,3,3,3,3,3,4),(-0.000640854183641207,
-0.000630840837021816,-0.000620827490402424,-0.000600800797163639,-0.00059215928153463,
-0.000560747410686068,-0.000480640637730918,-0.000320427091820608,-0.000103815349030914,
0.),.UNSPECIFIED.);
#969=B_SPLINE_CURVE_WITH_KNOTS('',3,(#53536,#53537,#53538,#53539,#53540,
#53541,#53542,#53543,#53544,#53545,#53546,#53547,#53548,#53549,#53550,#53551,
#53552,#53553,#53554,#53555,#53556,#53557,#53558,#53559,#53560,#53561,#53562,
#53563,#53564,#53565,#53566),.UNSPECIFIED.,.F.,.F.,(4,3,3,3,3,3,3,3,3,3,
4),(0.000821733649844019,0.00095608668379176,0.00102326333982933,0.00109043999586689,
0.00115888309266042,0.00122479330794202,0.00129196996397958,0.00132555829199836,
0.00134235245600775,0.00135074953801244,0.00135914662001713),
 .UNSPECIFIED.);
#970=B_SPLINE_CURVE_WITH_KNOTS('',3,(#53570,#53571,#53572,#53573,#53574,
#53575,#53576,#53577,#53578,#53579,#53580,#53581),.UNSPECIFIED.,.F.,.F.,
(4,2,2,2,2,4),(-3.10489780410495,-3.10241912589423,-3.00106326608238,-2.79835154645867,
-2.60059139286912,-2.40283123927957),.UNSPECIFIED.);
#971=B_SPLINE_CURVE_WITH_KNOTS('',3,(#53583,#53584,#53585,#53586,#53587,
#53588,#53589,#53590,#53591,#53592,#53593,#53594,#53595,#53596,#53597,#53598,
#53599,#53600,#53601,#53602,#53603,#53604),.UNSPECIFIED.,.F.,.F.,(4,2,2,
2,2,2,2,2,2,2,4),(0.800943746426511,0.998703900016066,1.19646405360562,
1.39917577322933,1.50053163304119,1.60188749285304,1.70324335266489,1.80459921247675,
2.00731093210046,2.20507108569001,2.35815643982996),.UNSPECIFIED.);
#972=B_SPLINE_CURVE_WITH_KNOTS('',3,(#53606,#53607,#53608,#53609,#53610,
#53611,#53612,#53613,#53614,#53615,#53616,#53617,#53618,#53619,#53620,#53621,
#53622,#53623,#53624),.UNSPECIFIED.,.F.,.F.,(4,3,3,3,3,3,4),(0.00615127099246931,
0.00628627180839864,0.00635377221636331,0.00642127262432798,0.00669127425618666,
0.00696127588804534,0.00723127751990402),.UNSPECIFIED.);
#973=B_SPLINE_CURVE_WITH_KNOTS('',3,(#53626,#53627,#53628,#53629,#53630,
#53631,#53632,#53633,#53634,#53635,#53636,#53637,#53638,#53639,#53640,#53641,
#53642,#53643,#53644,#53645,#53646,#53647,#53648,#53649,#53650,#53651,#53652,
#53653,#53654,#53655,#53656,#53657,#53658,#53659,#53660,#53661,#53662,#53663,
#53664,#53665,#53666,#53667,#53668,#53669,#53670,#53671,#53672,#53673,#53674,
#53675,#53676,#53677,#53678,#53679,#53680,#53681,#53682,#53683),
 .UNSPECIFIED.,.F.,.F.,(4,3,3,3,3,3,3,3,3,3,3,3,3,3,3,3,3,3,3,4),(0.00228250782718276,
0.00261772248031453,0.00276610322284359,0.00288700207175879,0.003007900920674,
0.00324969861850441,0.00357540633747326,0.00373329401416523,0.00406460842083867,
0.00421688940982604,0.00445868710765645,0.00451913653211405,0.00457958595657165,
0.00470048480548686,0.00502296949144011,0.00518408020114767,0.00542587789897808,
0.00566767559680849,0.0059094732946389,0.00615127099246931),
 .UNSPECIFIED.);
#974=B_SPLINE_CURVE_WITH_KNOTS('',3,(#53687,#53688,#53689,#53690,#53691,
#53692,#53693,#53694,#53695,#53696,#53697,#53698,#53699,#53700,#53701,#53702,
#53703,#53704,#53705,#53706),.UNSPECIFIED.,.F.,.F.,(4,2,2,2,2,2,2,2,2,4),
(0.850611926930939,0.998703900016074,1.19646405360563,1.39917577322933,
1.50053163304119,1.60188749285304,1.7032433526649,1.80459921247675,2.00731093210046,
2.1806981097713),.UNSPECIFIED.);
#975=B_SPLINE_CURVE_WITH_KNOTS('',3,(#53714,#53715,#53716,#53717,#53718,
#53719,#53720,#53721,#53722,#53723,#53724,#53725,#53726,#53727,#53728,#53729,
#53730,#53731,#53732,#53733,#53734,#53735,#53736,#53737,#53738,#53739,#53740,
#53741,#53742),.UNSPECIFIED.,.F.,.F.,(4,2,2,2,2,2,2,2,3,2,2,2,2,4),(-1.31557498404543,
-1.19646405360563,-0.998703900016074,-0.80094374642652,-0.603183592836967,
-0.405423439247414,-0.202711719623707,-0.101355859811853,0.,0.101355859811854,
0.202711719623707,0.405423439247413,0.603183592836967,0.756268946977335),
 .UNSPECIFIED.);
#976=B_SPLINE_CURVE_WITH_KNOTS('',3,(#53743,#53744,#53745,#53746,#53747,
#53748,#53749,#53750,#53751,#53752,#53753,#53754,#53755,#53756,#53757,#53758,
#53759,#53760,#53761,#53762,#53763,#53764,#53765,#53766,#53767,#53768,#53769,
#53770,#53771,#53772,#53773,#53774,#53775,#53776,#53777,#53778,#53779,#53780,
#53781,#53782,#53783,#53784,#53785,#53786,#53787,#53788,#53789,#53790,#53791,
#53792,#53793,#53794,#53795,#53796,#53797,#53798,#53799,#53800,#53801,#53802,
#53803,#53804,#53805,#53806,#53807,#53808,#53809,#53810,#53811,#53812),
 .UNSPECIFIED.,.F.,.F.,(4,3,3,3,3,3,3,3,3,3,3,3,3,3,3,3,3,3,3,3,3,3,3,4),
(0.00228250782718277,0.00259180593297786,0.00274645498587541,0.00282377951232418,
0.00290110403877294,0.00321040214456803,0.00351970025036311,0.0038289983561582,
0.00413829646195329,0.00444759456774837,0.00452491909419713,0.0046022436206459,
0.00475689267354343,0.0050661907793385,0.00537548888513356,0.00568478699092863,
0.0059940850967237,0.0062772128484052,0.00630338320251876,0.00638070772896753,
0.00645803225541631,0.00661268130831385,0.00692197941410894,0.00723127751990404),
 .UNSPECIFIED.);
#977=B_SPLINE_CURVE_WITH_KNOTS('',3,(#53813,#53814,#53815,#53816,#53817,
#53818,#53819,#53820,#53821,#53822,#53823,#53824,#53825,#53826,#53827,#53828,
#53829,#53830,#53831,#53832,#53833),.UNSPECIFIED.,.F.,.F.,(4,2,2,2,2,3,
2,2,2,4),(2.44750603872918,2.60059139286912,2.79835154645867,3.00106326608238,
3.10241912589423,3.20377498570608,3.30513084551794,3.40648670532979,3.6091984249535,
3.78258560262431),.UNSPECIFIED.);
#978=B_SPLINE_CURVE_WITH_KNOTS('',3,(#53838,#53839,#53840,#53841,#53842,
#53843),.UNSPECIFIED.,.F.,.F.,(4,2,4),(-1.75663608064087,-1.67778100951734,
-1.61558523752689),.UNSPECIFIED.);
#979=B_SPLINE_CURVE_WITH_KNOTS('',3,(#53845,#53846,#53847,#53848,#53849,
#53850,#53851,#53852,#53853,#53854,#53855,#53856,#53857,#53858,#53859,#53860,
#53861,#53862,#53863,#53864,#53865,#53866,#53867,#53868,#53869,#53870,#53871,
#53872,#53873,#53874,#53875,#53876,#53877,#53878,#53879,#53880,#53881,#53882,
#53883,#53884,#53885,#53886,#53887,#53888,#53889,#53890,#53891,#53892,#53893,
#53894,#53895,#53896,#53897,#53898,#53899,#53900,#53901,#53902,#53903,#53904,
#53905,#53906,#53907,#53908,#53909,#53910,#53911,#53912,#53913,#53914,#53915,
#53916,#53917,#53918,#53919,#53920,#53921,#53922,#53923,#53924,#53925,#53926,
#53927,#53928,#53929,#53930,#53931,#53932,#53933,#53934,#53935,#53936,#53937,
#53938,#53939,#53940,#53941,#53942,#53943,#53944,#53945,#53946,#53947,#53948,
#53949,#53950),.UNSPECIFIED.,.F.,.F.,(4,3,3,3,3,3,3,3,3,3,3,3,3,3,3,3,3,
3,3,3,3,3,3,3,3,3,3,3,3,3,3,3,3,3,3,4),(0.0305709307873588,0.0306063950419885,
0.0306418592966182,0.0307023678095767,0.0307127878058775,0.0308370374836857,
0.0308546448243963,0.0309745186599934,0.0311143035117337,0.0311383588614337,
0.031350416372114,0.0313990237158669,0.0314220728984712,0.031639460489526,
0.0316879165996665,0.0317057869355086,0.0319209128177052,0.03197751646506,
0.0319895009725461,0.0320604294818055,0.0321313579910648,0.0322664035810511,
0.0322732150095836,0.0324971762357835,0.0325549976396122,0.0325569290466211,
0.0326983162209017,0.0326987860651398,0.0327695930842391,0.0327697145743992,
0.0328051206407264,0.0328051788290289,0.0328229109563437,0.0328317770200012,
0.0328362100518299,0.0328406430836586),.UNSPECIFIED.);
#980=B_SPLINE_CURVE_WITH_KNOTS('',3,(#53951,#53952,#53953,#53954,#53955,
#53956,#53957,#53958,#53959,#53960,#53961,#53962,#53963,#53964,#53965,#53966,
#53967,#53968,#53969,#53970,#53971,#53972,#53973,#53974,#53975,#53976,#53977,
#53978,#53979,#53980,#53981,#53982,#53983,#53984,#53985,#53986,#53987,#53988,
#53989,#53990,#53991,#53992,#53993,#53994,#53995,#53996,#53997,#53998,#53999,
#54000,#54001,#54002,#54003,#54004,#54005,#54006,#54007,#54008,#54009,#54010,
#54011,#54012,#54013,#54014,#54015,#54016,#54017,#54018,#54019,#54020,#54021,
#54022,#54023,#54024,#54025,#54026,#54027,#54028,#54029,#54030,#54031,#54032,
#54033,#54034,#54035),.UNSPECIFIED.,.F.,.F.,(4,3,3,3,3,3,3,3,3,3,3,3,3,
3,3,3,3,3,3,3,3,3,3,3,3,3,3,3,4),(2.5816516038653E-11,3.54600608128747E-5,
3.56641847997305E-5,7.10560249003594E-5,0.000142556163497147,0.000285313478397844,
0.000286667929283135,0.000508969327732133,0.000570626956795688,0.000578229350350693,
0.000800126093089386,0.000855940435193532,0.000871807784634396,0.0010892321962361,
0.00114125391359138,0.00116414093555289,0.00137785778404045,0.00142656739198922,
0.00145179194908138,0.00146223157678895,0.00149789576158867,0.00156922413118814,
0.00171188087038706,0.00173474788861624,0.00187461379195942,0.00199719434878491,
0.00201280376719228,0.00214889827835077,0.00228250782718276),
 .UNSPECIFIED.);
#981=B_SPLINE_CURVE_WITH_KNOTS('',3,(#54042,#54043,#54044,#54045,#54046,
#54047,#54048,#54049,#54050,#54051,#54052,#54053,#54054,#54055,#54056,#54057,
#54058,#54059,#54060,#54061,#54062,#54063),.UNSPECIFIED.,.F.,.F.,(4,2,2,
2,2,2,2,2,2,2,4),(0.427651316099875,0.508717953234535,0.577778895492431,
0.646839837750328,0.694519804488737,0.742199771227145,0.837559704703962,
0.981848513434963,1.12613732216597,1.41471493962797,1.47691071161843),
 .UNSPECIFIED.);
#982=B_SPLINE_CURVE_WITH_KNOTS('',3,(#54066,#54067,#54068,#54069,#54070,
#54071),.UNSPECIFIED.,.F.,.F.,(4,2,4),(0.0698399460344426,0.254358976617267,
0.427651316099875),.UNSPECIFIED.);
#983=B_SPLINE_CURVE_WITH_KNOTS('',3,(#54072,#54073,#54074,#54075,#54076,
#54077,#54078,#54079,#54080,#54081,#54082,#54083,#54084,#54085,#54086,#54087,
#54088,#54089,#54090,#54091,#54092,#54093,#54094,#54095,#54096,#54097,#54098,
#54099,#54100,#54101,#54102,#54103,#54104,#54105,#54106,#54107,#54108,#54109,
#54110,#54111,#54112,#54113,#54114,#54115,#54116,#54117,#54118,#54119,#54120,
#54121,#54122,#54123,#54124,#54125,#54126,#54127,#54128,#54129,#54130,#54131,
#54132,#54133,#54134,#54135,#54136,#54137,#54138,#54139,#54140,#54141,#54142,
#54143,#54144,#54145,#54146,#54147,#54148,#54149,#54150,#54151,#54152,#54153,
#54154,#54155,#54156,#54157,#54158,#54159,#54160,#54161,#54162,#54163,#54164,
#54165,#54166,#54167,#54168,#54169,#54170,#54171,#54172,#54173,#54174,#54175,
#54176,#54177,#54178,#54179,#54180,#54181,#54182,#54183,#54184,#54185,#54186,
#54187,#54188,#54189,#54190,#54191,#54192,#54193,#54194,#54195,#54196,#54197,
#54198,#54199,#54200,#54201,#54202,#54203,#54204,#54205,#54206,#54207,#54208,
#54209,#54210,#54211,#54212,#54213,#54214,#54215,#54216,#54217,#54218,#54219,
#54220,#54221,#54222,#54223,#54224,#54225,#54226,#54227,#54228,#54229,#54230,
#54231,#54232,#54233,#54234,#54235,#54236,#54237,#54238,#54239,#54240,#54241,
#54242,#54243,#54244,#54245,#54246,#54247,#54248,#54249,#54250,#54251,#54252,
#54253,#54254,#54255,#54256,#54257,#54258,#54259,#54260,#54261,#54262,#54263,
#54264,#54265,#54266,#54267,#54268,#54269,#54270,#54271,#54272,#54273,#54274,
#54275,#54276,#54277,#54278,#54279,#54280,#54281,#54282,#54283,#54284,#54285,
#54286,#54287,#54288,#54289,#54290,#54291,#54292,#54293,#54294,#54295,#54296,
#54297,#54298,#54299,#54300,#54301,#54302,#54303,#54304,#54305,#54306,#54307,
#54308,#54309,#54310,#54311,#54312,#54313,#54314,#54315,#54316,#54317,#54318,
#54319,#54320,#54321,#54322,#54323,#54324,#54325,#54326,#54327,#54328,#54329,
#54330,#54331,#54332,#54333,#54334,#54335,#54336,#54337,#54338,#54339,#54340,
#54341,#54342,#54343,#54344,#54345,#54346,#54347,#54348,#54349,#54350,#54351,
#54352,#54353,#54354,#54355,#54356,#54357,#54358,#54359,#54360,#54361,#54362,
#54363,#54364,#54365,#54366,#54367,#54368,#54369,#54370,#54371,#54372,#54373,
#54374,#54375,#54376,#54377,#54378,#54379,#54380,#54381,#54382,#54383,#54384,
#54385,#54386,#54387,#54388,#54389,#54390,#54391,#54392,#54393,#54394,#54395,
#54396,#54397,#54398,#54399,#54400,#54401,#54402,#54403,#54404,#54405,#54406,
#54407,#54408,#54409,#54410,#54411,#54412,#54413,#54414,#54415,#54416,#54417,
#54418,#54419,#54420,#54421,#54422,#54423,#54424,#54425,#54426,#54427,#54428,
#54429,#54430,#54431,#54432,#54433,#54434,#54435,#54436,#54437,#54438,#54439,
#54440,#54441,#54442,#54443,#54444,#54445,#54446,#54447,#54448,#54449,#54450,
#54451,#54452,#54453,#54454,#54455,#54456,#54457,#54458,#54459,#54460,#54461,
#54462,#54463,#54464,#54465,#54466,#54467,#54468,#54469,#54470,#54471,#54472,
#54473,#54474,#54475,#54476,#54477,#54478,#54479,#54480,#54481,#54482,#54483,
#54484,#54485,#54486,#54487,#54488,#54489,#54490,#54491,#54492,#54493,#54494,
#54495,#54496,#54497,#54498),.UNSPECIFIED.,.F.,.F.,(4,3,3,3,3,3,3,3,3,3,
3,3,3,3,3,3,3,3,3,3,3,3,3,3,3,3,3,3,3,3,3,3,3,3,3,3,3,3,3,3,3,3,3,3,3,3,
3,3,3,3,3,3,3,3,3,3,3,3,3,3,3,3,3,3,3,3,3,3,3,3,3,3,3,3,3,3,3,3,3,3,3,3,
3,3,3,3,3,3,3,3,3,3,3,3,3,3,3,3,3,3,3,3,3,3,3,3,3,3,3,3,3,3,3,3,3,3,3,3,
3,3,3,3,3,3,3,3,3,3,3,3,3,3,3,3,3,3,3,3,3,3,3,3,4),(0.0206286231325014,
0.0206447094230554,0.0206839579200574,0.0207013849168472,0.0207232064170594,
0.0210060975778275,0.0210371943930756,0.0213114656590281,0.0213511823690917,
0.0216174688377158,0.0216651703451078,0.0216940599097884,0.0217436673391119,
0.021770732718017,0.0218221643331159,0.0219243902561196,0.021979158321124,
0.0222328665245741,0.0222931462971402,0.0225427671520463,0.0226071342731563,
0.0227641282611644,0.0228426252551685,0.0228539704164397,0.0228818737521705,
0.0229211222491725,0.0229319636339267,0.0230100441327226,0.0231664468356769,
0.0232351102251887,0.0234801808337334,0.0235490982012049,0.0237950373987436,
0.0238630861772211,0.0241109051815931,0.0241770741532372,0.024427705018772,
0.0244910621292534,0.0245695591232575,0.0245864047557396,0.0246480561172615,
0.0247452759130522,0.0248050501052696,0.0251190380812858,0.0253821615172229,
0.025433026057302,0.0257470140333182,0.0260209637001603,0.0263749899853506,
0.0266613596160773,0.0269820800759253,0.027002965937383,0.0271425602282344,
0.0271599599253911,0.0272228290434084,0.0272384569193951,0.0273031166709421,
0.0273169539133992,0.0276309418894154,0.0279454744899221,0.0282589178414478,
0.0285877913758882,0.0288868937934803,0.0292299702284112,0.0295148697455127,
0.02987192891183,0.0301428456975452,0.0305135974218362,0.0307708216495776,
0.0308343041148486,0.0309278156375857,0.0309946223687894,0.0310063126315898,
0.0310848096255938,0.0311548982142129,0.03139879760161,0.0317950926599704,
0.0320267735536425,0.0324336477724454,0.032654749505675,0.0330705169098406,
0.0332827254577074,0.0337056378092121,0.0338641371581584,0.0339107014097399,
0.033943344025685,0.0339891984037439,0.034022518463526,0.0340676953977479,
0.034224689385756,0.0343388083882488,0.0345386773617722,0.0349693595359445,
0.0351666533138045,0.0354806412898207,0.0355972043577933,0.0357537404841202,
0.0357946292658369,0.0358319417780599,0.0358731262598409,0.0359101028303693,
0.035951623253845,0.0361086172418531,0.0362222760339768,0.0364226052178693,
0.0367365931938856,0.0368444295298401,0.0370505811699018,0.0373645691459181,
0.0374430661399221,0.0374637324729354,0.0375215631339262,0.0375409504156616,
0.0376181302752573,0.0376785571219343,0.0377723740804822,0.0379925450979505,
0.0380804310369398,0.0383065330739667,0.0386205210499829,0.0386948655346232,
0.0389345090259991,0.0390012628917026,0.0390130060200032,0.0390522545170052,
0.0390777695532355,0.0390915030140073,0.0391542118436117,0.0392484970020154,
0.0393068924677751,0.0395624849780316,0.0396114511725609,0.0398764729540479,
0.039914949116982,0.040033466942056,0.0401708366815631,0.0401904609300641,
0.0402173631023923,0.0403685816462537,0.0404444323885405,0.040482420371629,
0.04050444890608,0.040520443503722),.UNSPECIFIED.);
#984=B_SPLINE_CURVE_WITH_KNOTS('',3,(#54568,#54569,#54570,#54571,#54572,
#54573,#54574,#54575,#54576,#54577,#54578,#54579,#54580,#54581,#54582,#54583,
#54584,#54585,#54586,#54587,#54588,#54589,#54590,#54591,#54592,#54593,#54594,
#54595,#54596,#54597,#54598,#54599,#54600,#54601,#54602,#54603,#54604,#54605,
#54606,#54607,#54608,#54609,#54610,#54611,#54612,#54613,#54614,#54615,#54616,
#54617,#54618,#54619,#54620,#54621,#54622,#54623,#54624,#54625,#54626,#54627,
#54628,#54629,#54630,#54631),.UNSPECIFIED.,.F.,.F.,(4,3,3,3,3,3,3,3,3,3,
3,3,3,3,3,3,3,3,3,3,3,4),(0.,6.36402803474462E-5,0.000127280560694892,0.000159100700868616,
0.00017501077095548,0.000190920841042344,0.000254561121389809,0.000318201401737275,
0.000334111471824142,0.000350021541911008,0.000381841682084741,0.000445481962432199,
0.000477302102605929,0.000493212172692793,0.000509122242779658,0.000572762523127108,
0.000636402803474558,0.000668222943648282,0.00068413301373514,0.000700043083821997,
0.000763683364169407,0.000782835047457224),.UNSPECIFIED.);
#985=B_SPLINE_CURVE_WITH_KNOTS('',3,(#54633,#54634,#54635,#54636,#54637,
#54638,#54639,#54640,#54641,#54642,#54643,#54644,#54645,#54646,#54647),
 .UNSPECIFIED.,.F.,.F.,(4,2,2,1,2,2,1,1,4),(0.000782835047457224,0.000827323644516816,
0.000843233714603663,0.000859143784690511,0.000890963924864205,0.000954604205211594,
0.000986424345385289,0.00100233441547213,0.00101824448555897),
 .UNSPECIFIED.);
#986=B_SPLINE_CURVE_WITH_KNOTS('',3,(#54648,#54649,#54650,#54651,#54652,
#54653,#54654,#54655,#54656,#54657,#54658,#54659,#54660,#54661,#54662,#54663,
#54664,#54665,#54666,#54667,#54668,#54669,#54670,#54671,#54672,#54673,#54674,
#54675,#54676,#54677,#54678,#54679,#54680,#54681,#54682,#54683,#54684,#54685,
#54686,#54687),.UNSPECIFIED.,.F.,.F.,(4,3,3,3,3,3,3,3,3,3,3,3,3,4),(3.25260651745651E-19,
3.42965330670762E-5,6.88862345657144E-5,0.000138341881978896,0.000207969419140507,
0.000225387427278471,0.000242804328229345,0.000277624644722789,0.000347060433943642,
0.000381766477338011,0.000399119499035193,0.000416472520732376,0.000485836343494754,
0.000555296694309835),.UNSPECIFIED.);
#987=B_SPLINE_CURVE_WITH_KNOTS('',3,(#54698,#54699,#54700,#54701,#54702,
#54703,#54704,#54705,#54706,#54707,#54708,#54709,#54710,#54711,#54712,#54713,
#54714,#54715,#54716,#54717,#54718,#54719,#54720,#54721,#54722,#54723,#54724,
#54725,#54726,#54727,#54728,#54729,#54730,#54731,#54732,#54733,#54734,#54735,
#54736,#54737,#54738,#54739,#54740,#54741,#54742,#54743,#54744,#54745,#54746,
#54747,#54748,#54749,#54750,#54751,#54752,#54753,#54754,#54755,#54756,#54757,
#54758,#54759,#54760,#54761,#54762,#54763,#54764,#54765,#54766,#54767,#54768,
#54769,#54770,#54771,#54772,#54773,#54774,#54775,#54776,#54777,#54778,#54779,
#54780,#54781,#54782,#54783,#54784,#54785,#54786,#54787,#54788,#54789,#54790,
#54791,#54792,#54793,#54794,#54795,#54796,#54797,#54798,#54799,#54800,#54801,
#54802,#54803,#54804,#54805,#54806,#54807,#54808,#54809,#54810,#54811,#54812,
#54813,#54814,#54815,#54816,#54817,#54818,#54819,#54820,#54821,#54822,#54823,
#54824,#54825,#54826,#54827,#54828,#54829,#54830,#54831,#54832,#54833),
 .UNSPECIFIED.,.F.,.F.,(4,3,3,3,3,3,3,3,3,3,3,3,3,3,3,3,3,3,3,3,3,3,3,3,
3,3,3,3,3,3,3,3,3,3,3,3,3,3,3,3,3,3,3,3,3,4),(0.,4.91689726004813E-5,5.05531472505571E-5,
7.39482684633374E-5,7.58297208758408E-5,8.63848253908088E-5,9.88503858357188E-5,
0.000101106294501124,0.00014892407146761,0.00015165944175169,0.000199318832959595,
0.000202212589002255,0.000227489162627535,0.000249994600458649,0.000252765736252814,
0.000275444625287608,0.000300981075513535,0.000303318883503374,0.000352201416378833,
0.000353872030753934,0.000403559031113317,0.000404425178004494,0.000429260234366245,
0.000429701751629774,0.000454948636729993,0.000454978325255055,0.000505531472505623,
0.000506209072757505,0.000556084619756192,0.000557247649660384,0.000581361193381469,
0.000582659083595442,0.000593999480194102,0.000606637767006736,0.000607987133405275,
0.000657190914257281,0.000658445872483203,0.000707744061507826,0.00070863765270964,
0.00075829720875837,0.000758539102560875,0.000770935495570998,0.000770971495620867,
0.000783408714808202,0.000783573782383626,0.00080811238697951),
 .UNSPECIFIED.);
#988=B_SPLINE_CURVE_WITH_KNOTS('',3,(#54835,#54836,#54837,#54838,#54839,
#54840,#54841,#54842,#54843,#54844,#54845,#54846,#54847,#54848,#54849,#54850,
#54851,#54852,#54853,#54854,#54855,#54856,#54857,#54858,#54859,#54860,#54861,
#54862,#54863,#54864,#54865,#54866,#54867,#54868,#54869,#54870,#54871,#54872,
#54873,#54874,#54875,#54876,#54877,#54878,#54879,#54880,#54881,#54882,#54883,
#54884,#54885,#54886,#54887,#54888,#54889,#54890,#54891,#54892,#54893,#54894,
#54895,#54896,#54897,#54898,#54899,#54900,#54901,#54902,#54903,#54904,#54905,
#54906,#54907,#54908,#54909,#54910,#54911,#54912,#54913,#54914,#54915,#54916,
#54917,#54918,#54919,#54920,#54921,#54922,#54923,#54924,#54925,#54926,#54927,
#54928,#54929,#54930,#54931,#54932,#54933,#54934,#54935,#54936,#54937,#54938,
#54939,#54940,#54941,#54942,#54943,#54944,#54945,#54946,#54947,#54948,#54949,
#54950,#54951,#54952,#54953,#54954,#54955,#54956,#54957,#54958,#54959,#54960,
#54961,#54962,#54963,#54964),.UNSPECIFIED.,.F.,.F.,(4,3,3,3,3,3,3,3,3,3,
3,3,3,3,3,3,3,3,3,3,3,3,3,3,3,3,3,3,3,3,3,3,3,3,3,3,3,3,3,3,3,3,3,4),(0.00080811238697951,
0.000808302945491443,0.000808850356008893,0.000858169371998666,0.000859403503259436,
0.00090813769617751,0.000909956650509979,0.000922594937322613,0.00093315937462551,
0.000935233224135246,0.00095824545751998,0.00096050979776051,0.00100870006033539,
0.00101106294501103,0.00105948647079065,0.00106161609226155,0.00108689266588681,
0.00111055157423082,0.00111216923951207,0.00116181788716099,0.0011627223867626,
0.00121318172198154,0.00121327553401313,0.00126382868126365,0.00126454753268235,
0.00127646696807629,0.00127737780427383,0.00128910525488892,0.00129020045697118,
0.00131438182851419,0.00131580628731212,0.00136493497576474,0.00136682939005471,
0.00141548812301528,0.00141753931363807,0.00144076469664055,0.00144275336852841,
0.00146604127026582,0.00146787510376584,0.00151659441751637,0.00151798775480161,
0.00156714756476691,0.00156793293030094,0.00161770071201745),
 .UNSPECIFIED.);
#989=B_SPLINE_CURVE_WITH_KNOTS('',3,(#54988,#54989,#54990,#54991,#54992,
#54993,#54994,#54995,#54996,#54997),.UNSPECIFIED.,.F.,.F.,(4,2,2,2,4),(-0.00550601116947268,
0.,0.0481725175638029,0.0759608671644843,0.10231697822769),
 .UNSPECIFIED.);
#990=B_SPLINE_CURVE_WITH_KNOTS('',3,(#55034,#55035,#55036,#55037,#55038,
#55039,#55040,#55041,#55042,#55043,#55044,#55045,#55046,#55047,#55048,#55049,
#55050,#55051,#55052,#55053,#55054,#55055,#55056,#55057,#55058,#55059,#55060,
#55061,#55062,#55063,#55064,#55065,#55066,#55067,#55068,#55069,#55070,#55071,
#55072,#55073,#55074,#55075,#55076,#55077,#55078,#55079,#55080,#55081,#55082,
#55083,#55084,#55085,#55086,#55087,#55088,#55089,#55090,#55091,#55092,#55093,
#55094,#55095,#55096,#55097,#55098,#55099,#55100),.UNSPECIFIED.,.F.,.F.,
(4,3,3,3,3,3,3,3,3,3,3,3,3,3,3,3,3,3,3,3,3,3,4),(-0.0010038592303248,-0.000996016580088018,
-0.000988173929851109,-0.000972488629377284,-0.000941118028429635,-0.000909747427481985,
-0.000878376826534336,-0.0007756051487124,-0.000752894422743731,-0.000656768417933472,
-0.000627412018953126,-0.000596041418005469,-0.000564670817057813,-0.0005019296151625,
-0.000413395135354653,-0.000376447211371868,-0.000313706009476555,-0.000282335408528902,
-0.00025096480758125,-0.000169956252849148,-0.000125482403790632,-6.2741201895316E-5,
0.),.UNSPECIFIED.);
#991=B_SPLINE_CURVE_WITH_KNOTS('',3,(#55108,#55109,#55110,#55111,#55112,
#55113,#55114,#55115,#55116,#55117),.UNSPECIFIED.,.F.,.F.,(4,2,2,2,4),(2.3288001587927E-6,
0.0253758099388679,0.0507136033495846,0.103872134093849,0.104445029963715),
 .UNSPECIFIED.);
#992=B_SPLINE_CURVE_WITH_KNOTS('',3,(#55244,#55245,#55246,#55247,#55248,
#55249,#55250,#55251,#55252,#55253,#55254,#55255,#55256,#55257,#55258,#55259,
#55260,#55261,#55262,#55263,#55264,#55265,#55266,#55267,#55268,#55269,#55270,
#55271,#55272,#55273,#55274,#55275,#55276,#55277,#55278,#55279,#55280,#55281,
#55282,#55283,#55284,#55285,#55286,#55287,#55288,#55289,#55290,#55291,#55292,
#55293,#55294,#55295,#55296,#55297,#55298,#55299,#55300,#55301,#55302,#55303,
#55304,#55305,#55306,#55307,#55308,#55309,#55310,#55311,#55312,#55313,#55314,
#55315,#55316,#55317,#55318,#55319,#55320,#55321,#55322,#55323,#55324,#55325,
#55326,#55327,#55328),.UNSPECIFIED.,.F.,.F.,(4,3,3,3,3,3,3,3,3,3,3,3,3,
3,3,3,3,3,3,3,3,3,3,3,3,3,3,3,4),(0.,0.000132953866864794,0.000143131415743608,
0.000214697123615411,0.000250479977551313,0.00026681859857174,0.000286262831487215,
0.00030052042883516,0.000322045685423116,0.000334541694191434,0.000357828539359018,
0.000403373858123355,0.000429394247230825,0.000543906469566681,0.00057252566297444,
0.000615590207484267,0.00064409137084625,0.000651788086821203,0.000679874224782152,
0.000688237624566197,0.000715657078718053,0.00083666270204627,0.000858788494461667,
0.000989235649453088,0.00100191991020528,0.00103770276414118,0.00106699082305431,
0.00107348561807708,0.00114505132594889),.UNSPECIFIED.);
#993=B_SPLINE_CURVE_WITH_KNOTS('',3,(#55341,#55342,#55343,#55344),
 .UNSPECIFIED.,.F.,.F.,(4,4),(0.00036767516211002,0.0122424340459221),
 .UNSPECIFIED.);
#994=B_SPLINE_CURVE_WITH_KNOTS('',3,(#55345,#55346,#55347,#55348,#55349,
#55350,#55351,#55352),.UNSPECIFIED.,.F.,.F.,(4,2,2,4),(-0.0849227079013314,
-0.0799038204840182,-0.0443510460373534,-1.00047370417821E-6),
 .UNSPECIFIED.);
#995=B_SPLINE_CURVE_WITH_KNOTS('',3,(#55633,#55634,#55635,#55636),
 .UNSPECIFIED.,.F.,.F.,(4,4),(0.,0.0113332794370003),.UNSPECIFIED.);
#996=B_SPLINE_CURVE_WITH_KNOTS('',3,(#55777,#55778,#55779,#55780,#55781,
#55782,#55783,#55784,#55785,#55786,#55787,#55788,#55789,#55790,#55791,#55792,
#55793,#55794,#55795,#55796,#55797,#55798,#55799,#55800,#55801,#55802,#55803,
#55804,#55805,#55806,#55807,#55808,#55809,#55810,#55811,#55812,#55813,#55814,
#55815,#55816,#55817,#55818,#55819,#55820,#55821,#55822,#55823,#55824,#55825,
#55826,#55827,#55828,#55829,#55830,#55831,#55832,#55833,#55834,#55835,#55836,
#55837,#55838,#55839,#55840,#55841,#55842,#55843),.UNSPECIFIED.,.F.,.F.,
(4,3,3,3,3,3,3,3,3,3,3,3,3,3,3,3,3,3,3,3,3,3,4),(0.,5.50030531657853E-5,
0.000110006106331571,0.000165009159497356,0.000178759922788797,0.000192510686080239,
0.000220012212663132,0.000275015265828909,0.000330018318994686,0.00035751984557757,
0.000385021372160454,0.000440024425326228,0.000495027478492002,0.000508778241783447,
0.000522529005074892,0.000550030531657776,0.000605033584823541,0.000660036637989305,
0.000687538164572187,0.000715039691155069,0.000770042744320831,0.000825045797486593,
0.000880048850652355),.UNSPECIFIED.);
#997=B_SPLINE_CURVE_WITH_KNOTS('',3,(#55844,#55845,#55846,#55847,#55848,
#55849,#55850,#55851,#55852,#55853,#55854,#55855,#55856,#55857,#55858,#55859,
#55860,#55861,#55862,#55863,#55864,#55865,#55866,#55867,#55868,#55869,#55870,
#55871,#55872,#55873,#55874,#55875,#55876,#55877,#55878,#55879,#55880,#55881,
#55882),.UNSPECIFIED.,.F.,.F.,(4,1,1,2,2,1,2,1,2,2,2,1,1,2,2,2,1,1,2,1,
2,2,1,1,4),(5.96075724321896E-15,0.000108435279304831,0.000216870558603701,
0.00032530583790257,0.00035241465772729,0.000379523477552009,0.000433741117201448,
0.000542176396500325,0.000650611675799202,0.000677720495623919,0.000704829315448636,
0.000759046955098071,0.000867482234396948,0.000975917513695825,0.00103013515334526,
0.00105724397316998,0.0010843527929947,0.00119278807229356,0.00130122335159243,
0.00135544099124186,0.00138254981106657,0.00140965863089129,0.00151809391019014,
0.00162652918948899,0.00173496446878785),.UNSPECIFIED.);
#998=B_SPLINE_CURVE_WITH_KNOTS('',3,(#56242,#56243,#56244,#56245),
 .UNSPECIFIED.,.F.,.F.,(4,4),(1.78796901209599,1.79013675073573),
 .UNSPECIFIED.);
#999=B_SPLINE_CURVE_WITH_KNOTS('',3,(#56352,#56353,#56354,#56355,#56356,
#56357,#56358,#56359,#56360,#56361,#56362,#56363,#56364,#56365,#56366,#56367,
#56368,#56369,#56370,#56371,#56372,#56373,#56374,#56375,#56376,#56377,#56378,
#56379,#56380,#56381,#56382,#56383,#56384,#56385,#56386,#56387,#56388,#56389,
#56390,#56391,#56392,#56393,#56394),.UNSPECIFIED.,.F.,.F.,(4,3,3,3,3,3,
3,3,3,3,3,3,3,3,4),(-0.00218249118872392,-0.00216544047631201,-0.00214838976390011,
-0.0021142883390763,-0.00204608548942867,-0.00190967979013342,-0.00163686839154293,
-0.00136405699295245,-0.00109124559436196,-0.000818434195771467,-0.000545622797180978,
-0.000409217097885734,-0.000272811398590489,-0.000136405699295245,0.),
 .UNSPECIFIED.);
#1000=B_SPLINE_CURVE_WITH_KNOTS('',3,(#56398,#56399,#56400,#56401,#56402,
#56403),.UNSPECIFIED.,.F.,.F.,(4,2,4),(-0.0212734387247141,-0.0106371499207884,
-1.22408019587832E-6),.UNSPECIFIED.);
#1001=B_SPLINE_CURVE_WITH_KNOTS('',3,(#56406,#56407,#56408,#56409,#56410,
#56411,#56412,#56413,#56414,#56415,#56416,#56417,#56418,#56419,#56420,#56421,
#56422,#56423,#56424,#56425,#56426,#56427,#56428,#56429,#56430,#56431,#56432,
#56433),.UNSPECIFIED.,.F.,.F.,(4,3,3,3,3,3,3,3,3,4),(-0.00112201278880437,
-0.00110806877345402,-0.00109412475810366,-0.00106623672740295,-0.00101046066600152,
-0.000924145508874287,-0.000898908543198666,-0.00084313248179724,-0.000787356420395815,
-0.000675804297592954),.UNSPECIFIED.);
#1002=B_SPLINE_CURVE_WITH_KNOTS('',3,(#56434,#56435,#56436,#56437,#56438,
#56439,#56440,#56441),.UNSPECIFIED.,.F.,.F.,(4,2,2,4),(-0.0127135782228372,
0.,0.0940564686398219,0.200639665029003),.UNSPECIFIED.);
#1003=B_SPLINE_CURVE_WITH_KNOTS('',3,(#56473,#56474,#56475,#56476,#56477,
#56478,#56479,#56480,#56481,#56482,#56483,#56484,#56485,#56486,#56487,#56488,
#56489,#56490,#56491,#56492,#56493,#56494,#56495,#56496,#56497,#56498,#56499,
#56500,#56501,#56502,#56503,#56504,#56505,#56506,#56507,#56508,#56509,#56510,
#56511,#56512,#56513,#56514,#56515),.UNSPECIFIED.,.F.,.F.,(4,3,3,3,3,3,
3,3,3,3,3,3,3,3,4),(0.,0.00013646494075281,0.000272940213284047,0.000409423605142272,
0.000545889876308567,0.000818834814462857,0.00109177975261715,0.00136472469077144,
0.00163777665242055,0.00191061456708002,0.00204708703615716,0.00211531911473619,
0.00214944040496523,0.00216650044659966,0.0021835595052343),
 .UNSPECIFIED.);
#1004=B_SPLINE_CURVE_WITH_KNOTS('',3,(#56516,#56517,#56518,#56519,#56520,
#56521,#56522,#56523,#56524,#56525,#56526,#56527,#56528,#56529,#56530,#56531,
#56532,#56533,#56534,#56535,#56536,#56537,#56538,#56539,#56540,#56541,#56542,
#56543,#56544,#56545,#56546,#56547,#56548,#56549,#56550,#56551,#56552,#56553,
#56554,#56555,#56556,#56557,#56558),.UNSPECIFIED.,.F.,.F.,(4,3,3,3,3,3,
3,3,3,3,3,3,3,3,4),(-0.00218249118872365,-0.00216544047631174,-0.00214838976389984,
-0.00211428833907603,-0.00204608548942841,-0.00190967979013318,-0.00163686839154273,
-0.00136405699295227,-0.00109124559436182,-0.000818434195771367,-0.000545622797180915,
-0.000409217097885686,-0.000272811398590457,-0.000136405699295229,0.),
 .UNSPECIFIED.);
#1005=B_SPLINE_CURVE_WITH_KNOTS('',3,(#56559,#56560,#56561,#56562,#56563,
#56564,#56565,#56566,#56567,#56568,#56569,#56570,#56571,#56572,#56573,#56574,
#56575,#56576,#56577,#56578,#56579,#56580,#56581,#56582,#56583,#56584,#56585,
#56586,#56587,#56588,#56589,#56590,#56591,#56592,#56593,#56594,#56595,#56596,
#56597,#56598,#56599,#56600,#56601),.UNSPECIFIED.,.F.,.F.,(4,3,3,3,3,3,
3,3,3,3,3,3,3,3,4),(0.,0.000136464940752808,0.000272940213284044,0.000409423605142217,
0.000545889876308567,0.000818834814462855,0.00109177975261714,0.00136472469077143,
0.00163766962892572,0.00191061456708001,0.00204708703615715,0.00211531911473613,
0.00214944040496524,0.00216650044659965,0.0021835595052343),
 .UNSPECIFIED.);
#1006=B_SPLINE_CURVE_WITH_KNOTS('',3,(#56686,#56687,#56688,#56689,#56690,
#56691,#56692,#56693,#56694,#56695,#56696,#56697,#56698,#56699,#56700,#56701,
#56702,#56703,#56704,#56705,#56706,#56707,#56708,#56709,#56710,#56711,#56712,
#56713,#56714,#56715,#56716,#56717,#56718,#56719,#56720,#56721,#56722,#56723,
#56724,#56725,#56726,#56727,#56728,#56729,#56730,#56731,#56732,#56733,#56734,
#56735,#56736,#56737,#56738,#56739,#56740,#56741,#56742,#56743,#56744,#56745,
#56746,#56747,#56748,#56749,#56750,#56751,#56752,#56753,#56754,#56755,#56756,
#56757,#56758,#56759,#56760,#56761,#56762,#56763,#56764,#56765,#56766,#56767,
#56768,#56769,#56770,#56771,#56772,#56773,#56774,#56775,#56776,#56777,#56778,
#56779,#56780,#56781,#56782,#56783,#56784,#56785,#56786,#56787,#56788,#56789,
#56790,#56791),.UNSPECIFIED.,.F.,.F.,(4,3,3,3,3,3,3,3,3,3,3,3,3,3,3,3,3,
3,3,3,3,3,3,3,3,3,3,3,3,3,3,3,3,3,3,4),(0.0305709307873591,0.0306063950419888,
0.0306418592966185,0.030702367809577,0.0307127878058778,0.030837037483686,
0.0308546448243965,0.0309745186599938,0.0311143035117341,0.031138358861434,
0.0313504163721782,0.0313990237158671,0.0314220728984714,0.0316394604894248,
0.0316879165996668,0.0317057869355089,0.0319209128176095,0.0319775164650602,
0.0319895009725463,0.0320604294818057,0.032131357991065,0.0322664035810513,
0.0322732150095838,0.0324971762357433,0.0325549976396124,0.0325569290466212,
0.0326983162209018,0.03269878606514,0.0327695930842393,0.0327697145743993,
0.0328051206407265,0.032805178829029,0.0328229109563438,0.0328317770200012,
0.0328362100518299,0.0328406430836587),.UNSPECIFIED.);
#1007=B_SPLINE_CURVE_WITH_KNOTS('',3,(#56876,#56877,#56878,#56879,#56880,
#56881,#56882,#56883,#56884,#56885,#56886,#56887,#56888,#56889,#56890,#56891,
#56892,#56893,#56894,#56895,#56896,#56897,#56898,#56899,#56900,#56901,#56902,
#56903,#56904,#56905,#56906,#56907,#56908,#56909,#56910,#56911,#56912,#56913,
#56914,#56915,#56916,#56917,#56918,#56919,#56920,#56921,#56922,#56923,#56924,
#56925,#56926,#56927,#56928,#56929,#56930,#56931,#56932,#56933,#56934,#56935,
#56936,#56937,#56938,#56939,#56940,#56941,#56942,#56943,#56944,#56945,#56946,
#56947,#56948,#56949,#56950,#56951,#56952,#56953,#56954,#56955,#56956,#56957,
#56958,#56959,#56960),.UNSPECIFIED.,.F.,.F.,(4,3,3,3,3,3,3,3,3,3,3,3,3,
3,3,3,3,3,3,3,3,3,3,3,3,3,3,3,4),(3.95831162944544E-12,1.39313221873946E-7,
3.5460060852014E-5,7.10560249004281E-5,0.000142556163497197,0.000285313478397842,
0.000286667929283137,0.000508969327502391,0.000570626956795684,0.000578229350350691,
0.000800126092930885,0.000855940435193526,0.000871807784634421,0.00108923219617937,
0.00114125391359137,0.00116414093555289,0.00137785778304641,0.00142656739198921,
0.00145179194908681,0.00146223157678894,0.00149789576158867,0.00156922413118814,
0.00171188087038706,0.00173474788861616,0.00187461379195925,0.00199719434878491,
0.00201280376719234,0.00214889827835083,0.00228250782718277),
 .UNSPECIFIED.);
#1008=B_SPLINE_CURVE_WITH_KNOTS('',3,(#57050,#57051,#57052,#57053,#57054,
#57055,#57056,#57057,#57058,#57059,#57060,#57061,#57062,#57063,#57064,#57065,
#57066,#57067,#57068,#57069,#57070,#57071,#57072,#57073,#57074,#57075,#57076,
#57077,#57078,#57079,#57080,#57081,#57082,#57083,#57084,#57085,#57086,#57087,
#57088,#57089,#57090,#57091,#57092,#57093,#57094,#57095,#57096,#57097,#57098,
#57099,#57100,#57101,#57102,#57103,#57104,#57105,#57106,#57107,#57108,#57109,
#57110,#57111,#57112,#57113,#57114,#57115,#57116,#57117,#57118,#57119,#57120,
#57121,#57122,#57123,#57124,#57125,#57126,#57127,#57128,#57129,#57130,#57131,
#57132,#57133,#57134,#57135,#57136,#57137,#57138,#57139,#57140,#57141,#57142,
#57143,#57144,#57145,#57146,#57147,#57148,#57149,#57150,#57151,#57152,#57153,
#57154,#57155,#57156,#57157,#57158,#57159,#57160,#57161,#57162,#57163,#57164,
#57165,#57166,#57167,#57168,#57169,#57170,#57171,#57172,#57173,#57174,#57175,
#57176,#57177,#57178,#57179,#57180,#57181,#57182,#57183,#57184,#57185,#57186,
#57187,#57188,#57189,#57190,#57191,#57192,#57193,#57194,#57195,#57196,#57197,
#57198,#57199,#57200,#57201,#57202,#57203,#57204,#57205,#57206,#57207,#57208,
#57209,#57210,#57211,#57212,#57213,#57214,#57215,#57216,#57217,#57218,#57219,
#57220,#57221,#57222,#57223,#57224,#57225,#57226,#57227,#57228,#57229,#57230,
#57231,#57232,#57233,#57234,#57235,#57236,#57237,#57238,#57239,#57240,#57241,
#57242,#57243,#57244,#57245,#57246,#57247,#57248,#57249,#57250,#57251,#57252,
#57253,#57254,#57255,#57256,#57257,#57258,#57259,#57260,#57261,#57262,#57263,
#57264,#57265,#57266,#57267,#57268,#57269,#57270,#57271),.UNSPECIFIED.,
 .F.,.F.,(4,2,2,1,2,1,2,2,2,2,2,2,2,2,2,1,1,2,2,2,2,2,1,2,2,2,1,2,2,1,2,
1,2,2,2,1,2,2,2,2,2,2,2,2,2,1,1,2,2,2,1,2,2,2,2,2,2,2,1,2,2,2,2,2,2,2,2,
2,2,2,2,2,1,2,2,2,2,1,1,2,2,2,2,2,2,1,2,2,2,1,1,2,2,1,2,2,2,1,1,2,2,2,2,
1,2,2,2,2,2,2,1,1,2,2,2,2,2,2,2,2,1,2,2,4),(0.,0.000124188080077072,0.000186282120115608,
0.000248376160154143,0.000496752320308307,0.000993504640616636,0.00149025696092496,
0.00173863312107913,0.00180072716111768,0.00186282120115623,0.00198700928123333,
0.00248376160154172,0.0029805139218501,0.00347726624215848,0.00353936028219703,
0.00360145432223558,0.00372564240231269,0.0039740185624669,0.00447077088277532,
0.00496752320308375,0.00509171128316085,0.00515380532319941,0.00521589936323796,
0.00546427552339219,0.00596102784370064,0.00645778016400908,0.0067061563241633,
0.00683034440424042,0.00689243844427897,0.00695453248431752,0.00745128480462597,
0.00794803712493441,0.00844478944524286,0.00856897752531997,0.00869316560539708,
0.0089415417655513,0.00918991792570552,0.00925201196574408,0.00931410600578263,
0.00943829408585974,0.00993504640616816,0.0104317987264766,0.010928551046785,
0.0111769272069392,0.0112390212469778,0.0113011152870163,0.0114253033670935,
0.0119220556874019,0.0124188080077103,0.0126671841678646,0.0127913722479417,
0.0128534662879802,0.0129155603280188,0.0134123126483272,0.0139090649686356,
0.0141574411287899,0.014281629208867,0.0143437232489055,0.0144058172889441,
0.0149025696092525,0.015399321929561,0.0156476980897152,0.0157097921297537,
0.0157718861697923,0.0158960742498694,0.0163928265701779,0.0168895788904864,
0.0171379550506406,0.0172621431307177,0.0173242371707563,0.0173863312107948,
0.017510519290872,0.0176347073709491,0.0178830835311034,0.0183798358514119,
0.0188765881717205,0.0190007762517976,0.0190628702918362,0.0191249643318747,
0.019373340492029,0.0198700928123375,0.0203668451326459,0.0208635974529544,
0.0209877855330315,0.0210498795730701,0.0211119736131087,0.0213603497732629,
0.0218571020935714,0.0223538544138799,0.0226022305740341,0.0227264186541112,
0.0227885126941498,0.0228506067341884,0.0233473590544968,0.0238441113748053,
0.0243408636951138,0.0244650517751909,0.0245271458152295,0.0245892398552681,
0.0248376160154223,0.0253343683357308,0.0258311206560393,0.0260794968161935,
0.0261415908562321,0.0262036848962706,0.0263278729763477,0.0268246252966562,
0.0273213776169647,0.0278181299372732,0.0278802239773118,0.0279423180173503,
0.0280665060974275,0.0283148822575817,0.0288116345778902,0.0293083868981987,
0.029556763058353,0.0298051392185072,0.0303018915388157,0.0307986438591242,
0.0310470200192785,0.0311712080993556,0.0312333021393942,0.0312953961794328,
0.0317921484997413),.UNSPECIFIED.);
#1009=B_SPLINE_CURVE_WITH_KNOTS('',3,(#57274,#57275,#57276,#57277,#57278,
#57279,#57280,#57281,#57282,#57283,#57284,#57285,#57286,#57287,#57288,#57289,
#57290,#57291,#57292,#57293,#57294,#57295,#57296,#57297,#57298,#57299,#57300,
#57301,#57302,#57303,#57304,#57305,#57306,#57307,#57308,#57309,#57310,#57311,
#57312,#57313,#57314,#57315,#57316,#57317,#57318,#57319,#57320,#57321,#57322,
#57323,#57324,#57325,#57326,#57327,#57328,#57329,#57330,#57331,#57332,#57333,
#57334,#57335,#57336,#57337,#57338,#57339,#57340),.UNSPECIFIED.,.F.,.F.,
(4,3,3,3,3,3,3,3,3,3,3,3,3,3,3,3,3,3,3,3,3,3,4),(1.01984272302816E-10,7.14212642807727E-5,
0.00011606672308277,0.000198180758390202,0.00023213344616554,0.000261150126936228,
0.000290166807706916,0.000348200169248292,0.000436238575559047,0.000464266892331045,
0.000560937956114547,0.000580333615413797,0.000609350296184482,0.000638366976955167,
0.000696400338496545,0.000797480418061141,0.000812467061579307,0.000870500423120685,
0.000899517103891371,0.000914025444276714,0.000921279614469381,0.000924906699565713,
0.000928533784662045),.UNSPECIFIED.);
#1010=B_SPLINE_CURVE_WITH_KNOTS('',3,(#58842,#58843,#58844,#58845,#58846,
#58847,#58848,#58849),.UNSPECIFIED.,.F.,.F.,(4,2,2,4),(1.99674797794768E-6,
0.115795506675109,0.23027663807213,0.231396261216017),.UNSPECIFIED.);
#1011=B_SPLINE_CURVE_WITH_KNOTS('',3,(#58966,#58967,#58968,#58969,#58970,
#58971,#58972,#58973,#58974,#58975,#58976,#58977,#58978,#58979,#58980,#58981,
#58982,#58983,#58984,#58985,#58986,#58987,#58988,#58989,#58990,#58991),
 .UNSPECIFIED.,.F.,.F.,(4,1,2,1,1,2,2,2,2,2,1,1,1,1,1,2,4),(1.83170469685919E-10,
8.90982346471883E-5,0.000178196469294377,0.000222745586617969,0.000245020145279767,
0.000267294703941566,0.000356392938588793,0.000445491173236021,0.000534589407883249,
0.000556863966545041,0.000579138525206834,0.000623687642530402,0.000668236759853971,
0.000690511318515748,0.000701648597846644,0.000707217237512084,0.000712785877177525),
 .UNSPECIFIED.);
#1012=B_SPLINE_CURVE_WITH_KNOTS('',3,(#59043,#59044,#59045,#59046,#59047,
#59048),.UNSPECIFIED.,.F.,.F.,(4,2,4),(0.163612590061207,0.211914877806934,
0.237815857774527),.UNSPECIFIED.);
#1013=B_SPLINE_CURVE_WITH_KNOTS('',3,(#59204,#59205,#59206,#59207,#59208,
#59209,#59210,#59211,#59212,#59213,#59214,#59215,#59216,#59217,#59218,#59219,
#59220,#59221,#59222,#59223,#59224,#59225,#59226,#59227,#59228,#59229,#59230,
#59231,#59232,#59233,#59234,#59235,#59236,#59237,#59238,#59239,#59240,#59241,
#59242,#59243,#59244,#59245,#59246,#59247,#59248,#59249,#59250,#59251,#59252,
#59253,#59254,#59255,#59256,#59257,#59258,#59259,#59260,#59261,#59262,#59263,
#59264,#59265,#59266,#59267,#59268,#59269,#59270,#59271,#59272,#59273,#59274,
#59275,#59276,#59277,#59278,#59279,#59280,#59281,#59282),.UNSPECIFIED.,
 .F.,.F.,(4,3,3,3,3,3,3,3,3,3,3,3,3,3,3,3,3,3,3,3,3,3,3,3,3,3,4),(-0.00129891904736022,
-0.00129130819356754,-0.00128877124230316,-0.00127862343724565,-0.00125832782713064,
-0.00121773660690063,-0.00113655416644058,-0.00105537172598053,-0.00101478050575051,
-0.000994484895635494,-0.00097418928552048,-0.000893006845060438,-0.000811824404600395,
-0.000730641964140352,-0.000690050743910334,-0.000669755133795326,-0.000649459523680318,
-0.000568277083220278,-0.000487094642760238,-0.000405912202300198,-0.00036532098207018,
-0.000345025371955169,-0.000324729761840158,-0.000243547321380123,-0.000162364880920088,
-8.11824404600523E-5,-1.7130394325271E-17),.UNSPECIFIED.);
#1014=B_SPLINE_CURVE_WITH_KNOTS('',3,(#59283,#59284,#59285,#59286,#59287,
#59288,#59289,#59290),.UNSPECIFIED.,.F.,.F.,(4,2,2,4),(-0.00857562118451602,
4.87793563352587E-7,0.0211728314512976,0.051545416127519),.UNSPECIFIED.);
#1015=B_SPLINE_CURVE_WITH_KNOTS('',3,(#59291,#59292,#59293,#59294,#59295,
#59296,#59297,#59298),.UNSPECIFIED.,.F.,.F.,(4,2,2,4),(-0.147545167441897,
-0.135199000031876,-0.073467772649398,-1.78767173606405E-6),
 .UNSPECIFIED.);
#1016=B_SPLINE_CURVE_WITH_KNOTS('',3,(#59587,#59588,#59589,#59590,#59591,
#59592,#59593,#59594,#59595,#59596,#59597,#59598,#59599,#59600,#59601,#59602,
#59603,#59604,#59605,#59606,#59607,#59608,#59609,#59610,#59611,#59612,#59613,
#59614,#59615,#59616,#59617,#59618,#59619,#59620,#59621,#59622,#59623,#59624,
#59625,#59626,#59627,#59628,#59629),.UNSPECIFIED.,.F.,.F.,(4,3,3,3,3,3,
3,3,3,3,3,3,3,3,4),(0.,9.86527119726346E-5,0.000147453735011662,0.000250428443831339,
0.000294907470023324,0.000331770903776236,0.000368634337529148,0.000442361205034974,
0.0005160880725408,0.00055295150629371,0.000571383223170166,0.000575991152389278,
0.000578295116998834,0.000580599081608391,0.00058981494004661),
 .UNSPECIFIED.);
#1017=B_SPLINE_CURVE_WITH_KNOTS('',3,(#59630,#59631,#59632,#59633,#59634,
#59635,#59636,#59637,#59638,#59639,#59640,#59641,#59642,#59643,#59644,#59645,
#59646,#59647,#59648,#59649,#59650,#59651,#59652,#59653,#59654,#59655,#59656,
#59657,#59658,#59659,#59660),.UNSPECIFIED.,.F.,.F.,(4,3,3,3,3,3,3,3,3,3,
4),(0.,0.000277651260623857,0.000292700609901568,0.000476971360228736,0.000555302521247713,
0.000570297395023951,0.000664174349502761,0.00083295378187157,0.000971779412183499,
0.00104408940251943,0.00111060504249543),.UNSPECIFIED.);
#1018=B_SPLINE_CURVE_WITH_KNOTS('',3,(#59665,#59666,#59667,#59668,#59669,
#59670,#59671,#59672),.UNSPECIFIED.,.F.,.F.,(4,2,2,4),(-0.000622277040978629,
0.,0.0768376409886872,0.127182502679576),.UNSPECIFIED.);
#1019=B_SPLINE_CURVE_WITH_KNOTS('',3,(#59676,#59677,#59678,#59679,#59680,
#59681,#59682,#59683,#59684,#59685,#59686,#59687,#59688,#59689,#59690,#59691,
#59692,#59693,#59694,#59695,#59696,#59697,#59698,#59699,#59700,#59701,#59702,
#59703,#59704,#59705,#59706,#59707,#59708,#59709,#59710,#59711,#59712,#59713,
#59714,#59715,#59716,#59717,#59718,#59719,#59720,#59721,#59722,#59723,#59724,
#59725,#59726,#59727,#59728,#59729,#59730,#59731,#59732,#59733,#59734,#59735,
#59736,#59737,#59738,#59739,#59740,#59741,#59742,#59743,#59744,#59745,#59746,
#59747,#59748,#59749,#59750,#59751,#59752,#59753,#59754,#59755,#59756,#59757,
#59758,#59759,#59760,#59761,#59762,#59763,#59764,#59765,#59766,#59767,#59768,
#59769),.UNSPECIFIED.,.F.,.F.,(4,3,3,3,3,3,3,3,3,3,3,3,3,3,3,3,3,3,3,3,
3,3,3,3,3,3,3,3,3,3,3,4),(0.,5.04083481357633E-5,6.06628904997995E-5,0.00010114819054449,
0.000121325780999599,0.000151657226249498,0.000165282521792658,0.000178369354151246,
0.000204828211607868,0.000242651561999202,0.000258887470162885,0.000303314452499011,
0.000314495273876791,0.000328648098408335,0.0003429052739943,0.000363977342998827,
0.000424640233498611,0.000485303123998396,0.000515634569248287,0.000530800291873228,
0.00054596601449817,0.000606628904997954,0.000620350766208646,0.000687203566160806,
0.000727954685997538,0.000755915169194966,0.00077338354336116,0.000788617576497332,
0.000826258928547019,0.000849280466997126,0.00089781676624165,0.000970606247996704),
 .UNSPECIFIED.);
#1020=B_SPLINE_CURVE_WITH_KNOTS('',3,(#60714,#60715,#60716,#60717,#60718,
#60719,#60720,#60721,#60722,#60723,#60724,#60725),.UNSPECIFIED.,.F.,.F.,
(4,2,2,2,2,4),(-0.29661354335631,-0.278391574572434,-0.254432654164122,
-0.234687270338995,-0.214941886513867,-0.210821993248899),.UNSPECIFIED.);
#1021=B_SPLINE_CURVE_WITH_KNOTS('',3,(#61884,#61885,#61886,#61887,#61888,
#61889,#61890,#61891,#61892,#61893,#61894,#61895,#61896,#61897,#61898,#61899,
#61900,#61901,#61902,#61903,#61904,#61905,#61906,#61907,#61908),
 .UNSPECIFIED.,.F.,.F.,(4,3,3,3,3,3,3,3,4),(1.2869157614395E-10,0.00023065303768028,
0.000313885266238508,0.000470827899357743,0.000549299215917362,0.000588534874197172,
0.000608152703337074,0.000617961617907029,0.000627770532476985),
 .UNSPECIFIED.);
#1022=B_SPLINE_CURVE_WITH_KNOTS('',3,(#62605,#62606,#62607,#62608,#62609,
#62610,#62611,#62612,#62613,#62614),.UNSPECIFIED.,.F.,.F.,(4,2,2,2,4),(0.000465302741751488,
0.0107996201392302,0.0220542164513607,0.0339643336336735,0.0466183650451173),
 .UNSPECIFIED.);
#1023=B_SPLINE_CURVE_WITH_KNOTS('',3,(#62616,#62617,#62618,#62619,#62620,
#62621,#62622,#62623,#62624,#62625),.UNSPECIFIED.,.F.,.F.,(4,2,2,2,4),(0.141205929776987,
0.153859961188429,0.16577007837074,0.177024674682869,0.187358992080346),
 .UNSPECIFIED.);
#1024=B_SPLINE_CURVE_WITH_KNOTS('',3,(#62662,#62663,#62664,#62665,#62666,
#62667,#62668,#62669,#62670,#62671),.UNSPECIFIED.,.F.,.F.,(4,2,2,2,4),(-0.0891808869303931,
-0.0817048501723883,-0.0742536419552704,-0.0668368032479844,-0.0594502997646748),
 .UNSPECIFIED.);
#1025=B_SPLINE_CURVE_WITH_KNOTS('',3,(#62674,#62675,#62676,#62677,#62678,
#62679,#62680,#62681,#62682,#62683),.UNSPECIFIED.,.F.,.F.,(4,2,2,2,4),(0.0594551317141721,
0.0668412192577732,0.0742583320696144,0.081710598423227,0.0891882604952256),
 .UNSPECIFIED.);
#1026=B_SPLINE_CURVE_WITH_KNOTS('',3,(#62689,#62690,#62691,#62692,#62693,
#62694,#62695,#62696,#62697,#62698),.UNSPECIFIED.,.F.,.F.,(4,2,2,2,4),(0.,
0.0073991168916538,0.0148071582868911,0.022226415171961,0.0296556575450588),
 .UNSPECIFIED.);
#1027=B_SPLINE_CURVE_WITH_KNOTS('',3,(#62701,#62702,#62703,#62704,#62705,
#62706,#62707,#62708,#62709,#62710),.UNSPECIFIED.,.F.,.F.,(4,2,2,2,4),(0.0889741245006404,
0.0964039199286515,0.103823503599454,0.111231617988348,0.118630606154988),
 .UNSPECIFIED.);
#1028=B_SPLINE_CURVE_WITH_KNOTS('',3,(#62716,#62717,#62718,#62719,#62720,
#62721,#62722,#62723,#62724,#62725),.UNSPECIFIED.,.F.,.F.,(4,2,2,2,4),(0.0889715481092505,
0.0964007904823484,0.103820047367418,0.111228088762656,0.118627205654309),
 .UNSPECIFIED.);
#1029=B_SPLINE_CURVE_WITH_KNOTS('',3,(#62728,#62729,#62730,#62731,#62732,
#62733,#62734,#62735,#62736,#62737),.UNSPECIFIED.,.F.,.F.,(4,2,2,2,4),(0.,
0.00739898816663991,0.014807102555534,0.0222266862263364,0.0296564816543475),
 .UNSPECIFIED.);
#1030=B_SPLINE_CURVE_WITH_KNOTS('',3,(#62743,#62744,#62745,#62746,#62747,
#62748,#62749,#62750,#62751,#62752),.UNSPECIFIED.,.F.,.F.,(4,2,2,2,4),(0.0594502997646748,
0.0668368032479844,0.0742536419552704,0.0817048501723883,0.0891808869303931),
 .UNSPECIFIED.);
#1031=B_SPLINE_CURVE_WITH_KNOTS('',3,(#62755,#62756,#62757,#62758,#62759,
#62760,#62761,#62762,#62763,#62764),.UNSPECIFIED.,.F.,.F.,(4,2,2,2,4),(0.0297220029331187,
0.0371996650051172,0.0446519313587299,0.0520690441705711,0.0594551317141721),
 .UNSPECIFIED.);
#1032=CONICAL_SURFACE('',#15353,7.5,0.221314442347791);
#1033=CONICAL_SURFACE('',#15376,5.04017795657138,0.606317781856836);
#1034=CONICAL_SURFACE('',#15394,4.2,0.785398163397447);
#1035=CONICAL_SURFACE('',#15500,1.8001015361136,0.0225322446275356);
#1036=CONICAL_SURFACE('',#15503,1.78525,0.201741568445237);
#1037=CONICAL_SURFACE('',#15727,2.5,0.174532925199433);
#1038=CONICAL_SURFACE('',#15732,2.5,0.174532925199434);
#1039=CONICAL_SURFACE('',#15735,2.5,0.174532925199435);
#1040=CONICAL_SURFACE('',#15741,2.5,0.174532925199433);
#1041=CONICAL_SURFACE('',#15890,4.,0.785398163397448);
#1042=CONICAL_SURFACE('',#16191,1.1935,0.785398163397446);
#1043=CONICAL_SURFACE('',#16389,14.5,0.104223486416359);
#1044=CONICAL_SURFACE('',#16420,2.5,0.785398163397453);
#1045=CONICAL_SURFACE('',#16498,3.,0.0156237286204751);
#1046=CONICAL_SURFACE('',#16504,19.5,0.358770670270572);
#1047=CONICAL_SURFACE('',#16635,17.4363291775691,0.358770670270571);
#1048=CONICAL_SURFACE('',#16885,2.5,1.04719755119659);
#1049=CONICAL_SURFACE('',#16892,2.88,1.04719755119651);
#1050=CONICAL_SURFACE('',#16913,3.,0.785398163397449);
#1051=CONICAL_SURFACE('',#16915,3.0139499546386,0.335638550327472);
#1052=CONICAL_SURFACE('',#16917,2.88,1.04719755119651);
#1053=CONICAL_SURFACE('',#16919,2.88,1.04719755119651);
#1054=CONICAL_SURFACE('',#16921,2.88,1.04719755119651);
#1055=CONICAL_SURFACE('',#16924,2.88,1.04719755119651);
#1056=CONICAL_SURFACE('',#16926,2.88,1.04719755119651);
#1057=LINE('',#21397,#2250);
#1058=LINE('',#21402,#2251);
#1059=LINE('',#21407,#2252);
#1060=LINE('',#21413,#2253);
#1061=LINE('',#21419,#2254);
#1062=LINE('',#21451,#2255);
#1063=LINE('',#21454,#2256);
#1064=LINE('',#21469,#2257);
#1065=LINE('',#21475,#2258);
#1066=LINE('',#21482,#2259);
#1067=LINE('',#21486,#2260);
#1068=LINE('',#21492,#2261);
#1069=LINE('',#21498,#2262);
#1070=LINE('',#21504,#2263);
#1071=LINE('',#21516,#2264);
#1072=LINE('',#21521,#2265);
#1073=LINE('',#21526,#2266);
#1074=LINE('',#21536,#2267);
#1075=LINE('',#21538,#2268);
#1076=LINE('',#21540,#2269);
#1077=LINE('',#21541,#2270);
#1078=LINE('',#21545,#2271);
#1079=LINE('',#21546,#2272);
#1080=LINE('',#21547,#2273);
#1081=LINE('',#21550,#2274);
#1082=LINE('',#21551,#2275);
#1083=LINE('',#21554,#2276);
#1084=LINE('',#21555,#2277);
#1085=LINE('',#21559,#2278);
#1086=LINE('',#21561,#2279);
#1087=LINE('',#21563,#2280);
#1088=LINE('',#21564,#2281);
#1089=LINE('',#21568,#2282);
#1090=LINE('',#21570,#2283);
#1091=LINE('',#21571,#2284);
#1092=LINE('',#21572,#2285);
#1093=LINE('',#21575,#2286);
#1094=LINE('',#21576,#2287);
#1095=LINE('',#21580,#2288);
#1096=LINE('',#21582,#2289);
#1097=LINE('',#21584,#2290);
#1098=LINE('',#21585,#2291);
#1099=LINE('',#21589,#2292);
#1100=LINE('',#21590,#2293);
#1101=LINE('',#21591,#2294);
#1102=LINE('',#21595,#2295);
#1103=LINE('',#21596,#2296);
#1104=LINE('',#21597,#2297);
#1105=LINE('',#21600,#2298);
#1106=LINE('',#21602,#2299);
#1107=LINE('',#21603,#2300);
#1108=LINE('',#21606,#2301);
#1109=LINE('',#21607,#2302);
#1110=LINE('',#21609,#2303);
#1111=LINE('',#21610,#2304);
#1112=LINE('',#21613,#2305);
#1113=LINE('',#21615,#2306);
#1114=LINE('',#21616,#2307);
#1115=LINE('',#21617,#2308);
#1116=LINE('',#21619,#2309);
#1117=LINE('',#21623,#2310);
#1118=LINE('',#21624,#2311);
#1119=LINE('',#21625,#2312);
#1120=LINE('',#21628,#2313);
#1121=LINE('',#21629,#2314);
#1122=LINE('',#21632,#2315);
#1123=LINE('',#21633,#2316);
#1124=LINE('',#21635,#2317);
#1125=LINE('',#21640,#2318);
#1126=LINE('',#21642,#2319);
#1127=LINE('',#21644,#2320);
#1128=LINE('',#21645,#2321);
#1129=LINE('',#21649,#2322);
#1130=LINE('',#21651,#2323);
#1131=LINE('',#21653,#2324);
#1132=LINE('',#21654,#2325);
#1133=LINE('',#21657,#2326);
#1134=LINE('',#21659,#2327);
#1135=LINE('',#21661,#2328);
#1136=LINE('',#21663,#2329);
#1137=LINE('',#21664,#2330);
#1138=LINE('',#21666,#2331);
#1139=LINE('',#21669,#2332);
#1140=LINE('',#21671,#2333);
#1141=LINE('',#21672,#2334);
#1142=LINE('',#21675,#2335);
#1143=LINE('',#21677,#2336);
#1144=LINE('',#21678,#2337);
#1145=LINE('',#21681,#2338);
#1146=LINE('',#21682,#2339);
#1147=LINE('',#21683,#2340);
#1148=LINE('',#21685,#2341);
#1149=LINE('',#21687,#2342);
#1150=LINE('',#21688,#2343);
#1151=LINE('',#21691,#2344);
#1152=LINE('',#21692,#2345);
#1153=LINE('',#21694,#2346);
#1154=LINE('',#21695,#2347);
#1155=LINE('',#21697,#2348);
#1156=LINE('',#21700,#2349);
#1157=LINE('',#21702,#2350);
#1158=LINE('',#21703,#2351);
#1159=LINE('',#21705,#2352);
#1160=LINE('',#21706,#2353);
#1161=LINE('',#21708,#2354);
#1162=LINE('',#21709,#2355);
#1163=LINE('',#21711,#2356);
#1164=LINE('',#21713,#2357);
#1165=LINE('',#33847,#2358);
#1166=LINE('',#33850,#2359);
#1167=LINE('',#33853,#2360);
#1168=LINE('',#33855,#2361);
#1169=LINE('',#33856,#2362);
#1170=LINE('',#33862,#2363);
#1171=LINE('',#33867,#2364);
#1172=LINE('',#33869,#2365);
#1173=LINE('',#33871,#2366);
#1174=LINE('',#33872,#2367);
#1175=LINE('',#33874,#2368);
#1176=LINE('',#33875,#2369);
#1177=LINE('',#33877,#2370);
#1178=LINE('',#33878,#2371);
#1179=LINE('',#33881,#2372);
#1180=LINE('',#33882,#2373);
#1181=LINE('',#33891,#2374);
#1182=LINE('',#33893,#2375);
#1183=LINE('',#33895,#2376);
#1184=LINE('',#33896,#2377);
#1185=LINE('',#33899,#2378);
#1186=LINE('',#33901,#2379);
#1187=LINE('',#33902,#2380);
#1188=LINE('',#33905,#2381);
#1189=LINE('',#33906,#2382);
#1190=LINE('',#33910,#2383);
#1191=LINE('',#33911,#2384);
#1192=LINE('',#33913,#2385);
#1193=LINE('',#33921,#2386);
#1194=LINE('',#33972,#2387);
#1195=LINE('',#33980,#2388);
#1196=LINE('',#33985,#2389);
#1197=LINE('',#33990,#2390);
#1198=LINE('',#33992,#2391);
#1199=LINE('',#33993,#2392);
#1200=LINE('',#33997,#2393);
#1201=LINE('',#33998,#2394);
#1202=LINE('',#33999,#2395);
#1203=LINE('',#34002,#2396);
#1204=LINE('',#34003,#2397);
#1205=LINE('',#34006,#2398);
#1206=LINE('',#34007,#2399);
#1207=LINE('',#34010,#2400);
#1208=LINE('',#34011,#2401);
#1209=LINE('',#34014,#2402);
#1210=LINE('',#34015,#2403);
#1211=LINE('',#34018,#2404);
#1212=LINE('',#34019,#2405);
#1213=LINE('',#34022,#2406);
#1214=LINE('',#34023,#2407);
#1215=LINE('',#34026,#2408);
#1216=LINE('',#34027,#2409);
#1217=LINE('',#34030,#2410);
#1218=LINE('',#34031,#2411);
#1219=LINE('',#34034,#2412);
#1220=LINE('',#34035,#2413);
#1221=LINE('',#34038,#2414);
#1222=LINE('',#34039,#2415);
#1223=LINE('',#34042,#2416);
#1224=LINE('',#34043,#2417);
#1225=LINE('',#34046,#2418);
#1226=LINE('',#34047,#2419);
#1227=LINE('',#34050,#2420);
#1228=LINE('',#34051,#2421);
#1229=LINE('',#34054,#2422);
#1230=LINE('',#34055,#2423);
#1231=LINE('',#34058,#2424);
#1232=LINE('',#34059,#2425);
#1233=LINE('',#34061,#2426);
#1234=LINE('',#34064,#2427);
#1235=LINE('',#34065,#2428);
#1236=LINE('',#34067,#2429);
#1237=LINE('',#34082,#2430);
#1238=LINE('',#34090,#2431);
#1239=LINE('',#34103,#2432);
#1240=LINE('',#34153,#2433);
#1241=LINE('',#34156,#2434);
#1242=LINE('',#34158,#2435);
#1243=LINE('',#34160,#2436);
#1244=LINE('',#34164,#2437);
#1245=LINE('',#34169,#2438);
#1246=LINE('',#34170,#2439);
#1247=LINE('',#34172,#2440);
#1248=LINE('',#34178,#2441);
#1249=LINE('',#34179,#2442);
#1250=LINE('',#34181,#2443);
#1251=LINE('',#34184,#2444);
#1252=LINE('',#34186,#2445);
#1253=LINE('',#34187,#2446);
#1254=LINE('',#34192,#2447);
#1255=LINE('',#34195,#2448);
#1256=LINE('',#34199,#2449);
#1257=LINE('',#34200,#2450);
#1258=LINE('',#34202,#2451);
#1259=LINE('',#34204,#2452);
#1260=LINE('',#34206,#2453);
#1261=LINE('',#34210,#2454);
#1262=LINE('',#34212,#2455);
#1263=LINE('',#34213,#2456);
#1264=LINE('',#34214,#2457);
#1265=LINE('',#34215,#2458);
#1266=LINE('',#34264,#2459);
#1267=LINE('',#34269,#2460);
#1268=LINE('',#34271,#2461);
#1269=LINE('',#34274,#2462);
#1270=LINE('',#34278,#2463);
#1271=LINE('',#34280,#2464);
#1272=LINE('',#34281,#2465);
#1273=LINE('',#34284,#2466);
#1274=LINE('',#34285,#2467);
#1275=LINE('',#34288,#2468);
#1276=LINE('',#34290,#2469);
#1277=LINE('',#34292,#2470);
#1278=LINE('',#34294,#2471);
#1279=LINE('',#34296,#2472);
#1280=LINE('',#34298,#2473);
#1281=LINE('',#34300,#2474);
#1282=LINE('',#34302,#2475);
#1283=LINE('',#34304,#2476);
#1284=LINE('',#34306,#2477);
#1285=LINE('',#34308,#2478);
#1286=LINE('',#34310,#2479);
#1287=LINE('',#34312,#2480);
#1288=LINE('',#34314,#2481);
#1289=LINE('',#34316,#2482);
#1290=LINE('',#34318,#2483);
#1291=LINE('',#34320,#2484);
#1292=LINE('',#34321,#2485);
#1293=LINE('',#34323,#2486);
#1294=LINE('',#34324,#2487);
#1295=LINE('',#34326,#2488);
#1296=LINE('',#34328,#2489);
#1297=LINE('',#34330,#2490);
#1298=LINE('',#34332,#2491);
#1299=LINE('',#34334,#2492);
#1300=LINE('',#34336,#2493);
#1301=LINE('',#34338,#2494);
#1302=LINE('',#34340,#2495);
#1303=LINE('',#34342,#2496);
#1304=LINE('',#34344,#2497);
#1305=LINE('',#34346,#2498);
#1306=LINE('',#34348,#2499);
#1307=LINE('',#34350,#2500);
#1308=LINE('',#34352,#2501);
#1309=LINE('',#34354,#2502);
#1310=LINE('',#34359,#2503);
#1311=LINE('',#34363,#2504);
#1312=LINE('',#34367,#2505);
#1313=LINE('',#34371,#2506);
#1314=LINE('',#34373,#2507);
#1315=LINE('',#34379,#2508);
#1316=LINE('',#34381,#2509);
#1317=LINE('',#34383,#2510);
#1318=LINE('',#34385,#2511);
#1319=LINE('',#34387,#2512);
#1320=LINE('',#34389,#2513);
#1321=LINE('',#34391,#2514);
#1322=LINE('',#34393,#2515);
#1323=LINE('',#34395,#2516);
#1324=LINE('',#34397,#2517);
#1325=LINE('',#34399,#2518);
#1326=LINE('',#34401,#2519);
#1327=LINE('',#34403,#2520);
#1328=LINE('',#34405,#2521);
#1329=LINE('',#34407,#2522);
#1330=LINE('',#34409,#2523);
#1331=LINE('',#34411,#2524);
#1332=LINE('',#34413,#2525);
#1333=LINE('',#34415,#2526);
#1334=LINE('',#34416,#2527);
#1335=LINE('',#34418,#2528);
#1336=LINE('',#34419,#2529);
#1337=LINE('',#34421,#2530);
#1338=LINE('',#34423,#2531);
#1339=LINE('',#34425,#2532);
#1340=LINE('',#34427,#2533);
#1341=LINE('',#34429,#2534);
#1342=LINE('',#34431,#2535);
#1343=LINE('',#34433,#2536);
#1344=LINE('',#34435,#2537);
#1345=LINE('',#34437,#2538);
#1346=LINE('',#34439,#2539);
#1347=LINE('',#34441,#2540);
#1348=LINE('',#34443,#2541);
#1349=LINE('',#34445,#2542);
#1350=LINE('',#34447,#2543);
#1351=LINE('',#34449,#2544);
#1352=LINE('',#34451,#2545);
#1353=LINE('',#34453,#2546);
#1354=LINE('',#34455,#2547);
#1355=LINE('',#34485,#2548);
#1356=LINE('',#34488,#2549);
#1357=LINE('',#34493,#2550);
#1358=LINE('',#34500,#2551);
#1359=LINE('',#34503,#2552);
#1360=LINE('',#34509,#2553);
#1361=LINE('',#34512,#2554);
#1362=LINE('',#34518,#2555);
#1363=LINE('',#34523,#2556);
#1364=LINE('',#34527,#2557);
#1365=LINE('',#34529,#2558);
#1366=LINE('',#34531,#2559);
#1367=LINE('',#34532,#2560);
#1368=LINE('',#34535,#2561);
#1369=LINE('',#34537,#2562);
#1370=LINE('',#34538,#2563);
#1371=LINE('',#34541,#2564);
#1372=LINE('',#34543,#2565);
#1373=LINE('',#34544,#2566);
#1374=LINE('',#34548,#2567);
#1375=LINE('',#34550,#2568);
#1376=LINE('',#34552,#2569);
#1377=LINE('',#34553,#2570);
#1378=LINE('',#34557,#2571);
#1379=LINE('',#34558,#2572);
#1380=LINE('',#34559,#2573);
#1381=LINE('',#34563,#2574);
#1382=LINE('',#34564,#2575);
#1383=LINE('',#34565,#2576);
#1384=LINE('',#34569,#2577);
#1385=LINE('',#34571,#2578);
#1386=LINE('',#34573,#2579);
#1387=LINE('',#34574,#2580);
#1388=LINE('',#34578,#2581);
#1389=LINE('',#34580,#2582);
#1390=LINE('',#34582,#2583);
#1391=LINE('',#34583,#2584);
#1392=LINE('',#34585,#2585);
#1393=LINE('',#34587,#2586);
#1394=LINE('',#34589,#2587);
#1395=LINE('',#34590,#2588);
#1396=LINE('',#34592,#2589);
#1397=LINE('',#34594,#2590);
#1398=LINE('',#34596,#2591);
#1399=LINE('',#34598,#2592);
#1400=LINE('',#34600,#2593);
#1401=LINE('',#34601,#2594);
#1402=LINE('',#34605,#2595);
#1403=LINE('',#34606,#2596);
#1404=LINE('',#34607,#2597);
#1405=LINE('',#34611,#2598);
#1406=LINE('',#34612,#2599);
#1407=LINE('',#34613,#2600);
#1408=LINE('',#34619,#2601);
#1409=LINE('',#34620,#2602);
#1410=LINE('',#34622,#2603);
#1411=LINE('',#34624,#2604);
#1412=LINE('',#34627,#2605);
#1413=LINE('',#34631,#2606);
#1414=LINE('',#34633,#2607);
#1415=LINE('',#34635,#2608);
#1416=LINE('',#34641,#2609);
#1417=LINE('',#34643,#2610);
#1418=LINE('',#34645,#2611);
#1419=LINE('',#34647,#2612);
#1420=LINE('',#34649,#2613);
#1421=LINE('',#34650,#2614);
#1422=LINE('',#34654,#2615);
#1423=LINE('',#34656,#2616);
#1424=LINE('',#34658,#2617);
#1425=LINE('',#34660,#2618);
#1426=LINE('',#34662,#2619);
#1427=LINE('',#34663,#2620);
#1428=LINE('',#34666,#2621);
#1429=LINE('',#34668,#2622);
#1430=LINE('',#34669,#2623);
#1431=LINE('',#34673,#2624);
#1432=LINE('',#34675,#2625);
#1433=LINE('',#34677,#2626);
#1434=LINE('',#34678,#2627);
#1435=LINE('',#34682,#2628);
#1436=LINE('',#34684,#2629);
#1437=LINE('',#34686,#2630);
#1438=LINE('',#34687,#2631);
#1439=LINE('',#34688,#2632);
#1440=LINE('',#34691,#2633);
#1441=LINE('',#34692,#2634);
#1442=LINE('',#34695,#2635);
#1443=LINE('',#34697,#2636);
#1444=LINE('',#34698,#2637);
#1445=LINE('',#34700,#2638);
#1446=LINE('',#34703,#2639);
#1447=LINE('',#34704,#2640);
#1448=LINE('',#34708,#2641);
#1449=LINE('',#34709,#2642);
#1450=LINE('',#34710,#2643);
#1451=LINE('',#34712,#2644);
#1452=LINE('',#34716,#2645);
#1453=LINE('',#34720,#2646);
#1454=LINE('',#34724,#2647);
#1455=LINE('',#34726,#2648);
#1456=LINE('',#34727,#2649);
#1457=LINE('',#34730,#2650);
#1458=LINE('',#34732,#2651);
#1459=LINE('',#34733,#2652);
#1460=LINE('',#34738,#2653);
#1461=LINE('',#34744,#2654);
#1462=LINE('',#34748,#2655);
#1463=LINE('',#34750,#2656);
#1464=LINE('',#34751,#2657);
#1465=LINE('',#34754,#2658);
#1466=LINE('',#34756,#2659);
#1467=LINE('',#34757,#2660);
#1468=LINE('',#34760,#2661);
#1469=LINE('',#34761,#2662);
#1470=LINE('',#34766,#2663);
#1471=LINE('',#34768,#2664);
#1472=LINE('',#34769,#2665);
#1473=LINE('',#34774,#2666);
#1474=LINE('',#34776,#2667);
#1475=LINE('',#34777,#2668);
#1476=LINE('',#34778,#2669);
#1477=LINE('',#34779,#2670);
#1478=LINE('',#34782,#2671);
#1479=LINE('',#34784,#2672);
#1480=LINE('',#34785,#2673);
#1481=LINE('',#34791,#2674);
#1482=LINE('',#34794,#2675);
#1483=LINE('',#34796,#2676);
#1484=LINE('',#34798,#2677);
#1485=LINE('',#34799,#2678);
#1486=LINE('',#34805,#2679);
#1487=LINE('',#34810,#2680);
#1488=LINE('',#34813,#2681);
#1489=LINE('',#34814,#2682);
#1490=LINE('',#34819,#2683);
#1491=LINE('',#34826,#2684);
#1492=LINE('',#34829,#2685);
#1493=LINE('',#34831,#2686);
#1494=LINE('',#34832,#2687);
#1495=LINE('',#34841,#2688);
#1496=LINE('',#34843,#2689);
#1497=LINE('',#34845,#2690);
#1498=LINE('',#34847,#2691);
#1499=LINE('',#34852,#2692);
#1500=LINE('',#34856,#2693);
#1501=LINE('',#34858,#2694);
#1502=LINE('',#34859,#2695);
#1503=LINE('',#34861,#2696);
#1504=LINE('',#34865,#2697);
#1505=LINE('',#34867,#2698);
#1506=LINE('',#34869,#2699);
#1507=LINE('',#34870,#2700);
#1508=LINE('',#34872,#2701);
#1509=LINE('',#34873,#2702);
#1510=LINE('',#34878,#2703);
#1511=LINE('',#34880,#2704);
#1512=LINE('',#34882,#2705);
#1513=LINE('',#34883,#2706);
#1514=LINE('',#34884,#2707);
#1515=LINE('',#34888,#2708);
#1516=LINE('',#34889,#2709);
#1517=LINE('',#34890,#2710);
#1518=LINE('',#34892,#2711);
#1519=LINE('',#34893,#2712);
#1520=LINE('',#34896,#2713);
#1521=LINE('',#34898,#2714);
#1522=LINE('',#34900,#2715);
#1523=LINE('',#34902,#2716);
#1524=LINE('',#34904,#2717);
#1525=LINE('',#34905,#2718);
#1526=LINE('',#34907,#2719);
#1527=LINE('',#34908,#2720);
#1528=LINE('',#34911,#2721);
#1529=LINE('',#34913,#2722);
#1530=LINE('',#34914,#2723);
#1531=LINE('',#34917,#2724);
#1532=LINE('',#34919,#2725);
#1533=LINE('',#34920,#2726);
#1534=LINE('',#34922,#2727);
#1535=LINE('',#34924,#2728);
#1536=LINE('',#34926,#2729);
#1537=LINE('',#34929,#2730);
#1538=LINE('',#34931,#2731);
#1539=LINE('',#34932,#2732);
#1540=LINE('',#34934,#2733);
#1541=LINE('',#34936,#2734);
#1542=LINE('',#34939,#2735);
#1543=LINE('',#34940,#2736);
#1544=LINE('',#34943,#2737);
#1545=LINE('',#34945,#2738);
#1546=LINE('',#34947,#2739);
#1547=LINE('',#34948,#2740);
#1548=LINE('',#34951,#2741);
#1549=LINE('',#34953,#2742);
#1550=LINE('',#34954,#2743);
#1551=LINE('',#34956,#2744);
#1552=LINE('',#34958,#2745);
#1553=LINE('',#34960,#2746);
#1554=LINE('',#34961,#2747);
#1555=LINE('',#34964,#2748);
#1556=LINE('',#34966,#2749);
#1557=LINE('',#34967,#2750);
#1558=LINE('',#34974,#2751);
#1559=LINE('',#34977,#2752);
#1560=LINE('',#34978,#2753);
#1561=LINE('',#34981,#2754);
#1562=LINE('',#34983,#2755);
#1563=LINE('',#34984,#2756);
#1564=LINE('',#34987,#2757);
#1565=LINE('',#34989,#2758);
#1566=LINE('',#34990,#2759);
#1567=LINE('',#34992,#2760);
#1568=LINE('',#34994,#2761);
#1569=LINE('',#34995,#2762);
#1570=LINE('',#34998,#2763);
#1571=LINE('',#34999,#2764);
#1572=LINE('',#35000,#2765);
#1573=LINE('',#35003,#2766);
#1574=LINE('',#35005,#2767);
#1575=LINE('',#35008,#2768);
#1576=LINE('',#35010,#2769);
#1577=LINE('',#35014,#2770);
#1578=LINE('',#35019,#2771);
#1579=LINE('',#35020,#2772);
#1580=LINE('',#35023,#2773);
#1581=LINE('',#35025,#2774);
#1582=LINE('',#35028,#2775);
#1583=LINE('',#35031,#2776);
#1584=LINE('',#35032,#2777);
#1585=LINE('',#35035,#2778);
#1586=LINE('',#35037,#2779);
#1587=LINE('',#35039,#2780);
#1588=LINE('',#35040,#2781);
#1589=LINE('',#35044,#2782);
#1590=LINE('',#35047,#2783);
#1591=LINE('',#35050,#2784);
#1592=LINE('',#35051,#2785);
#1593=LINE('',#35054,#2786);
#1594=LINE('',#35055,#2787);
#1595=LINE('',#35058,#2788);
#1596=LINE('',#35060,#2789);
#1597=LINE('',#35061,#2790);
#1598=LINE('',#35063,#2791);
#1599=LINE('',#35067,#2792);
#1600=LINE('',#35069,#2793);
#1601=LINE('',#35070,#2794);
#1602=LINE('',#35073,#2795);
#1603=LINE('',#35077,#2796);
#1604=LINE('',#35078,#2797);
#1605=LINE('',#35081,#2798);
#1606=LINE('',#35085,#2799);
#1607=LINE('',#35086,#2800);
#1608=LINE('',#35089,#2801);
#1609=LINE('',#35093,#2802);
#1610=LINE('',#35098,#2803);
#1611=LINE('',#35099,#2804);
#1612=LINE('',#35100,#2805);
#1613=LINE('',#35102,#2806);
#1614=LINE('',#35103,#2807);
#1615=LINE('',#35108,#2808);
#1616=LINE('',#35110,#2809);
#1617=LINE('',#35112,#2810);
#1618=LINE('',#35113,#2811);
#1619=LINE('',#35117,#2812);
#1620=LINE('',#35119,#2813);
#1621=LINE('',#35121,#2814);
#1622=LINE('',#35122,#2815);
#1623=LINE('',#35126,#2816);
#1624=LINE('',#35127,#2817);
#1625=LINE('',#35128,#2818);
#1626=LINE('',#35129,#2819);
#1627=LINE('',#35132,#2820);
#1628=LINE('',#35133,#2821);
#1629=LINE('',#35136,#2822);
#1630=LINE('',#35137,#2823);
#1631=LINE('',#35139,#2824);
#1632=LINE('',#35140,#2825);
#1633=LINE('',#35143,#2826);
#1634=LINE('',#35144,#2827);
#1635=LINE('',#35146,#2828);
#1636=LINE('',#35550,#2829);
#1637=LINE('',#35558,#2830);
#1638=LINE('',#35565,#2831);
#1639=LINE('',#35571,#2832);
#1640=LINE('',#35575,#2833);
#1641=LINE('',#35592,#2834);
#1642=LINE('',#35609,#2835);
#1643=LINE('',#35613,#2836);
#1644=LINE('',#35620,#2837);
#1645=LINE('',#35624,#2838);
#1646=LINE('',#35645,#2839);
#1647=LINE('',#35717,#2840);
#1648=LINE('',#35728,#2841);
#1649=LINE('',#35841,#2842);
#1650=LINE('',#35844,#2843);
#1651=LINE('',#36060,#2844);
#1652=LINE('',#36075,#2845);
#1653=LINE('',#36079,#2846);
#1654=LINE('',#36151,#2847);
#1655=LINE('',#36159,#2848);
#1656=LINE('',#36347,#2849);
#1657=LINE('',#36349,#2850);
#1658=LINE('',#36352,#2851);
#1659=LINE('',#36355,#2852);
#1660=LINE('',#36360,#2853);
#1661=LINE('',#36366,#2854);
#1662=LINE('',#36584,#2855);
#1663=LINE('',#36599,#2856);
#1664=LINE('',#36603,#2857);
#1665=LINE('',#36607,#2858);
#1666=LINE('',#36611,#2859);
#1667=LINE('',#36631,#2860);
#1668=LINE('',#36634,#2861);
#1669=LINE('',#36678,#2862);
#1670=LINE('',#39178,#2863);
#1671=LINE('',#39180,#2864);
#1672=LINE('',#41332,#2865);
#1673=LINE('',#41333,#2866);
#1674=LINE('',#41336,#2867);
#1675=LINE('',#41338,#2868);
#1676=LINE('',#41339,#2869);
#1677=LINE('',#41341,#2870);
#1678=LINE('',#41342,#2871);
#1679=LINE('',#41343,#2872);
#1680=LINE('',#41345,#2873);
#1681=LINE('',#41346,#2874);
#1682=LINE('',#41347,#2875);
#1683=LINE('',#41351,#2876);
#1684=LINE('',#41353,#2877);
#1685=LINE('',#41355,#2878);
#1686=LINE('',#41356,#2879);
#1687=LINE('',#41360,#2880);
#1688=LINE('',#41362,#2881);
#1689=LINE('',#41364,#2882);
#1690=LINE('',#41365,#2883);
#1691=LINE('',#41369,#2884);
#1692=LINE('',#41371,#2885);
#1693=LINE('',#41373,#2886);
#1694=LINE('',#41374,#2887);
#1695=LINE('',#41376,#2888);
#1696=LINE('',#41378,#2889);
#1697=LINE('',#41380,#2890);
#1698=LINE('',#41416,#2891);
#1699=LINE('',#41447,#2892);
#1700=LINE('',#41449,#2893);
#1701=LINE('',#41451,#2894);
#1702=LINE('',#41496,#2895);
#1703=LINE('',#41497,#2896);
#1704=LINE('',#41503,#2897);
#1705=LINE('',#41505,#2898);
#1706=LINE('',#41506,#2899);
#1707=LINE('',#41652,#2900);
#1708=LINE('',#41655,#2901);
#1709=LINE('',#41957,#2902);
#1710=LINE('',#41958,#2903);
#1711=LINE('',#41961,#2904);
#1712=LINE('',#41962,#2905);
#1713=LINE('',#41964,#2906);
#1714=LINE('',#41965,#2907);
#1715=LINE('',#41966,#2908);
#1716=LINE('',#41968,#2909);
#1717=LINE('',#42001,#2910);
#1718=LINE('',#42003,#2911);
#1719=LINE('',#42005,#2912);
#1720=LINE('',#42007,#2913);
#1721=LINE('',#42010,#2914);
#1722=LINE('',#42011,#2915);
#1723=LINE('',#42033,#2916);
#1724=LINE('',#42410,#2917);
#1725=LINE('',#42414,#2918);
#1726=LINE('',#42563,#2919);
#1727=LINE('',#43117,#2920);
#1728=LINE('',#43136,#2921);
#1729=LINE('',#43140,#2922);
#1730=LINE('',#43145,#2923);
#1731=LINE('',#43147,#2924);
#1732=LINE('',#43176,#2925);
#1733=LINE('',#43187,#2926);
#1734=LINE('',#43192,#2927);
#1735=LINE('',#43196,#2928);
#1736=LINE('',#43197,#2929);
#1737=LINE('',#43199,#2930);
#1738=LINE('',#43203,#2931);
#1739=LINE('',#43204,#2932);
#1740=LINE('',#43206,#2933);
#1741=LINE('',#43207,#2934);
#1742=LINE('',#43211,#2935);
#1743=LINE('',#43213,#2936);
#1744=LINE('',#43221,#2937);
#1745=LINE('',#43223,#2938);
#1746=LINE('',#43225,#2939);
#1747=LINE('',#43226,#2940);
#1748=LINE('',#43230,#2941);
#1749=LINE('',#43380,#2942);
#1750=LINE('',#43549,#2943);
#1751=LINE('',#43750,#2944);
#1752=LINE('',#43753,#2945);
#1753=LINE('',#43756,#2946);
#1754=LINE('',#43759,#2947);
#1755=LINE('',#43763,#2948);
#1756=LINE('',#43769,#2949);
#1757=LINE('',#43787,#2950);
#1758=LINE('',#43790,#2951);
#1759=LINE('',#43794,#2952);
#1760=LINE('',#43799,#2953);
#1761=LINE('',#43803,#2954);
#1762=LINE('',#43807,#2955);
#1763=LINE('',#43810,#2956);
#1764=LINE('',#43812,#2957);
#1765=LINE('',#43814,#2958);
#1766=LINE('',#43815,#2959);
#1767=LINE('',#43914,#2960);
#1768=LINE('',#43936,#2961);
#1769=LINE('',#43977,#2962);
#1770=LINE('',#43979,#2963);
#1771=LINE('',#44215,#2964);
#1772=LINE('',#44216,#2965);
#1773=LINE('',#44427,#2966);
#1774=LINE('',#44428,#2967);
#1775=LINE('',#44430,#2968);
#1776=LINE('',#44469,#2969);
#1777=LINE('',#44474,#2970);
#1778=LINE('',#44479,#2971);
#1779=LINE('',#44483,#2972);
#1780=LINE('',#44485,#2973);
#1781=LINE('',#44486,#2974);
#1782=LINE('',#44489,#2975);
#1783=LINE('',#44490,#2976);
#1784=LINE('',#44493,#2977);
#1785=LINE('',#44494,#2978);
#1786=LINE('',#44497,#2979);
#1787=LINE('',#44498,#2980);
#1788=LINE('',#44501,#2981);
#1789=LINE('',#44502,#2982);
#1790=LINE('',#44505,#2983);
#1791=LINE('',#44506,#2984);
#1792=LINE('',#44509,#2985);
#1793=LINE('',#44510,#2986);
#1794=LINE('',#44513,#2987);
#1795=LINE('',#44514,#2988);
#1796=LINE('',#44517,#2989);
#1797=LINE('',#44518,#2990);
#1798=LINE('',#44521,#2991);
#1799=LINE('',#44522,#2992);
#1800=LINE('',#44525,#2993);
#1801=LINE('',#44526,#2994);
#1802=LINE('',#44528,#2995);
#1803=LINE('',#44535,#2996);
#1804=LINE('',#44550,#2997);
#1805=LINE('',#44565,#2998);
#1806=LINE('',#44570,#2999);
#1807=LINE('',#44575,#3000);
#1808=LINE('',#44579,#3001);
#1809=LINE('',#44584,#3002);
#1810=LINE('',#44589,#3003);
#1811=LINE('',#44604,#3004);
#1812=LINE('',#44619,#3005);
#1813=LINE('',#44634,#3006);
#1814=LINE('',#44650,#3007);
#1815=LINE('',#44655,#3008);
#1816=LINE('',#44661,#3009);
#1817=LINE('',#44676,#3010);
#1818=LINE('',#44691,#3011);
#1819=LINE('',#44695,#3012);
#1820=LINE('',#44700,#3013);
#1821=LINE('',#44715,#3014);
#1822=LINE('',#44730,#3015);
#1823=LINE('',#44745,#3016);
#1824=LINE('',#44761,#3017);
#1825=LINE('',#44776,#3018);
#1826=LINE('',#44791,#3019);
#1827=LINE('',#44806,#3020);
#1828=LINE('',#44823,#3021);
#1829=LINE('',#44829,#3022);
#1830=LINE('',#44835,#3023);
#1831=LINE('',#44842,#3024);
#1832=LINE('',#44845,#3025);
#1833=LINE('',#44850,#3026);
#1834=LINE('',#44856,#3027);
#1835=LINE('',#44862,#3028);
#1836=LINE('',#44866,#3029);
#1837=LINE('',#44870,#3030);
#1838=LINE('',#44876,#3031);
#1839=LINE('',#44882,#3032);
#1840=LINE('',#44888,#3033);
#1841=LINE('',#44892,#3034);
#1842=LINE('',#44896,#3035);
#1843=LINE('',#44903,#3036);
#1844=LINE('',#44908,#3037);
#1845=LINE('',#44916,#3038);
#1846=LINE('',#44920,#3039);
#1847=LINE('',#44921,#3040);
#1848=LINE('',#44923,#3041);
#1849=LINE('',#44924,#3042);
#1850=LINE('',#44930,#3043);
#1851=LINE('',#44933,#3044);
#1852=LINE('',#44935,#3045);
#1853=LINE('',#44936,#3046);
#1854=LINE('',#44937,#3047);
#1855=LINE('',#44940,#3048);
#1856=LINE('',#44943,#3049);
#1857=LINE('',#44946,#3050);
#1858=LINE('',#44948,#3051);
#1859=LINE('',#44950,#3052);
#1860=LINE('',#44951,#3053);
#1861=LINE('',#44954,#3054);
#1862=LINE('',#44957,#3055);
#1863=LINE('',#44959,#3056);
#1864=LINE('',#44961,#3057);
#1865=LINE('',#44964,#3058);
#1866=LINE('',#44966,#3059);
#1867=LINE('',#44967,#3060);
#1868=LINE('',#44969,#3061);
#1869=LINE('',#44970,#3062);
#1870=LINE('',#44975,#3063);
#1871=LINE('',#44976,#3064);
#1872=LINE('',#44981,#3065);
#1873=LINE('',#44985,#3066);
#1874=LINE('',#44987,#3067);
#1875=LINE('',#44988,#3068);
#1876=LINE('',#44992,#3069);
#1877=LINE('',#44994,#3070);
#1878=LINE('',#44995,#3071);
#1879=LINE('',#44998,#3072);
#1880=LINE('',#45000,#3073);
#1881=LINE('',#45001,#3074);
#1882=LINE('',#45003,#3075);
#1883=LINE('',#45006,#3076);
#1884=LINE('',#45010,#3077);
#1885=LINE('',#45011,#3078);
#1886=LINE('',#45017,#3079);
#1887=LINE('',#45020,#3080);
#1888=LINE('',#45023,#3081);
#1889=LINE('',#45025,#3082);
#1890=LINE('',#45026,#3083);
#1891=LINE('',#45030,#3084);
#1892=LINE('',#45032,#3085);
#1893=LINE('',#45034,#3086);
#1894=LINE('',#45035,#3087);
#1895=LINE('',#45036,#3088);
#1896=LINE('',#45039,#3089);
#1897=LINE('',#45041,#3090);
#1898=LINE('',#45042,#3091);
#1899=LINE('',#45044,#3092);
#1900=LINE('',#45047,#3093);
#1901=LINE('',#45049,#3094);
#1902=LINE('',#45050,#3095);
#1903=LINE('',#45052,#3096);
#1904=LINE('',#45053,#3097);
#1905=LINE('',#45055,#3098);
#1906=LINE('',#45059,#3099);
#1907=LINE('',#45060,#3100);
#1908=LINE('',#45062,#3101);
#1909=LINE('',#45063,#3102);
#1910=LINE('',#45069,#3103);
#1911=LINE('',#45072,#3104);
#1912=LINE('',#45074,#3105);
#1913=LINE('',#45075,#3106);
#1914=LINE('',#45076,#3107);
#1915=LINE('',#45079,#3108);
#1916=LINE('',#45082,#3109);
#1917=LINE('',#45086,#3110);
#1918=LINE('',#45089,#3111);
#1919=LINE('',#45091,#3112);
#1920=LINE('',#45094,#3113);
#1921=LINE('',#45095,#3114);
#1922=LINE('',#45106,#3115);
#1923=LINE('',#45108,#3116);
#1924=LINE('',#45110,#3117);
#1925=LINE('',#45111,#3118);
#1926=LINE('',#45114,#3119);
#1927=LINE('',#45116,#3120);
#1928=LINE('',#45117,#3121);
#1929=LINE('',#45121,#3122);
#1930=LINE('',#45123,#3123);
#1931=LINE('',#45125,#3124);
#1932=LINE('',#45126,#3125);
#1933=LINE('',#45131,#3126);
#1934=LINE('',#45135,#3127);
#1935=LINE('',#45137,#3128);
#1936=LINE('',#45138,#3129);
#1937=LINE('',#45143,#3130);
#1938=LINE('',#45147,#3131);
#1939=LINE('',#45149,#3132);
#1940=LINE('',#45150,#3133);
#1941=LINE('',#45155,#3134);
#1942=LINE('',#45159,#3135);
#1943=LINE('',#45163,#3136);
#1944=LINE('',#45166,#3137);
#1945=LINE('',#45167,#3138);
#1946=LINE('',#45169,#3139);
#1947=LINE('',#45172,#3140);
#1948=LINE('',#45173,#3141);
#1949=LINE('',#45175,#3142);
#1950=LINE('',#45195,#3143);
#1951=LINE('',#45217,#3144);
#1952=LINE('',#45298,#3145);
#1953=LINE('',#45301,#3146);
#1954=LINE('',#45307,#3147);
#1955=LINE('',#45310,#3148);
#1956=LINE('',#45313,#3149);
#1957=LINE('',#45319,#3150);
#1958=LINE('',#45324,#3151);
#1959=LINE('',#45329,#3152);
#1960=LINE('',#45335,#3153);
#1961=LINE('',#45341,#3154);
#1962=LINE('',#45347,#3155);
#1963=LINE('',#45354,#3156);
#1964=LINE('',#45357,#3157);
#1965=LINE('',#45362,#3158);
#1966=LINE('',#45368,#3159);
#1967=LINE('',#45372,#3160);
#1968=LINE('',#45378,#3161);
#1969=LINE('',#45385,#3162);
#1970=LINE('',#45387,#3163);
#1971=LINE('',#45388,#3164);
#1972=LINE('',#45392,#3165);
#1973=LINE('',#45394,#3166);
#1974=LINE('',#45396,#3167);
#1975=LINE('',#45397,#3168);
#1976=LINE('',#45400,#3169);
#1977=LINE('',#45402,#3170);
#1978=LINE('',#45403,#3171);
#1979=LINE('',#45406,#3172);
#1980=LINE('',#45408,#3173);
#1981=LINE('',#45410,#3174);
#1982=LINE('',#45411,#3175);
#1983=LINE('',#45414,#3176);
#1984=LINE('',#45416,#3177);
#1985=LINE('',#45417,#3178);
#1986=LINE('',#45420,#3179);
#1987=LINE('',#45422,#3180);
#1988=LINE('',#45423,#3181);
#1989=LINE('',#45429,#3182);
#1990=LINE('',#45432,#3183);
#1991=LINE('',#45434,#3184);
#1992=LINE('',#45435,#3185);
#1993=LINE('',#45441,#3186);
#1994=LINE('',#45444,#3187);
#1995=LINE('',#45446,#3188);
#1996=LINE('',#45447,#3189);
#1997=LINE('',#45451,#3190);
#1998=LINE('',#45459,#3191);
#1999=LINE('',#45462,#3192);
#2000=LINE('',#45466,#3193);
#2001=LINE('',#45468,#3194);
#2002=LINE('',#45470,#3195);
#2003=LINE('',#45471,#3196);
#2004=LINE('',#45474,#3197);
#2005=LINE('',#45476,#3198);
#2006=LINE('',#45478,#3199);
#2007=LINE('',#45479,#3200);
#2008=LINE('',#45482,#3201);
#2009=LINE('',#45483,#3202);
#2010=LINE('',#45485,#3203);
#2011=LINE('',#45486,#3204);
#2012=LINE('',#45487,#3205);
#2013=LINE('',#45490,#3206);
#2014=LINE('',#45491,#3207);
#2015=LINE('',#45493,#3208);
#2016=LINE('',#45495,#3209);
#2017=LINE('',#45496,#3210);
#2018=LINE('',#45499,#3211);
#2019=LINE('',#45501,#3212);
#2020=LINE('',#45503,#3213);
#2021=LINE('',#45504,#3214);
#2022=LINE('',#45510,#3215);
#2023=LINE('',#45512,#3216);
#2024=LINE('',#45514,#3217);
#2025=LINE('',#45515,#3218);
#2026=LINE('',#45521,#3219);
#2027=LINE('',#45527,#3220);
#2028=LINE('',#45530,#3221);
#2029=LINE('',#45531,#3222);
#2030=LINE('',#45534,#3223);
#2031=LINE('',#45535,#3224);
#2032=LINE('',#45537,#3225);
#2033=LINE('',#45538,#3226);
#2034=LINE('',#45541,#3227);
#2035=LINE('',#45542,#3228);
#2036=LINE('',#45544,#3229);
#2037=LINE('',#45547,#3230);
#2038=LINE('',#45551,#3231);
#2039=LINE('',#45554,#3232);
#2040=LINE('',#45555,#3233);
#2041=LINE('',#45559,#3234);
#2042=LINE('',#45562,#3235);
#2043=LINE('',#45564,#3236);
#2044=LINE('',#45597,#3237);
#2045=LINE('',#46086,#3238);
#2046=LINE('',#46368,#3239);
#2047=LINE('',#47036,#3240);
#2048=LINE('',#48369,#3241);
#2049=LINE('',#48909,#3242);
#2050=LINE('',#49043,#3243);
#2051=LINE('',#50240,#3244);
#2052=LINE('',#50244,#3245);
#2053=LINE('',#51646,#3246);
#2054=LINE('',#52119,#3247);
#2055=LINE('',#52122,#3248);
#2056=LINE('',#52141,#3249);
#2057=LINE('',#53447,#3250);
#2058=LINE('',#53473,#3251);
#2059=LINE('',#53486,#3252);
#2060=LINE('',#53489,#3253);
#2061=LINE('',#53491,#3254);
#2062=LINE('',#53708,#3255);
#2063=LINE('',#53712,#3256);
#2064=LINE('',#54041,#3257);
#2065=LINE('',#54507,#3258);
#2066=LINE('',#54513,#3259);
#2067=LINE('',#54519,#3260);
#2068=LINE('',#54533,#3261);
#2069=LINE('',#54536,#3262);
#2070=LINE('',#54541,#3263);
#2071=LINE('',#54544,#3264);
#2072=LINE('',#54553,#3265);
#2073=LINE('',#54554,#3266);
#2074=LINE('',#54563,#3267);
#2075=LINE('',#54689,#3268);
#2076=LINE('',#54692,#3269);
#2077=LINE('',#54696,#3270);
#2078=LINE('',#54965,#3271);
#2079=LINE('',#54969,#3272);
#2080=LINE('',#54972,#3273);
#2081=LINE('',#54976,#3274);
#2082=LINE('',#54979,#3275);
#2083=LINE('',#54984,#3276);
#2084=LINE('',#54999,#3277);
#2085=LINE('',#55005,#3278);
#2086=LINE('',#55013,#3279);
#2087=LINE('',#55021,#3280);
#2088=LINE('',#55027,#3281);
#2089=LINE('',#55102,#3282);
#2090=LINE('',#55107,#3283);
#2091=LINE('',#55122,#3284);
#2092=LINE('',#55123,#3285);
#2093=LINE('',#55124,#3286);
#2094=LINE('',#55128,#3287);
#2095=LINE('',#55135,#3288);
#2096=LINE('',#55137,#3289);
#2097=LINE('',#55140,#3290);
#2098=LINE('',#55143,#3291);
#2099=LINE('',#55144,#3292);
#2100=LINE('',#55147,#3293);
#2101=LINE('',#55151,#3294);
#2102=LINE('',#55152,#3295);
#2103=LINE('',#55155,#3296);
#2104=LINE('',#55158,#3297);
#2105=LINE('',#56070,#3298);
#2106=LINE('',#56071,#3299);
#2107=LINE('',#56076,#3300);
#2108=LINE('',#56077,#3301);
#2109=LINE('',#56089,#3302);
#2110=LINE('',#56090,#3303);
#2111=LINE('',#56095,#3304);
#2112=LINE('',#56096,#3305);
#2113=LINE('',#56105,#3306);
#2114=LINE('',#56106,#3307);
#2115=LINE('',#56111,#3308);
#2116=LINE('',#56112,#3309);
#2117=LINE('',#56121,#3310);
#2118=LINE('',#56122,#3311);
#2119=LINE('',#56125,#3312);
#2120=LINE('',#56128,#3313);
#2121=LINE('',#56137,#3314);
#2122=LINE('',#56138,#3315);
#2123=LINE('',#56143,#3316);
#2124=LINE('',#56145,#3317);
#2125=LINE('',#56151,#3318);
#2126=LINE('',#56152,#3319);
#2127=LINE('',#56155,#3320);
#2128=LINE('',#56158,#3321);
#2129=LINE('',#56162,#3322);
#2130=LINE('',#56163,#3323);
#2131=LINE('',#56167,#3324);
#2132=LINE('',#56168,#3325);
#2133=LINE('',#56171,#3326);
#2134=LINE('',#56174,#3327);
#2135=LINE('',#56178,#3328);
#2136=LINE('',#56181,#3329);
#2137=LINE('',#56189,#3330);
#2138=LINE('',#56190,#3331);
#2139=LINE('',#56192,#3332);
#2140=LINE('',#56193,#3333);
#2141=LINE('',#56195,#3334);
#2142=LINE('',#56196,#3335);
#2143=LINE('',#56199,#3336);
#2144=LINE('',#56202,#3337);
#2145=LINE('',#56204,#3338);
#2146=LINE('',#56207,#3339);
#2147=LINE('',#56208,#3340);
#2148=LINE('',#56210,#3341);
#2149=LINE('',#56212,#3342);
#2150=LINE('',#56217,#3343);
#2151=LINE('',#56218,#3344);
#2152=LINE('',#56219,#3345);
#2153=LINE('',#56223,#3346);
#2154=LINE('',#56227,#3347);
#2155=LINE('',#56230,#3348);
#2156=LINE('',#56231,#3349);
#2157=LINE('',#56238,#3350);
#2158=LINE('',#56239,#3351);
#2159=LINE('',#56249,#3352);
#2160=LINE('',#56251,#3353);
#2161=LINE('',#56252,#3354);
#2162=LINE('',#56254,#3355);
#2163=LINE('',#56256,#3356);
#2164=LINE('',#56404,#3357);
#2165=LINE('',#56452,#3358);
#2166=LINE('',#56454,#3359);
#2167=LINE('',#56456,#3360);
#2168=LINE('',#56459,#3361);
#2169=LINE('',#56460,#3362);
#2170=LINE('',#56464,#3363);
#2171=LINE('',#56467,#3364);
#2172=LINE('',#56469,#3365);
#2173=LINE('',#56470,#3366);
#2174=LINE('',#57048,#3367);
#2175=LINE('',#57272,#3368);
#2176=LINE('',#58852,#3369);
#2177=LINE('',#58853,#3370);
#2178=LINE('',#58857,#3371);
#2179=LINE('',#58862,#3372);
#2180=LINE('',#58994,#3373);
#2181=LINE('',#58996,#3374);
#2182=LINE('',#58997,#3375);
#2183=LINE('',#59000,#3376);
#2184=LINE('',#59001,#3377);
#2185=LINE('',#59002,#3378);
#2186=LINE('',#59006,#3379);
#2187=LINE('',#59007,#3380);
#2188=LINE('',#59009,#3381);
#2189=LINE('',#59013,#3382);
#2190=LINE('',#59019,#3383);
#2191=LINE('',#59020,#3384);
#2192=LINE('',#59022,#3385);
#2193=LINE('',#59026,#3386);
#2194=LINE('',#59031,#3387);
#2195=LINE('',#59034,#3388);
#2196=LINE('',#59037,#3389);
#2197=LINE('',#59039,#3390);
#2198=LINE('',#59040,#3391);
#2199=LINE('',#59050,#3392);
#2200=LINE('',#59051,#3393);
#2201=LINE('',#60713,#3394);
#2202=LINE('',#62630,#3395);
#2203=LINE('',#62634,#3396);
#2204=LINE('',#62637,#3397);
#2205=LINE('',#62646,#3398);
#2206=LINE('',#62652,#3399);
#2207=LINE('',#62766,#3400);
#2208=LINE('',#62767,#3401);
#2209=LINE('',#62769,#3402);
#2210=LINE('',#62770,#3403);
#2211=LINE('',#62772,#3404);
#2212=LINE('',#62773,#3405);
#2213=LINE('',#62775,#3406);
#2214=LINE('',#62776,#3407);
#2215=LINE('',#62783,#3408);
#2216=LINE('',#62812,#3409);
#2217=LINE('',#62824,#3410);
#2218=LINE('',#62836,#3411);
#2219=LINE('',#62839,#3412);
#2220=LINE('',#62864,#3413);
#2221=LINE('',#62865,#3414);
#2222=LINE('',#62882,#3415);
#2223=LINE('',#62883,#3416);
#2224=LINE('',#62886,#3417);
#2225=LINE('',#62887,#3418);
#2226=LINE('',#62891,#3419);
#2227=LINE('',#62892,#3420);
#2228=LINE('',#62894,#3421);
#2229=LINE('',#62895,#3422);
#2230=LINE('',#62897,#3423);
#2231=LINE('',#62899,#3424);
#2232=LINE('',#62900,#3425);
#2233=LINE('',#62902,#3426);
#2234=LINE('',#62904,#3427);
#2235=LINE('',#62906,#3428);
#2236=LINE('',#62907,#3429);
#2237=LINE('',#62909,#3430);
#2238=LINE('',#62910,#3431);
#2239=LINE('',#62912,#3432);
#2240=LINE('',#62914,#3433);
#2241=LINE('',#62915,#3434);
#2242=LINE('',#62918,#3435);
#2243=LINE('',#62920,#3436);
#2244=LINE('',#62921,#3437);
#2245=LINE('',#62922,#3438);
#2246=LINE('',#62924,#3439);
#2247=LINE('',#62925,#3440);
#2248=LINE('',#62926,#3441);
#2249=LINE('',#62927,#3442);
#2250=VECTOR('',#16970,6.25);
#2251=VECTOR('',#16977,6.25);
#2252=VECTOR('',#16982,2.25);
#2253=VECTOR('',#16989,3.);
#2254=VECTOR('',#16996,7.5);
#2255=VECTOR('',#17005,1000.);
#2256=VECTOR('',#17008,1000.);
#2257=VECTOR('',#17025,4.);
#2258=VECTOR('',#17032,5.25);
#2259=VECTOR('',#17041,5.04017795657138);
#2260=VECTOR('',#17046,5.04017795657138);
#2261=VECTOR('',#17053,0.300000000000003);
#2262=VECTOR('',#17060,0.300000000000003);
#2263=VECTOR('',#17067,4.);
#2264=VECTOR('',#17082,4.2);
#2265=VECTOR('',#17089,4.2);
#2266=VECTOR('',#17094,5.8);
#2267=VECTOR('',#17109,1000.);
#2268=VECTOR('',#17110,1000.);
#2269=VECTOR('',#17111,1000.);
#2270=VECTOR('',#17112,1000.);
#2271=VECTOR('',#17115,1000.);
#2272=VECTOR('',#17116,1000.);
#2273=VECTOR('',#17117,1000.);
#2274=VECTOR('',#17120,1000.);
#2275=VECTOR('',#17121,1000.);
#2276=VECTOR('',#17124,1000.);
#2277=VECTOR('',#17125,1000.);
#2278=VECTOR('',#17128,1000.);
#2279=VECTOR('',#17129,1000.);
#2280=VECTOR('',#17130,1000.);
#2281=VECTOR('',#17131,1000.);
#2282=VECTOR('',#17134,1000.);
#2283=VECTOR('',#17135,1000.);
#2284=VECTOR('',#17136,1000.);
#2285=VECTOR('',#17137,1000.);
#2286=VECTOR('',#17140,1000.);
#2287=VECTOR('',#17141,1000.);
#2288=VECTOR('',#17144,1000.);
#2289=VECTOR('',#17145,1000.);
#2290=VECTOR('',#17146,1000.);
#2291=VECTOR('',#17147,1000.);
#2292=VECTOR('',#17150,1000.);
#2293=VECTOR('',#17151,1000.);
#2294=VECTOR('',#17152,1000.);
#2295=VECTOR('',#17155,1000.);
#2296=VECTOR('',#17156,1000.);
#2297=VECTOR('',#17157,1000.);
#2298=VECTOR('',#17160,1000.);
#2299=VECTOR('',#17161,1000.);
#2300=VECTOR('',#17162,1000.);
#2301=VECTOR('',#17165,1000.);
#2302=VECTOR('',#17166,1000.);
#2303=VECTOR('',#17169,1000.);
#2304=VECTOR('',#17170,1000.);
#2305=VECTOR('',#17173,1000.);
#2306=VECTOR('',#17174,1000.);
#2307=VECTOR('',#17175,1000.);
#2308=VECTOR('',#17176,1000.);
#2309=VECTOR('',#17179,1000.);
#2310=VECTOR('',#17182,1000.);
#2311=VECTOR('',#17183,1000.);
#2312=VECTOR('',#17184,1000.);
#2313=VECTOR('',#17187,1000.);
#2314=VECTOR('',#17188,1000.);
#2315=VECTOR('',#17191,1000.);
#2316=VECTOR('',#17192,1000.);
#2317=VECTOR('',#17195,1000.);
#2318=VECTOR('',#17200,1000.);
#2319=VECTOR('',#17201,1000.);
#2320=VECTOR('',#17202,1000.);
#2321=VECTOR('',#17203,1000.);
#2322=VECTOR('',#17206,1000.);
#2323=VECTOR('',#17207,1000.);
#2324=VECTOR('',#17208,1000.);
#2325=VECTOR('',#17209,1000.);
#2326=VECTOR('',#17212,1000.);
#2327=VECTOR('',#17213,1000.);
#2328=VECTOR('',#17214,1000.);
#2329=VECTOR('',#17215,1000.);
#2330=VECTOR('',#17216,1000.);
#2331=VECTOR('',#17219,1000.);
#2332=VECTOR('',#17222,1000.);
#2333=VECTOR('',#17223,1000.);
#2334=VECTOR('',#17224,1000.);
#2335=VECTOR('',#17227,1000.);
#2336=VECTOR('',#17228,1000.);
#2337=VECTOR('',#17229,1000.);
#2338=VECTOR('',#17232,1000.);
#2339=VECTOR('',#17233,1000.);
#2340=VECTOR('',#17234,1000.);
#2341=VECTOR('',#17237,1000.);
#2342=VECTOR('',#17238,1000.);
#2343=VECTOR('',#17239,1000.);
#2344=VECTOR('',#17242,1000.);
#2345=VECTOR('',#17243,1000.);
#2346=VECTOR('',#17246,1000.);
#2347=VECTOR('',#17247,1000.);
#2348=VECTOR('',#17250,1000.);
#2349=VECTOR('',#17253,1000.);
#2350=VECTOR('',#17254,1000.);
#2351=VECTOR('',#17255,1000.);
#2352=VECTOR('',#17258,1000.);
#2353=VECTOR('',#17259,1000.);
#2354=VECTOR('',#17262,1000.);
#2355=VECTOR('',#17263,1000.);
#2356=VECTOR('',#17266,1000.);
#2357=VECTOR('',#17269,1000.);
#2358=VECTOR('',#17284,1000.);
#2359=VECTOR('',#17287,1000.);
#2360=VECTOR('',#17290,1000.);
#2361=VECTOR('',#17291,1000.);
#2362=VECTOR('',#17292,1000.);
#2363=VECTOR('',#17299,1000.);
#2364=VECTOR('',#17304,1000.);
#2365=VECTOR('',#17305,1000.);
#2366=VECTOR('',#17306,1000.);
#2367=VECTOR('',#17307,1000.);
#2368=VECTOR('',#17310,1000.);
#2369=VECTOR('',#17311,1000.);
#2370=VECTOR('',#17314,1000.);
#2371=VECTOR('',#17315,1000.);
#2372=VECTOR('',#17320,1000.);
#2373=VECTOR('',#17321,1000.);
#2374=VECTOR('',#17334,1000.);
#2375=VECTOR('',#17335,1000.);
#2376=VECTOR('',#17336,1000.);
#2377=VECTOR('',#17337,1000.);
#2378=VECTOR('',#17340,1000.);
#2379=VECTOR('',#17341,1000.);
#2380=VECTOR('',#17342,1000.);
#2381=VECTOR('',#17345,1000.);
#2382=VECTOR('',#17346,1000.);
#2383=VECTOR('',#17351,1000.);
#2384=VECTOR('',#17352,1000.);
#2385=VECTOR('',#17355,1000.);
#2386=VECTOR('',#17366,4.);
#2387=VECTOR('',#17421,1.8001015361136);
#2388=VECTOR('',#17430,1.78525);
#2389=VECTOR('',#17437,2.);
#2390=VECTOR('',#17444,1000.);
#2391=VECTOR('',#17445,1000.);
#2392=VECTOR('',#17446,1000.);
#2393=VECTOR('',#17449,1000.);
#2394=VECTOR('',#17450,1000.);
#2395=VECTOR('',#17451,1000.);
#2396=VECTOR('',#17454,1000.);
#2397=VECTOR('',#17455,1000.);
#2398=VECTOR('',#17458,1000.);
#2399=VECTOR('',#17459,1000.);
#2400=VECTOR('',#17462,1000.);
#2401=VECTOR('',#17463,1000.);
#2402=VECTOR('',#17466,1000.);
#2403=VECTOR('',#17467,1000.);
#2404=VECTOR('',#17470,1000.);
#2405=VECTOR('',#17471,1000.);
#2406=VECTOR('',#17474,1000.);
#2407=VECTOR('',#17475,1000.);
#2408=VECTOR('',#17478,1000.);
#2409=VECTOR('',#17479,1000.);
#2410=VECTOR('',#17482,1000.);
#2411=VECTOR('',#17483,1000.);
#2412=VECTOR('',#17486,1000.);
#2413=VECTOR('',#17487,1000.);
#2414=VECTOR('',#17490,1000.);
#2415=VECTOR('',#17491,1000.);
#2416=VECTOR('',#17494,1000.);
#2417=VECTOR('',#17495,1000.);
#2418=VECTOR('',#17498,1000.);
#2419=VECTOR('',#17499,1000.);
#2420=VECTOR('',#17502,1000.);
#2421=VECTOR('',#17503,1000.);
#2422=VECTOR('',#17506,1000.);
#2423=VECTOR('',#17507,1000.);
#2424=VECTOR('',#17510,1000.);
#2425=VECTOR('',#17511,1000.);
#2426=VECTOR('',#17514,1000.);
#2427=VECTOR('',#17517,1000.);
#2428=VECTOR('',#17518,1000.);
#2429=VECTOR('',#17521,1000.);
#2430=VECTOR('',#17528,1000.);
#2431=VECTOR('',#17535,1000.);
#2432=VECTOR('',#17548,3.);
#2433=VECTOR('',#17601,4.);
#2434=VECTOR('',#17604,1000.);
#2435=VECTOR('',#17605,1000.);
#2436=VECTOR('',#17606,1000.);
#2437=VECTOR('',#17609,4.);
#2438=VECTOR('',#17614,1000.);
#2439=VECTOR('',#17615,1000.);
#2440=VECTOR('',#17616,1000.);
#2441=VECTOR('',#17621,1000.);
#2442=VECTOR('',#17622,1000.);
#2443=VECTOR('',#17623,1000.);
#2444=VECTOR('',#17626,1000.);
#2445=VECTOR('',#17627,1000.);
#2446=VECTOR('',#17628,1000.);
#2447=VECTOR('',#17631,1000.);
#2448=VECTOR('',#17634,1000.);
#2449=VECTOR('',#17637,1000.);
#2450=VECTOR('',#17638,1000.);
#2451=VECTOR('',#17639,1000.);
#2452=VECTOR('',#17640,1000.);
#2453=VECTOR('',#17641,1000.);
#2454=VECTOR('',#17644,1000.);
#2455=VECTOR('',#17645,1000.);
#2456=VECTOR('',#17646,1000.);
#2457=VECTOR('',#17647,1000.);
#2458=VECTOR('',#17648,1000.);
#2459=VECTOR('',#17701,3.);
#2460=VECTOR('',#17710,1000.);
#2461=VECTOR('',#17713,1000.);
#2462=VECTOR('',#17718,1000.);
#2463=VECTOR('',#17723,1000.);
#2464=VECTOR('',#17724,1000.);
#2465=VECTOR('',#17725,1000.);
#2466=VECTOR('',#17728,1000.);
#2467=VECTOR('',#17729,1000.);
#2468=VECTOR('',#17732,1000.);
#2469=VECTOR('',#17733,1000.);
#2470=VECTOR('',#17734,1000.);
#2471=VECTOR('',#17735,1000.);
#2472=VECTOR('',#17736,1000.);
#2473=VECTOR('',#17737,1000.);
#2474=VECTOR('',#17738,1000.);
#2475=VECTOR('',#17739,1000.);
#2476=VECTOR('',#17740,1000.);
#2477=VECTOR('',#17741,1000.);
#2478=VECTOR('',#17742,1000.);
#2479=VECTOR('',#17743,1000.);
#2480=VECTOR('',#17744,1000.);
#2481=VECTOR('',#17745,1000.);
#2482=VECTOR('',#17746,1000.);
#2483=VECTOR('',#17747,1000.);
#2484=VECTOR('',#17748,1000.);
#2485=VECTOR('',#17749,1000.);
#2486=VECTOR('',#17752,1000.);
#2487=VECTOR('',#17753,1000.);
#2488=VECTOR('',#17756,1000.);
#2489=VECTOR('',#17759,1000.);
#2490=VECTOR('',#17762,1000.);
#2491=VECTOR('',#17765,1000.);
#2492=VECTOR('',#17768,1000.);
#2493=VECTOR('',#17771,1000.);
#2494=VECTOR('',#17774,1000.);
#2495=VECTOR('',#17777,1000.);
#2496=VECTOR('',#17780,1000.);
#2497=VECTOR('',#17783,1000.);
#2498=VECTOR('',#17786,1000.);
#2499=VECTOR('',#17789,1000.);
#2500=VECTOR('',#17792,1000.);
#2501=VECTOR('',#17795,1000.);
#2502=VECTOR('',#17798,1000.);
#2503=VECTOR('',#17807,1000.);
#2504=VECTOR('',#17814,1000.);
#2505=VECTOR('',#17821,1000.);
#2506=VECTOR('',#17828,1000.);
#2507=VECTOR('',#17831,1000.);
#2508=VECTOR('',#17838,1000.);
#2509=VECTOR('',#17839,1000.);
#2510=VECTOR('',#17840,1000.);
#2511=VECTOR('',#17841,1000.);
#2512=VECTOR('',#17842,1000.);
#2513=VECTOR('',#17843,1000.);
#2514=VECTOR('',#17844,1000.);
#2515=VECTOR('',#17845,1000.);
#2516=VECTOR('',#17846,1000.);
#2517=VECTOR('',#17847,1000.);
#2518=VECTOR('',#17848,1000.);
#2519=VECTOR('',#17849,1000.);
#2520=VECTOR('',#17850,1000.);
#2521=VECTOR('',#17851,1000.);
#2522=VECTOR('',#17852,1000.);
#2523=VECTOR('',#17853,1000.);
#2524=VECTOR('',#17854,1000.);
#2525=VECTOR('',#17855,1000.);
#2526=VECTOR('',#17856,1000.);
#2527=VECTOR('',#17857,1000.);
#2528=VECTOR('',#17860,1000.);
#2529=VECTOR('',#17861,1000.);
#2530=VECTOR('',#17864,1000.);
#2531=VECTOR('',#17867,1000.);
#2532=VECTOR('',#17870,1000.);
#2533=VECTOR('',#17873,1000.);
#2534=VECTOR('',#17876,1000.);
#2535=VECTOR('',#17879,1000.);
#2536=VECTOR('',#17882,1000.);
#2537=VECTOR('',#17885,1000.);
#2538=VECTOR('',#17888,1000.);
#2539=VECTOR('',#17891,1000.);
#2540=VECTOR('',#17894,1000.);
#2541=VECTOR('',#17897,1000.);
#2542=VECTOR('',#17900,1000.);
#2543=VECTOR('',#17903,1000.);
#2544=VECTOR('',#17906,1000.);
#2545=VECTOR('',#17909,1000.);
#2546=VECTOR('',#17912,1000.);
#2547=VECTOR('',#17915,1000.);
#2548=VECTOR('',#17948,1000.);
#2549=VECTOR('',#17951,1000.);
#2550=VECTOR('',#17956,2.067);
#2551=VECTOR('',#17963,1000.);
#2552=VECTOR('',#17966,1000.);
#2553=VECTOR('',#17971,1000.);
#2554=VECTOR('',#17974,1000.);
#2555=VECTOR('',#17979,1000.);
#2556=VECTOR('',#17984,1000.);
#2557=VECTOR('',#17987,1000.);
#2558=VECTOR('',#17988,1000.);
#2559=VECTOR('',#17989,1000.);
#2560=VECTOR('',#17990,1000.);
#2561=VECTOR('',#17993,1000.);
#2562=VECTOR('',#17994,1000.);
#2563=VECTOR('',#17995,1000.);
#2564=VECTOR('',#17998,1000.);
#2565=VECTOR('',#17999,1000.);
#2566=VECTOR('',#18000,1000.);
#2567=VECTOR('',#18003,1000.);
#2568=VECTOR('',#18004,1000.);
#2569=VECTOR('',#18005,1000.);
#2570=VECTOR('',#18006,1000.);
#2571=VECTOR('',#18009,1000.);
#2572=VECTOR('',#18010,1000.);
#2573=VECTOR('',#18011,1000.);
#2574=VECTOR('',#18014,1000.);
#2575=VECTOR('',#18015,1000.);
#2576=VECTOR('',#18016,1000.);
#2577=VECTOR('',#18019,1000.);
#2578=VECTOR('',#18020,1000.);
#2579=VECTOR('',#18021,1000.);
#2580=VECTOR('',#18022,1000.);
#2581=VECTOR('',#18025,1000.);
#2582=VECTOR('',#18026,1000.);
#2583=VECTOR('',#18027,1000.);
#2584=VECTOR('',#18028,1000.);
#2585=VECTOR('',#18031,1000.);
#2586=VECTOR('',#18032,1000.);
#2587=VECTOR('',#18033,1000.);
#2588=VECTOR('',#18034,1000.);
#2589=VECTOR('',#18037,1000.);
#2590=VECTOR('',#18038,1000.);
#2591=VECTOR('',#18039,1000.);
#2592=VECTOR('',#18040,1000.);
#2593=VECTOR('',#18041,1000.);
#2594=VECTOR('',#18042,1000.);
#2595=VECTOR('',#18045,1000.);
#2596=VECTOR('',#18046,1000.);
#2597=VECTOR('',#18047,1000.);
#2598=VECTOR('',#18050,1000.);
#2599=VECTOR('',#18051,1000.);
#2600=VECTOR('',#18052,1000.);
#2601=VECTOR('',#18057,1000.);
#2602=VECTOR('',#18058,1000.);
#2603=VECTOR('',#18059,1000.);
#2604=VECTOR('',#18060,1000.);
#2605=VECTOR('',#18063,1000.);
#2606=VECTOR('',#18066,1000.);
#2607=VECTOR('',#18067,1000.);
#2608=VECTOR('',#18068,1000.);
#2609=VECTOR('',#18075,1000.);
#2610=VECTOR('',#18076,1000.);
#2611=VECTOR('',#18077,1000.);
#2612=VECTOR('',#18078,1000.);
#2613=VECTOR('',#18079,1000.);
#2614=VECTOR('',#18080,1000.);
#2615=VECTOR('',#18083,1000.);
#2616=VECTOR('',#18084,1000.);
#2617=VECTOR('',#18085,1000.);
#2618=VECTOR('',#18086,1000.);
#2619=VECTOR('',#18087,1000.);
#2620=VECTOR('',#18088,1000.);
#2621=VECTOR('',#18091,1000.);
#2622=VECTOR('',#18092,1000.);
#2623=VECTOR('',#18093,1000.);
#2624=VECTOR('',#18096,1000.);
#2625=VECTOR('',#18097,1000.);
#2626=VECTOR('',#18098,1000.);
#2627=VECTOR('',#18099,1000.);
#2628=VECTOR('',#18102,1000.);
#2629=VECTOR('',#18103,1000.);
#2630=VECTOR('',#18104,1000.);
#2631=VECTOR('',#18105,1000.);
#2632=VECTOR('',#18106,1000.);
#2633=VECTOR('',#18109,1000.);
#2634=VECTOR('',#18110,1000.);
#2635=VECTOR('',#18113,1000.);
#2636=VECTOR('',#18114,1000.);
#2637=VECTOR('',#18115,1000.);
#2638=VECTOR('',#18118,1000.);
#2639=VECTOR('',#18121,1000.);
#2640=VECTOR('',#18122,1000.);
#2641=VECTOR('',#18125,1000.);
#2642=VECTOR('',#18126,1000.);
#2643=VECTOR('',#18127,1000.);
#2644=VECTOR('',#18130,1000.);
#2645=VECTOR('',#18133,1000.);
#2646=VECTOR('',#18136,1000.);
#2647=VECTOR('',#18141,1000.);
#2648=VECTOR('',#18142,1000.);
#2649=VECTOR('',#18143,1000.);
#2650=VECTOR('',#18146,1000.);
#2651=VECTOR('',#18147,1000.);
#2652=VECTOR('',#18148,1000.);
#2653=VECTOR('',#18153,1000.);
#2654=VECTOR('',#18160,1000.);
#2655=VECTOR('',#18165,1000.);
#2656=VECTOR('',#18166,1000.);
#2657=VECTOR('',#18167,1000.);
#2658=VECTOR('',#18170,1000.);
#2659=VECTOR('',#18171,1000.);
#2660=VECTOR('',#18172,1000.);
#2661=VECTOR('',#18175,1000.);
#2662=VECTOR('',#18176,1000.);
#2663=VECTOR('',#18185,1000.);
#2664=VECTOR('',#18188,1000.);
#2665=VECTOR('',#18189,1000.);
#2666=VECTOR('',#18196,1000.);
#2667=VECTOR('',#18197,1000.);
#2668=VECTOR('',#18198,1000.);
#2669=VECTOR('',#18199,1000.);
#2670=VECTOR('',#18200,1000.);
#2671=VECTOR('',#18203,1000.);
#2672=VECTOR('',#18204,1000.);
#2673=VECTOR('',#18205,1000.);
#2674=VECTOR('',#18212,1000.);
#2675=VECTOR('',#18215,1000.);
#2676=VECTOR('',#18216,1000.);
#2677=VECTOR('',#18217,1000.);
#2678=VECTOR('',#18218,1000.);
#2679=VECTOR('',#18225,1000.);
#2680=VECTOR('',#18230,1000.);
#2681=VECTOR('',#18235,1000.);
#2682=VECTOR('',#18236,1000.);
#2683=VECTOR('',#18241,1000.);
#2684=VECTOR('',#18250,1000.);
#2685=VECTOR('',#18253,1000.);
#2686=VECTOR('',#18254,1000.);
#2687=VECTOR('',#18255,1000.);
#2688=VECTOR('',#18268,1000.);
#2689=VECTOR('',#18271,1000.);
#2690=VECTOR('',#18274,1000.);
#2691=VECTOR('',#18277,1000.);
#2692=VECTOR('',#18282,1000.);
#2693=VECTOR('',#18285,1000.);
#2694=VECTOR('',#18286,1000.);
#2695=VECTOR('',#18287,1000.);
#2696=VECTOR('',#18290,1000.);
#2697=VECTOR('',#18293,1000.);
#2698=VECTOR('',#18294,1000.);
#2699=VECTOR('',#18295,1000.);
#2700=VECTOR('',#18296,1000.);
#2701=VECTOR('',#18297,1000.);
#2702=VECTOR('',#18298,1000.);
#2703=VECTOR('',#18303,1000.);
#2704=VECTOR('',#18304,1000.);
#2705=VECTOR('',#18305,1000.);
#2706=VECTOR('',#18306,1000.);
#2707=VECTOR('',#18307,1000.);
#2708=VECTOR('',#18310,1000.);
#2709=VECTOR('',#18311,1000.);
#2710=VECTOR('',#18312,1000.);
#2711=VECTOR('',#18313,1000.);
#2712=VECTOR('',#18314,1000.);
#2713=VECTOR('',#18317,1000.);
#2714=VECTOR('',#18318,1000.);
#2715=VECTOR('',#18319,1000.);
#2716=VECTOR('',#18320,1000.);
#2717=VECTOR('',#18321,1000.);
#2718=VECTOR('',#18322,1000.);
#2719=VECTOR('',#18323,1000.);
#2720=VECTOR('',#18324,1000.);
#2721=VECTOR('',#18327,1000.);
#2722=VECTOR('',#18328,1000.);
#2723=VECTOR('',#18329,1000.);
#2724=VECTOR('',#18332,1000.);
#2725=VECTOR('',#18333,1000.);
#2726=VECTOR('',#18334,1000.);
#2727=VECTOR('',#18337,1000.);
#2728=VECTOR('',#18340,1000.);
#2729=VECTOR('',#18343,1000.);
#2730=VECTOR('',#18346,1000.);
#2731=VECTOR('',#18347,1000.);
#2732=VECTOR('',#18348,1000.);
#2733=VECTOR('',#18351,1000.);
#2734=VECTOR('',#18354,1000.);
#2735=VECTOR('',#18357,1000.);
#2736=VECTOR('',#18358,1000.);
#2737=VECTOR('',#18361,1000.);
#2738=VECTOR('',#18362,1000.);
#2739=VECTOR('',#18363,1000.);
#2740=VECTOR('',#18364,1000.);
#2741=VECTOR('',#18367,1000.);
#2742=VECTOR('',#18368,1000.);
#2743=VECTOR('',#18369,1000.);
#2744=VECTOR('',#18372,1000.);
#2745=VECTOR('',#18373,1000.);
#2746=VECTOR('',#18374,1000.);
#2747=VECTOR('',#18375,1000.);
#2748=VECTOR('',#18378,1000.);
#2749=VECTOR('',#18379,1000.);
#2750=VECTOR('',#18380,1000.);
#2751=VECTOR('',#18391,1000.);
#2752=VECTOR('',#18394,1000.);
#2753=VECTOR('',#18395,1000.);
#2754=VECTOR('',#18398,1000.);
#2755=VECTOR('',#18399,1000.);
#2756=VECTOR('',#18400,1000.);
#2757=VECTOR('',#18403,1000.);
#2758=VECTOR('',#18404,1000.);
#2759=VECTOR('',#18405,1000.);
#2760=VECTOR('',#18408,1000.);
#2761=VECTOR('',#18409,1000.);
#2762=VECTOR('',#18410,1000.);
#2763=VECTOR('',#18413,1000.);
#2764=VECTOR('',#18414,1000.);
#2765=VECTOR('',#18415,1000.);
#2766=VECTOR('',#18418,1000.);
#2767=VECTOR('',#18419,1000.);
#2768=VECTOR('',#18422,1000.);
#2769=VECTOR('',#18423,1000.);
#2770=VECTOR('',#18428,1000.);
#2771=VECTOR('',#18435,1000.);
#2772=VECTOR('',#18436,1000.);
#2773=VECTOR('',#18441,1000.);
#2774=VECTOR('',#18442,1000.);
#2775=VECTOR('',#18445,1000.);
#2776=VECTOR('',#18448,1000.);
#2777=VECTOR('',#18449,1000.);
#2778=VECTOR('',#18452,1000.);
#2779=VECTOR('',#18453,1000.);
#2780=VECTOR('',#18454,1000.);
#2781=VECTOR('',#18455,1000.);
#2782=VECTOR('',#18462,1000.);
#2783=VECTOR('',#18465,1000.);
#2784=VECTOR('',#18470,1000.);
#2785=VECTOR('',#18471,1000.);
#2786=VECTOR('',#18474,1000.);
#2787=VECTOR('',#18475,1000.);
#2788=VECTOR('',#18480,1000.);
#2789=VECTOR('',#18481,1000.);
#2790=VECTOR('',#18482,1000.);
#2791=VECTOR('',#18485,1000.);
#2792=VECTOR('',#18490,1000.);
#2793=VECTOR('',#18491,1000.);
#2794=VECTOR('',#18492,1000.);
#2795=VECTOR('',#18495,1000.);
#2796=VECTOR('',#18500,1000.);
#2797=VECTOR('',#18501,1000.);
#2798=VECTOR('',#18504,1000.);
#2799=VECTOR('',#18509,1000.);
#2800=VECTOR('',#18510,1000.);
#2801=VECTOR('',#18513,1000.);
#2802=VECTOR('',#18518,1000.);
#2803=VECTOR('',#18527,1000.);
#2804=VECTOR('',#18528,1000.);
#2805=VECTOR('',#18529,1000.);
#2806=VECTOR('',#18532,1000.);
#2807=VECTOR('',#18533,1000.);
#2808=VECTOR('',#18538,1000.);
#2809=VECTOR('',#18539,1000.);
#2810=VECTOR('',#18540,1000.);
#2811=VECTOR('',#18541,1000.);
#2812=VECTOR('',#18544,1000.);
#2813=VECTOR('',#18545,1000.);
#2814=VECTOR('',#18546,1000.);
#2815=VECTOR('',#18547,1000.);
#2816=VECTOR('',#18550,1000.);
#2817=VECTOR('',#18551,1000.);
#2818=VECTOR('',#18552,1000.);
#2819=VECTOR('',#18553,1000.);
#2820=VECTOR('',#18556,1000.);
#2821=VECTOR('',#18557,1000.);
#2822=VECTOR('',#18560,1000.);
#2823=VECTOR('',#18561,1000.);
#2824=VECTOR('',#18564,1000.);
#2825=VECTOR('',#18565,1000.);
#2826=VECTOR('',#18568,1000.);
#2827=VECTOR('',#18569,1000.);
#2828=VECTOR('',#18572,1000.);
#2829=VECTOR('',#18639,4.);
#2830=VECTOR('',#18648,4.);
#2831=VECTOR('',#18657,4.);
#2832=VECTOR('',#18662,2.8);
#2833=VECTOR('',#18665,1000.);
#2834=VECTOR('',#18668,1000.);
#2835=VECTOR('',#18671,1000.);
#2836=VECTOR('',#18674,1000.);
#2837=VECTOR('',#18683,2.5);
#2838=VECTOR('',#18686,1000.);
#2839=VECTOR('',#18687,1000.);
#2840=VECTOR('',#18690,1000.);
#2841=VECTOR('',#18693,1000.);
#2842=VECTOR('',#18718,1000.);
#2843=VECTOR('',#18721,1000.);
#2844=VECTOR('',#18730,1000.);
#2845=VECTOR('',#18733,1000.);
#2846=VECTOR('',#18736,1000.);
#2847=VECTOR('',#18767,1.5);
#2848=VECTOR('',#18776,1000.);
#2849=VECTOR('',#18779,1000.);
#2850=VECTOR('',#18780,1000.);
#2851=VECTOR('',#18783,1000.);
#2852=VECTOR('',#18786,1000.);
#2853=VECTOR('',#18791,1000.);
#2854=VECTOR('',#18798,1000.);
#2855=VECTOR('',#18815,1000.);
#2856=VECTOR('',#18818,1000.);
#2857=VECTOR('',#18821,1000.);
#2858=VECTOR('',#18824,1000.);
#2859=VECTOR('',#18827,1000.);
#2860=VECTOR('',#18828,1000.);
#2861=VECTOR('',#18831,1000.);
#2862=VECTOR('',#18836,1000.);
#2863=VECTOR('',#18865,0.8);
#2864=VECTOR('',#18868,0.8);
#2865=VECTOR('',#18875,1000.);
#2866=VECTOR('',#18876,1000.);
#2867=VECTOR('',#18879,1000.);
#2868=VECTOR('',#18880,1000.);
#2869=VECTOR('',#18881,1000.);
#2870=VECTOR('',#18884,1000.);
#2871=VECTOR('',#18885,1000.);
#2872=VECTOR('',#18886,1000.);
#2873=VECTOR('',#18889,1000.);
#2874=VECTOR('',#18890,1000.);
#2875=VECTOR('',#18891,1000.);
#2876=VECTOR('',#18894,1000.);
#2877=VECTOR('',#18895,1000.);
#2878=VECTOR('',#18896,1000.);
#2879=VECTOR('',#18897,1000.);
#2880=VECTOR('',#18900,1000.);
#2881=VECTOR('',#18901,1000.);
#2882=VECTOR('',#18902,1000.);
#2883=VECTOR('',#18903,1000.);
#2884=VECTOR('',#18906,1000.);
#2885=VECTOR('',#18907,1000.);
#2886=VECTOR('',#18908,1000.);
#2887=VECTOR('',#18909,1000.);
#2888=VECTOR('',#18912,1000.);
#2889=VECTOR('',#18915,1000.);
#2890=VECTOR('',#18918,1000.);
#2891=VECTOR('',#18927,1000.);
#2892=VECTOR('',#18930,1000.);
#2893=VECTOR('',#18933,1000.);
#2894=VECTOR('',#18936,1000.);
#2895=VECTOR('',#18955,1000.);
#2896=VECTOR('',#18956,1000.);
#2897=VECTOR('',#18961,1000.);
#2898=VECTOR('',#18962,1000.);
#2899=VECTOR('',#18963,1000.);
#2900=VECTOR('',#18972,1000.);
#2901=VECTOR('',#18975,1000.);
#2902=VECTOR('',#18980,1000.);
#2903=VECTOR('',#18981,1000.);
#2904=VECTOR('',#18984,1000.);
#2905=VECTOR('',#18985,1000.);
#2906=VECTOR('',#18986,1000.);
#2907=VECTOR('',#18987,1000.);
#2908=VECTOR('',#18988,1000.);
#2909=VECTOR('',#18991,1000.);
#2910=VECTOR('',#19000,1000.);
#2911=VECTOR('',#19003,1000.);
#2912=VECTOR('',#19006,1000.);
#2913=VECTOR('',#19009,1000.);
#2914=VECTOR('',#19012,1000.);
#2915=VECTOR('',#19013,1000.);
#2916=VECTOR('',#19022,1000.);
#2917=VECTOR('',#19031,1000.);
#2918=VECTOR('',#19036,1000.);
#2919=VECTOR('',#19041,1000.);
#2920=VECTOR('',#19068,1000.);
#2921=VECTOR('',#19079,1000.);
#2922=VECTOR('',#19082,1000.);
#2923=VECTOR('',#19087,1000.);
#2924=VECTOR('',#19088,1000.);
#2925=VECTOR('',#19089,1000.);
#2926=VECTOR('',#19104,1000.);
#2927=VECTOR('',#19111,1000.);
#2928=VECTOR('',#19116,1000.);
#2929=VECTOR('',#19117,1000.);
#2930=VECTOR('',#19120,1000.);
#2931=VECTOR('',#19123,1000.);
#2932=VECTOR('',#19124,1000.);
#2933=VECTOR('',#19125,1000.);
#2934=VECTOR('',#19126,1000.);
#2935=VECTOR('',#19129,1000.);
#2936=VECTOR('',#19130,1000.);
#2937=VECTOR('',#19131,1000.);
#2938=VECTOR('',#19132,1000.);
#2939=VECTOR('',#19133,1000.);
#2940=VECTOR('',#19134,1000.);
#2941=VECTOR('',#19139,1000.);
#2942=VECTOR('',#19146,1000.);
#2943=VECTOR('',#19161,1000.);
#2944=VECTOR('',#19180,1000.);
#2945=VECTOR('',#19183,1000.);
#2946=VECTOR('',#19186,1000.);
#2947=VECTOR('',#19187,1000.);
#2948=VECTOR('',#19190,1000.);
#2949=VECTOR('',#19201,1000.);
#2950=VECTOR('',#19212,1000.);
#2951=VECTOR('',#19217,1000.);
#2952=VECTOR('',#19220,1000.);
#2953=VECTOR('',#19225,1000.);
#2954=VECTOR('',#19228,1000.);
#2955=VECTOR('',#19233,1000.);
#2956=VECTOR('',#19236,1000.);
#2957=VECTOR('',#19239,1000.);
#2958=VECTOR('',#19240,1000.);
#2959=VECTOR('',#19241,1000.);
#2960=VECTOR('',#19274,1000.);
#2961=VECTOR('',#19283,1000.);
#2962=VECTOR('',#19290,1000.);
#2963=VECTOR('',#19291,1000.);
#2964=VECTOR('',#19306,1000.);
#2965=VECTOR('',#19307,1000.);
#2966=VECTOR('',#19338,1000.);
#2967=VECTOR('',#19339,1000.);
#2968=VECTOR('',#19342,1000.);
#2969=VECTOR('',#19387,1.1935);
#2970=VECTOR('',#19394,3.);
#2971=VECTOR('',#19401,1.5);
#2972=VECTOR('',#19406,1000.);
#2973=VECTOR('',#19407,1000.);
#2974=VECTOR('',#19408,1000.);
#2975=VECTOR('',#19411,1000.);
#2976=VECTOR('',#19412,1000.);
#2977=VECTOR('',#19415,1000.);
#2978=VECTOR('',#19416,1000.);
#2979=VECTOR('',#19419,1000.);
#2980=VECTOR('',#19420,1000.);
#2981=VECTOR('',#19423,1000.);
#2982=VECTOR('',#19424,1000.);
#2983=VECTOR('',#19427,1000.);
#2984=VECTOR('',#19428,1000.);
#2985=VECTOR('',#19431,1000.);
#2986=VECTOR('',#19432,1000.);
#2987=VECTOR('',#19435,1000.);
#2988=VECTOR('',#19436,1000.);
#2989=VECTOR('',#19439,1000.);
#2990=VECTOR('',#19440,1000.);
#2991=VECTOR('',#19443,1000.);
#2992=VECTOR('',#19444,1000.);
#2993=VECTOR('',#19447,1000.);
#2994=VECTOR('',#19448,1000.);
#2995=VECTOR('',#19451,1000.);
#2996=VECTOR('',#19460,4.5);
#2997=VECTOR('',#19463,1000.);
#2998=VECTOR('',#19466,4.5);
#2999=VECTOR('',#19471,1000.);
#3000=VECTOR('',#19476,4.5);
#3001=VECTOR('',#19479,1000.);
#3002=VECTOR('',#19484,1000.);
#3003=VECTOR('',#19489,4.5);
#3004=VECTOR('',#19492,1000.);
#3005=VECTOR('',#19495,4.5);
#3006=VECTOR('',#19498,1000.);
#3007=VECTOR('',#19503,1000.);
#3008=VECTOR('',#19508,1000.);
#3009=VECTOR('',#19515,4.5);
#3010=VECTOR('',#19518,1000.);
#3011=VECTOR('',#19521,4.5);
#3012=VECTOR('',#19524,1000.);
#3013=VECTOR('',#19529,5.5);
#3014=VECTOR('',#19532,1000.);
#3015=VECTOR('',#19535,1000.);
#3016=VECTOR('',#19538,1000.);
#3017=VECTOR('',#19543,5.5);
#3018=VECTOR('',#19546,1000.);
#3019=VECTOR('',#19549,1000.);
#3020=VECTOR('',#19552,1000.);
#3021=VECTOR('',#19559,2.);
#3022=VECTOR('',#19566,2.5);
#3023=VECTOR('',#19573,1.75);
#3024=VECTOR('',#19580,1000.);
#3025=VECTOR('',#19583,1000.);
#3026=VECTOR('',#19588,1000.);
#3027=VECTOR('',#19595,1000.);
#3028=VECTOR('',#19602,1000.);
#3029=VECTOR('',#19605,1000.);
#3030=VECTOR('',#19608,1000.);
#3031=VECTOR('',#19615,1000.);
#3032=VECTOR('',#19622,1000.);
#3033=VECTOR('',#19629,1000.);
#3034=VECTOR('',#19632,1000.);
#3035=VECTOR('',#19635,1000.);
#3036=VECTOR('',#19644,1000.);
#3037=VECTOR('',#19649,3.5);
#3038=VECTOR('',#19660,1000.);
#3039=VECTOR('',#19667,1000.);
#3040=VECTOR('',#19668,1000.);
#3041=VECTOR('',#19671,1000.);
#3042=VECTOR('',#19672,1000.);
#3043=VECTOR('',#19677,1000.);
#3044=VECTOR('',#19680,1000.);
#3045=VECTOR('',#19683,1000.);
#3046=VECTOR('',#19684,1000.);
#3047=VECTOR('',#19685,1000.);
#3048=VECTOR('',#19688,1000.);
#3049=VECTOR('',#19691,1000.);
#3050=VECTOR('',#19696,1000.);
#3051=VECTOR('',#19697,1000.);
#3052=VECTOR('',#19698,1000.);
#3053=VECTOR('',#19699,1000.);
#3054=VECTOR('',#19702,1000.);
#3055=VECTOR('',#19705,1000.);
#3056=VECTOR('',#19708,1000.);
#3057=VECTOR('',#19711,1000.);
#3058=VECTOR('',#19714,1000.);
#3059=VECTOR('',#19715,1000.);
#3060=VECTOR('',#19716,1000.);
#3061=VECTOR('',#19719,1000.);
#3062=VECTOR('',#19720,1000.);
#3063=VECTOR('',#19729,1000.);
#3064=VECTOR('',#19730,1000.);
#3065=VECTOR('',#19735,1000.);
#3066=VECTOR('',#19740,1000.);
#3067=VECTOR('',#19741,1000.);
#3068=VECTOR('',#19742,1000.);
#3069=VECTOR('',#19747,1000.);
#3070=VECTOR('',#19748,1000.);
#3071=VECTOR('',#19749,1000.);
#3072=VECTOR('',#19752,1000.);
#3073=VECTOR('',#19753,1000.);
#3074=VECTOR('',#19754,1000.);
#3075=VECTOR('',#19757,1000.);
#3076=VECTOR('',#19762,1000.);
#3077=VECTOR('',#19769,1000.);
#3078=VECTOR('',#19770,1000.);
#3079=VECTOR('',#19775,1000.);
#3080=VECTOR('',#19778,1000.);
#3081=VECTOR('',#19781,1000.);
#3082=VECTOR('',#19782,1000.);
#3083=VECTOR('',#19783,1000.);
#3084=VECTOR('',#19788,1000.);
#3085=VECTOR('',#19789,1000.);
#3086=VECTOR('',#19790,1000.);
#3087=VECTOR('',#19791,1000.);
#3088=VECTOR('',#19792,1000.);
#3089=VECTOR('',#19795,1000.);
#3090=VECTOR('',#19796,1000.);
#3091=VECTOR('',#19797,1000.);
#3092=VECTOR('',#19800,1000.);
#3093=VECTOR('',#19803,1000.);
#3094=VECTOR('',#19806,1000.);
#3095=VECTOR('',#19807,1000.);
#3096=VECTOR('',#19810,1000.);
#3097=VECTOR('',#19811,1000.);
#3098=VECTOR('',#19814,1000.);
#3099=VECTOR('',#19821,1000.);
#3100=VECTOR('',#19822,1000.);
#3101=VECTOR('',#19825,1000.);
#3102=VECTOR('',#19826,1000.);
#3103=VECTOR('',#19831,1000.);
#3104=VECTOR('',#19834,1000.);
#3105=VECTOR('',#19837,1000.);
#3106=VECTOR('',#19838,1000.);
#3107=VECTOR('',#19839,1000.);
#3108=VECTOR('',#19842,1000.);
#3109=VECTOR('',#19845,1000.);
#3110=VECTOR('',#19850,1000.);
#3111=VECTOR('',#19853,1000.);
#3112=VECTOR('',#19856,1000.);
#3113=VECTOR('',#19861,1000.);
#3114=VECTOR('',#19862,1000.);
#3115=VECTOR('',#19879,1000.);
#3116=VECTOR('',#19880,1000.);
#3117=VECTOR('',#19881,1000.);
#3118=VECTOR('',#19882,1000.);
#3119=VECTOR('',#19885,1000.);
#3120=VECTOR('',#19886,1000.);
#3121=VECTOR('',#19887,1000.);
#3122=VECTOR('',#19890,1000.);
#3123=VECTOR('',#19891,1000.);
#3124=VECTOR('',#19892,1000.);
#3125=VECTOR('',#19893,1000.);
#3126=VECTOR('',#19898,1000.);
#3127=VECTOR('',#19903,1000.);
#3128=VECTOR('',#19904,1000.);
#3129=VECTOR('',#19905,1000.);
#3130=VECTOR('',#19910,1000.);
#3131=VECTOR('',#19915,1000.);
#3132=VECTOR('',#19916,1000.);
#3133=VECTOR('',#19917,1000.);
#3134=VECTOR('',#19922,1000.);
#3135=VECTOR('',#19927,1000.);
#3136=VECTOR('',#19932,1000.);
#3137=VECTOR('',#19935,1000.);
#3138=VECTOR('',#19936,1000.);
#3139=VECTOR('',#19939,1000.);
#3140=VECTOR('',#19942,1000.);
#3141=VECTOR('',#19943,1000.);
#3142=VECTOR('',#19946,1000.);
#3143=VECTOR('',#19955,14.5);
#3144=VECTOR('',#19958,14.5);
#3145=VECTOR('',#19965,1000.);
#3146=VECTOR('',#19968,1000.);
#3147=VECTOR('',#19973,1000.);
#3148=VECTOR('',#19976,1000.);
#3149=VECTOR('',#19979,2.5);
#3150=VECTOR('',#19986,2.4585);
#3151=VECTOR('',#19993,6.5);
#3152=VECTOR('',#19998,1.62099999999999);
#3153=VECTOR('',#20005,2.4585);
#3154=VECTOR('',#20012,3.5);
#3155=VECTOR('',#20019,3.50000000000384);
#3156=VECTOR('',#20026,1000.);
#3157=VECTOR('',#20029,1000.);
#3158=VECTOR('',#20034,2.5);
#3159=VECTOR('',#20041,1.6);
#3160=VECTOR('',#20046,2.5);
#3161=VECTOR('',#20053,1.75);
#3162=VECTOR('',#20064,1000.);
#3163=VECTOR('',#20065,1000.);
#3164=VECTOR('',#20066,1000.);
#3165=VECTOR('',#20069,1000.);
#3166=VECTOR('',#20070,1000.);
#3167=VECTOR('',#20071,1000.);
#3168=VECTOR('',#20072,1000.);
#3169=VECTOR('',#20075,1000.);
#3170=VECTOR('',#20076,1000.);
#3171=VECTOR('',#20077,1000.);
#3172=VECTOR('',#20080,1000.);
#3173=VECTOR('',#20081,1000.);
#3174=VECTOR('',#20082,1000.);
#3175=VECTOR('',#20083,1000.);
#3176=VECTOR('',#20086,1000.);
#3177=VECTOR('',#20087,1000.);
#3178=VECTOR('',#20088,1000.);
#3179=VECTOR('',#20091,1000.);
#3180=VECTOR('',#20092,1000.);
#3181=VECTOR('',#20093,1000.);
#3182=VECTOR('',#20100,1000.);
#3183=VECTOR('',#20103,1000.);
#3184=VECTOR('',#20104,1000.);
#3185=VECTOR('',#20105,1000.);
#3186=VECTOR('',#20112,1000.);
#3187=VECTOR('',#20115,1000.);
#3188=VECTOR('',#20116,1000.);
#3189=VECTOR('',#20117,1000.);
#3190=VECTOR('',#20120,1000.);
#3191=VECTOR('',#20129,1000.);
#3192=VECTOR('',#20132,1000.);
#3193=VECTOR('',#20135,1000.);
#3194=VECTOR('',#20136,1000.);
#3195=VECTOR('',#20137,1000.);
#3196=VECTOR('',#20138,1000.);
#3197=VECTOR('',#20141,1000.);
#3198=VECTOR('',#20142,1000.);
#3199=VECTOR('',#20143,1000.);
#3200=VECTOR('',#20144,1000.);
#3201=VECTOR('',#20147,1000.);
#3202=VECTOR('',#20148,1000.);
#3203=VECTOR('',#20151,1000.);
#3204=VECTOR('',#20152,1000.);
#3205=VECTOR('',#20153,1000.);
#3206=VECTOR('',#20156,1000.);
#3207=VECTOR('',#20157,1000.);
#3208=VECTOR('',#20158,1000.);
#3209=VECTOR('',#20159,1000.);
#3210=VECTOR('',#20160,1000.);
#3211=VECTOR('',#20163,1000.);
#3212=VECTOR('',#20164,1000.);
#3213=VECTOR('',#20165,1000.);
#3214=VECTOR('',#20166,1000.);
#3215=VECTOR('',#20173,1000.);
#3216=VECTOR('',#20174,1000.);
#3217=VECTOR('',#20175,1000.);
#3218=VECTOR('',#20176,1000.);
#3219=VECTOR('',#20183,1000.);
#3220=VECTOR('',#20192,1000.);
#3221=VECTOR('',#20195,1000.);
#3222=VECTOR('',#20196,1000.);
#3223=VECTOR('',#20199,1000.);
#3224=VECTOR('',#20200,1000.);
#3225=VECTOR('',#20201,1000.);
#3226=VECTOR('',#20202,1000.);
#3227=VECTOR('',#20205,1000.);
#3228=VECTOR('',#20206,1000.);
#3229=VECTOR('',#20209,1000.);
#3230=VECTOR('',#20212,1000.);
#3231=VECTOR('',#20219,1000.);
#3232=VECTOR('',#20224,1000.);
#3233=VECTOR('',#20225,1000.);
#3234=VECTOR('',#20230,1000.);
#3235=VECTOR('',#20235,1000.);
#3236=VECTOR('',#20238,1000.);
#3237=VECTOR('',#20263,19.5);
#3238=VECTOR('',#20268,3.);
#3239=VECTOR('',#20283,19.5);
#3240=VECTOR('',#20302,16.5);
#3241=VECTOR('',#20309,1000.);
#3242=VECTOR('',#20322,1000.);
#3243=VECTOR('',#20325,1000.);
#3244=VECTOR('',#20338,1000.);
#3245=VECTOR('',#20341,1000.);
#3246=VECTOR('',#20374,8.);
#3247=VECTOR('',#20379,1000.);
#3248=VECTOR('',#20382,1000.);
#3249=VECTOR('',#20395,14.5);
#3250=VECTOR('',#20418,1000.);
#3251=VECTOR('',#20421,1000.);
#3252=VECTOR('',#20424,1000.);
#3253=VECTOR('',#20427,1000.);
#3254=VECTOR('',#20430,19.5);
#3255=VECTOR('',#20437,1000.);
#3256=VECTOR('',#20440,1000.);
#3257=VECTOR('',#20451,5.);
#3258=VECTOR('',#20462,2.);
#3259=VECTOR('',#20469,2.2295);
#3260=VECTOR('',#20476,17.5);
#3261=VECTOR('',#20491,1000.);
#3262=VECTOR('',#20494,1000.);
#3263=VECTOR('',#20499,1000.);
#3264=VECTOR('',#20502,1000.);
#3265=VECTOR('',#20513,1000.);
#3266=VECTOR('',#20514,1000.);
#3267=VECTOR('',#20525,3.3235);
#3268=VECTOR('',#20530,1000.);
#3269=VECTOR('',#20533,1000.);
#3270=VECTOR('',#20538,1000.);
#3271=VECTOR('',#20539,1000.);
#3272=VECTOR('',#20544,4.);
#3273=VECTOR('',#20547,4.);
#3274=VECTOR('',#20552,1000.);
#3275=VECTOR('',#20555,1000.);
#3276=VECTOR('',#20560,2.5);
#3277=VECTOR('',#20565,1000.);
#3278=VECTOR('',#20572,2.067);
#3279=VECTOR('',#20583,17.4363291775691);
#3280=VECTOR('',#20594,2.5);
#3281=VECTOR('',#20601,2.);
#3282=VECTOR('',#20612,1000.);
#3283=VECTOR('',#20617,1000.);
#3284=VECTOR('',#20622,1000.);
#3285=VECTOR('',#20623,1000.);
#3286=VECTOR('',#20624,1000.);
#3287=VECTOR('',#20627,1000.);
#3288=VECTOR('',#20636,1000.);
#3289=VECTOR('',#20637,1000.);
#3290=VECTOR('',#20640,1000.);
#3291=VECTOR('',#20643,1000.);
#3292=VECTOR('',#20644,1000.);
#3293=VECTOR('',#20647,1000.);
#3294=VECTOR('',#20652,1000.);
#3295=VECTOR('',#20653,1000.);
#3296=VECTOR('',#20656,1000.);
#3297=VECTOR('',#20661,1000.);
#3298=VECTOR('',#20700,1000.);
#3299=VECTOR('',#20701,1000.);
#3300=VECTOR('',#20706,1000.);
#3301=VECTOR('',#20707,1000.);
#3302=VECTOR('',#20720,1000.);
#3303=VECTOR('',#20721,1000.);
#3304=VECTOR('',#20726,1000.);
#3305=VECTOR('',#20727,1000.);
#3306=VECTOR('',#20738,1000.);
#3307=VECTOR('',#20739,1000.);
#3308=VECTOR('',#20744,1000.);
#3309=VECTOR('',#20745,1000.);
#3310=VECTOR('',#20756,1000.);
#3311=VECTOR('',#20757,1000.);
#3312=VECTOR('',#20760,1000.);
#3313=VECTOR('',#20763,1000.);
#3314=VECTOR('',#20774,1000.);
#3315=VECTOR('',#20775,1000.);
#3316=VECTOR('',#20780,1000.);
#3317=VECTOR('',#20783,1000.);
#3318=VECTOR('',#20792,1000.);
#3319=VECTOR('',#20793,1000.);
#3320=VECTOR('',#20796,1000.);
#3321=VECTOR('',#20799,1000.);
#3322=VECTOR('',#20804,1000.);
#3323=VECTOR('',#20805,1000.);
#3324=VECTOR('',#20812,1000.);
#3325=VECTOR('',#20813,1000.);
#3326=VECTOR('',#20816,1000.);
#3327=VECTOR('',#20819,1000.);
#3328=VECTOR('',#20824,1000.);
#3329=VECTOR('',#20827,1000.);
#3330=VECTOR('',#20838,1000.);
#3331=VECTOR('',#20839,1000.);
#3332=VECTOR('',#20842,1000.);
#3333=VECTOR('',#20843,1000.);
#3334=VECTOR('',#20846,1000.);
#3335=VECTOR('',#20847,1000.);
#3336=VECTOR('',#20850,1000.);
#3337=VECTOR('',#20853,1000.);
#3338=VECTOR('',#20856,1000.);
#3339=VECTOR('',#20859,1000.);
#3340=VECTOR('',#20860,1000.);
#3341=VECTOR('',#20861,1000.);
#3342=VECTOR('',#20862,1000.);
#3343=VECTOR('',#20867,1000.);
#3344=VECTOR('',#20868,1000.);
#3345=VECTOR('',#20869,1000.);
#3346=VECTOR('',#20872,1000.);
#3347=VECTOR('',#20875,1000.);
#3348=VECTOR('',#20878,1000.);
#3349=VECTOR('',#20879,1000.);
#3350=VECTOR('',#20886,1000.);
#3351=VECTOR('',#20887,1000.);
#3352=VECTOR('',#20894,1000.);
#3353=VECTOR('',#20895,1000.);
#3354=VECTOR('',#20896,1000.);
#3355=VECTOR('',#20899,1000.);
#3356=VECTOR('',#20900,1000.);
#3357=VECTOR('',#20923,1000.);
#3358=VECTOR('',#20942,1000.);
#3359=VECTOR('',#20945,1000.);
#3360=VECTOR('',#20948,1000.);
#3361=VECTOR('',#20953,1000.);
#3362=VECTOR('',#20954,1000.);
#3363=VECTOR('',#20959,1000.);
#3364=VECTOR('',#20962,1000.);
#3365=VECTOR('',#20965,1000.);
#3366=VECTOR('',#20966,1000.);
#3367=VECTOR('',#20973,1000.);
#3368=VECTOR('',#20974,1000.);
#3369=VECTOR('',#20983,1000.);
#3370=VECTOR('',#20984,1000.);
#3371=VECTOR('',#20989,1000.);
#3372=VECTOR('',#20996,1000.);
#3373=VECTOR('',#21001,1000.);
#3374=VECTOR('',#21002,1000.);
#3375=VECTOR('',#21003,1000.);
#3376=VECTOR('',#21006,1000.);
#3377=VECTOR('',#21007,1000.);
#3378=VECTOR('',#21008,1000.);
#3379=VECTOR('',#21011,1000.);
#3380=VECTOR('',#21012,1000.);
#3381=VECTOR('',#21013,1000.);
#3382=VECTOR('',#21016,1000.);
#3383=VECTOR('',#21025,1000.);
#3384=VECTOR('',#21026,1000.);
#3385=VECTOR('',#21027,1000.);
#3386=VECTOR('',#21034,1000.);
#3387=VECTOR('',#21041,1000.);
#3388=VECTOR('',#21044,1000.);
#3389=VECTOR('',#21049,1000.);
#3390=VECTOR('',#21050,1000.);
#3391=VECTOR('',#21051,1000.);
#3392=VECTOR('',#21054,1000.);
#3393=VECTOR('',#21055,1000.);
#3394=VECTOR('',#21084,1000.);
#3395=VECTOR('',#21127,1000.);
#3396=VECTOR('',#21132,1000.);
#3397=VECTOR('',#21135,1000.);
#3398=VECTOR('',#21148,3.5);
#3399=VECTOR('',#21155,1.6);
#3400=VECTOR('',#21190,1000.);
#3401=VECTOR('',#21191,1000.);
#3402=VECTOR('',#21194,1000.);
#3403=VECTOR('',#21195,1000.);
#3404=VECTOR('',#21198,1000.);
#3405=VECTOR('',#21199,1000.);
#3406=VECTOR('',#21202,1000.);
#3407=VECTOR('',#21203,1000.);
#3408=VECTOR('',#21212,2.5);
#3409=VECTOR('',#21241,5.);
#3410=VECTOR('',#21256,3.);
#3411=VECTOR('',#21271,3.);
#3412=VECTOR('',#21276,3.0139499546386);
#3413=VECTOR('',#21293,1000.);
#3414=VECTOR('',#21294,1000.);
#3415=VECTOR('',#21305,1000.);
#3416=VECTOR('',#21306,1000.);
#3417=VECTOR('',#21309,1000.);
#3418=VECTOR('',#21310,1000.);
#3419=VECTOR('',#21315,1000.);
#3420=VECTOR('',#21316,1000.);
#3421=VECTOR('',#21317,1000.);
#3422=VECTOR('',#21318,1000.);
#3423=VECTOR('',#21321,1000.);
#3424=VECTOR('',#21322,1000.);
#3425=VECTOR('',#21323,1000.);
#3426=VECTOR('',#21326,1000.);
#3427=VECTOR('',#21327,1000.);
#3428=VECTOR('',#21328,1000.);
#3429=VECTOR('',#21329,1000.);
#3430=VECTOR('',#21332,1000.);
#3431=VECTOR('',#21333,1000.);
#3432=VECTOR('',#21334,1000.);
#3433=VECTOR('',#21335,1000.);
#3434=VECTOR('',#21336,1000.);
#3435=VECTOR('',#21339,1000.);
#3436=VECTOR('',#21340,1000.);
#3437=VECTOR('',#21341,1000.);
#3438=VECTOR('',#21342,1000.);
#3439=VECTOR('',#21345,1000.);
#3440=VECTOR('',#21346,1000.);
#3441=VECTOR('',#21347,1000.);
#3442=VECTOR('',#21348,1000.);
#3443=CYLINDRICAL_SURFACE('',#15343,6.25);
#3444=CYLINDRICAL_SURFACE('',#15345,6.25);
#3445=CYLINDRICAL_SURFACE('',#15347,2.25);
#3446=CYLINDRICAL_SURFACE('',#15350,3.);
#3447=CYLINDRICAL_SURFACE('',#15357,10.0000000011845);
#3448=CYLINDRICAL_SURFACE('',#15360,5.25);
#3449=CYLINDRICAL_SURFACE('',#15366,4.);
#3450=CYLINDRICAL_SURFACE('',#15369,5.25);
#3451=CYLINDRICAL_SURFACE('',#15373,5.04017795657138);
#3452=CYLINDRICAL_SURFACE('',#15378,0.300000000000003);
#3453=CYLINDRICAL_SURFACE('',#15381,0.300000000000003);
#3454=CYLINDRICAL_SURFACE('',#15384,4.);
#3455=CYLINDRICAL_SURFACE('',#15391,4.2);
#3456=CYLINDRICAL_SURFACE('',#15396,5.8);
#3457=CYLINDRICAL_SURFACE('',#15445,5.);
#3458=CYLINDRICAL_SURFACE('',#15449,10.0000000011845);
#3459=CYLINDRICAL_SURFACE('',#15472,4.);
#3460=CYLINDRICAL_SURFACE('',#15506,2.);
#3461=CYLINDRICAL_SURFACE('',#15538,3.);
#3462=CYLINDRICAL_SURFACE('',#15566,4.);
#3463=CYLINDRICAL_SURFACE('',#15601,3.);
#3464=CYLINDRICAL_SURFACE('',#15680,9.6875);
#3465=CYLINDRICAL_SURFACE('',#15685,2.067);
#3466=CYLINDRICAL_SURFACE('',#15688,5.);
#3467=CYLINDRICAL_SURFACE('',#15691,9.);
#3468=CYLINDRICAL_SURFACE('',#15694,9.);
#3469=CYLINDRICAL_SURFACE('',#15750,9.);
#3470=CYLINDRICAL_SURFACE('',#15754,9.);
#3471=CYLINDRICAL_SURFACE('',#15757,9.);
#3472=CYLINDRICAL_SURFACE('',#15761,0.5);
#3473=CYLINDRICAL_SURFACE('',#15764,0.5);
#3474=CYLINDRICAL_SURFACE('',#15768,0.5);
#3475=CYLINDRICAL_SURFACE('',#15771,0.5);
#3476=CYLINDRICAL_SURFACE('',#15799,3.5);
#3477=CYLINDRICAL_SURFACE('',#15802,3.5);
#3478=CYLINDRICAL_SURFACE('',#15812,2.);
#3479=CYLINDRICAL_SURFACE('',#15814,2.);
#3480=CYLINDRICAL_SURFACE('',#15824,0.799999999999998);
#3481=CYLINDRICAL_SURFACE('',#15826,0.799999999999998);
#3482=CYLINDRICAL_SURFACE('',#15833,2.5);
#3483=CYLINDRICAL_SURFACE('',#15836,2.5);
#3484=CYLINDRICAL_SURFACE('',#15839,2.5);
#3485=CYLINDRICAL_SURFACE('',#15841,2.5);
#3486=CYLINDRICAL_SURFACE('',#15887,4.);
#3487=CYLINDRICAL_SURFACE('',#15894,4.);
#3488=CYLINDRICAL_SURFACE('',#15897,2.8);
#3489=CYLINDRICAL_SURFACE('',#15905,2.5);
#3490=CYLINDRICAL_SURFACE('',#15920,17.);
#3491=CYLINDRICAL_SURFACE('',#15923,17.);
#3492=CYLINDRICAL_SURFACE('',#15942,1.5);
#3493=CYLINDRICAL_SURFACE('',#15945,3.8);
#3494=CYLINDRICAL_SURFACE('',#15950,0.499999999999999);
#3495=CYLINDRICAL_SURFACE('',#15953,1.);
#3496=CYLINDRICAL_SURFACE('',#15961,2.5);
#3497=CYLINDRICAL_SURFACE('',#15968,0.500000000000002);
#3498=CYLINDRICAL_SURFACE('',#15984,0.8);
#3499=CYLINDRICAL_SURFACE('',#15985,0.8);
#3500=CYLINDRICAL_SURFACE('',#15988,6.);
#3501=CYLINDRICAL_SURFACE('',#15996,0.5);
#3502=CYLINDRICAL_SURFACE('',#15997,0.5);
#3503=CYLINDRICAL_SURFACE('',#16001,0.5);
#3504=CYLINDRICAL_SURFACE('',#16002,0.5);
#3505=CYLINDRICAL_SURFACE('',#16003,0.5);
#3506=CYLINDRICAL_SURFACE('',#16004,0.5);
#3507=CYLINDRICAL_SURFACE('',#16013,0.5);
#3508=CYLINDRICAL_SURFACE('',#16019,0.5);
#3509=CYLINDRICAL_SURFACE('',#16036,0.5);
#3510=CYLINDRICAL_SURFACE('',#16040,0.500000000000002);
#3511=CYLINDRICAL_SURFACE('',#16041,0.5);
#3512=CYLINDRICAL_SURFACE('',#16044,0.5);
#3513=CYLINDRICAL_SURFACE('',#16057,0.5);
#3514=CYLINDRICAL_SURFACE('',#16062,10.5);
#3515=CYLINDRICAL_SURFACE('',#16069,1.);
#3516=CYLINDRICAL_SURFACE('',#16072,1.);
#3517=CYLINDRICAL_SURFACE('',#16075,1.);
#3518=CYLINDRICAL_SURFACE('',#16081,0.5);
#3519=CYLINDRICAL_SURFACE('',#16085,0.499999999999999);
#3520=CYLINDRICAL_SURFACE('',#16092,0.5);
#3521=CYLINDRICAL_SURFACE('',#16093,3.8);
#3522=CYLINDRICAL_SURFACE('',#16111,10.5);
#3523=CYLINDRICAL_SURFACE('',#16113,10.5);
#3524=CYLINDRICAL_SURFACE('',#16125,6.);
#3525=CYLINDRICAL_SURFACE('',#16128,10.5);
#3526=CYLINDRICAL_SURFACE('',#16129,6.);
#3527=CYLINDRICAL_SURFACE('',#16132,6.);
#3528=CYLINDRICAL_SURFACE('',#16135,0.5);
#3529=CYLINDRICAL_SURFACE('',#16136,0.5);
#3530=CYLINDRICAL_SURFACE('',#16137,0.5);
#3531=CYLINDRICAL_SURFACE('',#16139,0.5);
#3532=CYLINDRICAL_SURFACE('',#16141,1.);
#3533=CYLINDRICAL_SURFACE('',#16143,1.);
#3534=CYLINDRICAL_SURFACE('',#16144,0.5);
#3535=CYLINDRICAL_SURFACE('',#16149,0.5);
#3536=CYLINDRICAL_SURFACE('',#16152,0.5);
#3537=CYLINDRICAL_SURFACE('',#16153,4.5);
#3538=CYLINDRICAL_SURFACE('',#16156,0.5);
#3539=CYLINDRICAL_SURFACE('',#16157,0.5);
#3540=CYLINDRICAL_SURFACE('',#16161,0.5);
#3541=CYLINDRICAL_SURFACE('',#16162,0.5);
#3542=CYLINDRICAL_SURFACE('',#16164,0.5);
#3543=CYLINDRICAL_SURFACE('',#16165,13.5);
#3544=CYLINDRICAL_SURFACE('',#16172,0.499999999999999);
#3545=CYLINDRICAL_SURFACE('',#16195,3.);
#3546=CYLINDRICAL_SURFACE('',#16197,1.5);
#3547=CYLINDRICAL_SURFACE('',#16215,4.5);
#3548=CYLINDRICAL_SURFACE('',#16221,4.5);
#3549=CYLINDRICAL_SURFACE('',#16226,4.5);
#3550=CYLINDRICAL_SURFACE('',#16235,4.5);
#3551=CYLINDRICAL_SURFACE('',#16241,5.5);
#3552=CYLINDRICAL_SURFACE('',#16246,5.5);
#3553=CYLINDRICAL_SURFACE('',#16251,2.);
#3554=CYLINDRICAL_SURFACE('',#16254,2.5);
#3555=CYLINDRICAL_SURFACE('',#16257,1.75);
#3556=CYLINDRICAL_SURFACE('',#16260,1.);
#3557=CYLINDRICAL_SURFACE('',#16263,1.);
#3558=CYLINDRICAL_SURFACE('',#16266,1.);
#3559=CYLINDRICAL_SURFACE('',#16269,5.5);
#3560=CYLINDRICAL_SURFACE('',#16274,1.);
#3561=CYLINDRICAL_SURFACE('',#16277,1.);
#3562=CYLINDRICAL_SURFACE('',#16280,5.5);
#3563=CYLINDRICAL_SURFACE('',#16285,1.);
#3564=CYLINDRICAL_SURFACE('',#16288,3.5);
#3565=CYLINDRICAL_SURFACE('',#16291,4.5);
#3566=CYLINDRICAL_SURFACE('',#16299,0.5);
#3567=CYLINDRICAL_SURFACE('',#16305,0.500000000000001);
#3568=CYLINDRICAL_SURFACE('',#16307,0.5);
#3569=CYLINDRICAL_SURFACE('',#16309,0.500000000000001);
#3570=CYLINDRICAL_SURFACE('',#16310,0.500000000000001);
#3571=CYLINDRICAL_SURFACE('',#16314,0.500000000000001);
#3572=CYLINDRICAL_SURFACE('',#16317,0.5);
#3573=CYLINDRICAL_SURFACE('',#16328,0.5);
#3574=CYLINDRICAL_SURFACE('',#16330,0.5);
#3575=CYLINDRICAL_SURFACE('',#16343,0.5);
#3576=CYLINDRICAL_SURFACE('',#16346,0.5);
#3577=CYLINDRICAL_SURFACE('',#16352,0.5);
#3578=CYLINDRICAL_SURFACE('',#16353,0.5);
#3579=CYLINDRICAL_SURFACE('',#16355,0.5);
#3580=CYLINDRICAL_SURFACE('',#16356,0.5);
#3581=CYLINDRICAL_SURFACE('',#16359,0.5);
#3582=CYLINDRICAL_SURFACE('',#16368,0.500000000000002);
#3583=CYLINDRICAL_SURFACE('',#16372,0.500000000000002);
#3584=CYLINDRICAL_SURFACE('',#16379,0.500000000000002);
#3585=CYLINDRICAL_SURFACE('',#16387,0.500000000000002);
#3586=CYLINDRICAL_SURFACE('',#16392,5.);
#3587=CYLINDRICAL_SURFACE('',#16395,5.5);
#3588=CYLINDRICAL_SURFACE('',#16398,2.5);
#3589=CYLINDRICAL_SURFACE('',#16400,2.4585);
#3590=CYLINDRICAL_SURFACE('',#16403,6.5);
#3591=CYLINDRICAL_SURFACE('',#16405,1.62099999999999);
#3592=CYLINDRICAL_SURFACE('',#16408,2.4585);
#3593=CYLINDRICAL_SURFACE('',#16411,3.5);
#3594=CYLINDRICAL_SURFACE('',#16414,3.50000000000384);
#3595=CYLINDRICAL_SURFACE('',#16417,7.);
#3596=CYLINDRICAL_SURFACE('',#16423,1.6);
#3597=CYLINDRICAL_SURFACE('',#16426,2.5);
#3598=CYLINDRICAL_SURFACE('',#16428,1.75);
#3599=CYLINDRICAL_SURFACE('',#16440,21.);
#3600=CYLINDRICAL_SURFACE('',#16444,5.5);
#3601=CYLINDRICAL_SURFACE('',#16448,21.);
#3602=CYLINDRICAL_SURFACE('',#16451,5.);
#3603=CYLINDRICAL_SURFACE('',#16467,19.);
#3604=CYLINDRICAL_SURFACE('',#16478,7.00000000000384);
#3605=CYLINDRICAL_SURFACE('',#16487,19.);
#3606=CYLINDRICAL_SURFACE('',#16495,19.5);
#3607=CYLINDRICAL_SURFACE('',#16513,16.5);
#3608=CYLINDRICAL_SURFACE('',#16530,5.);
#3609=CYLINDRICAL_SURFACE('',#16546,8.);
#3610=CYLINDRICAL_SURFACE('',#16549,9.);
#3611=CYLINDRICAL_SURFACE('',#16555,14.5);
#3612=CYLINDRICAL_SURFACE('',#16566,2.9);
#3613=CYLINDRICAL_SURFACE('',#16569,0.5);
#3614=CYLINDRICAL_SURFACE('',#16571,19.5);
#3615=CYLINDRICAL_SURFACE('',#16573,6.5);
#3616=CYLINDRICAL_SURFACE('',#16576,5.);
#3617=CYLINDRICAL_SURFACE('',#16579,5.);
#3618=CYLINDRICAL_SURFACE('',#16582,2.);
#3619=CYLINDRICAL_SURFACE('',#16587,2.2295);
#3620=CYLINDRICAL_SURFACE('',#16590,17.5);
#3621=CYLINDRICAL_SURFACE('',#16597,0.5);
#3622=CYLINDRICAL_SURFACE('',#16600,0.499999999999999);
#3623=CYLINDRICAL_SURFACE('',#16606,0.5);
#3624=CYLINDRICAL_SURFACE('',#16611,3.3235);
#3625=CYLINDRICAL_SURFACE('',#16614,0.5);
#3626=CYLINDRICAL_SURFACE('',#16616,0.5);
#3627=CYLINDRICAL_SURFACE('',#16618,4.);
#3628=CYLINDRICAL_SURFACE('',#16620,4.);
#3629=CYLINDRICAL_SURFACE('',#16622,5.5);
#3630=CYLINDRICAL_SURFACE('',#16624,2.5);
#3631=CYLINDRICAL_SURFACE('',#16627,0.5);
#3632=CYLINDRICAL_SURFACE('',#16629,2.067);
#3633=CYLINDRICAL_SURFACE('',#16639,2.5);
#3634=CYLINDRICAL_SURFACE('',#16642,2.);
#3635=CYLINDRICAL_SURFACE('',#16648,0.5);
#3636=CYLINDRICAL_SURFACE('',#16650,0.5);
#3637=CYLINDRICAL_SURFACE('',#16653,21.);
#3638=CYLINDRICAL_SURFACE('',#16660,5.5);
#3639=CYLINDRICAL_SURFACE('',#16663,21.);
#3640=CYLINDRICAL_SURFACE('',#16684,0.5);
#3641=CYLINDRICAL_SURFACE('',#16685,0.499999999999998);
#3642=CYLINDRICAL_SURFACE('',#16691,0.5);
#3643=CYLINDRICAL_SURFACE('',#16693,0.5);
#3644=CYLINDRICAL_SURFACE('',#16698,0.5);
#3645=CYLINDRICAL_SURFACE('',#16700,0.5);
#3646=CYLINDRICAL_SURFACE('',#16705,0.5);
#3647=CYLINDRICAL_SURFACE('',#16707,0.499999999999998);
#3648=CYLINDRICAL_SURFACE('',#16713,0.499999999999998);
#3649=CYLINDRICAL_SURFACE('',#16714,0.499999999999998);
#3650=CYLINDRICAL_SURFACE('',#16720,0.5);
#3651=CYLINDRICAL_SURFACE('',#16721,0.499999999999999);
#3652=CYLINDRICAL_SURFACE('',#16723,0.5);
#3653=CYLINDRICAL_SURFACE('',#16727,0.5);
#3654=CYLINDRICAL_SURFACE('',#16728,0.499999999999998);
#3655=CYLINDRICAL_SURFACE('',#16731,0.5);
#3656=CYLINDRICAL_SURFACE('',#16736,0.499999999999999);
#3657=CYLINDRICAL_SURFACE('',#16738,0.499999999999999);
#3658=CYLINDRICAL_SURFACE('',#16739,0.5);
#3659=CYLINDRICAL_SURFACE('',#16740,0.5);
#3660=CYLINDRICAL_SURFACE('',#16752,5.);
#3661=CYLINDRICAL_SURFACE('',#16757,5.);
#3662=CYLINDRICAL_SURFACE('',#16775,0.5);
#3663=CYLINDRICAL_SURFACE('',#16777,0.499999999999998);
#3664=CYLINDRICAL_SURFACE('',#16781,0.5);
#3665=CYLINDRICAL_SURFACE('',#16783,0.5);
#3666=CYLINDRICAL_SURFACE('',#16785,5.);
#3667=CYLINDRICAL_SURFACE('',#16786,5.);
#3668=CYLINDRICAL_SURFACE('',#16787,0.5);
#3669=CYLINDRICAL_SURFACE('',#16792,0.5);
#3670=CYLINDRICAL_SURFACE('',#16794,0.499999999999998);
#3671=CYLINDRICAL_SURFACE('',#16819,1.);
#3672=CYLINDRICAL_SURFACE('',#16822,0.5);
#3673=CYLINDRICAL_SURFACE('',#16823,1.);
#3674=CYLINDRICAL_SURFACE('',#16825,0.5);
#3675=CYLINDRICAL_SURFACE('',#16826,0.5);
#3676=CYLINDRICAL_SURFACE('',#16827,1.);
#3677=CYLINDRICAL_SURFACE('',#16828,0.5);
#3678=CYLINDRICAL_SURFACE('',#16829,1.);
#3679=CYLINDRICAL_SURFACE('',#16830,1.);
#3680=CYLINDRICAL_SURFACE('',#16832,1.);
#3681=CYLINDRICAL_SURFACE('',#16836,0.999999999999999);
#3682=CYLINDRICAL_SURFACE('',#16840,1.);
#3683=CYLINDRICAL_SURFACE('',#16853,4.5);
#3684=CYLINDRICAL_SURFACE('',#16857,3.5);
#3685=CYLINDRICAL_SURFACE('',#16860,1.6);
#3686=CYLINDRICAL_SURFACE('',#16880,3.15);
#3687=CYLINDRICAL_SURFACE('',#16881,5.8);
#3688=CYLINDRICAL_SURFACE('',#16899,5.);
#3689=CYLINDRICAL_SURFACE('',#16906,3.);
#3690=FACE_OUTER_BOUND('',#4557,.T.);
#3691=FACE_OUTER_BOUND('',#4558,.T.);
#3692=FACE_OUTER_BOUND('',#4559,.T.);
#3693=FACE_OUTER_BOUND('',#4560,.T.);
#3694=FACE_OUTER_BOUND('',#4561,.T.);
#3695=FACE_OUTER_BOUND('',#4562,.T.);
#3696=FACE_OUTER_BOUND('',#4563,.T.);
#3697=FACE_OUTER_BOUND('',#4564,.T.);
#3698=FACE_OUTER_BOUND('',#4565,.T.);
#3699=FACE_OUTER_BOUND('',#4566,.T.);
#3700=FACE_OUTER_BOUND('',#4567,.T.);
#3701=FACE_OUTER_BOUND('',#4568,.T.);
#3702=FACE_OUTER_BOUND('',#4569,.T.);
#3703=FACE_OUTER_BOUND('',#4570,.T.);
#3704=FACE_OUTER_BOUND('',#4571,.T.);
#3705=FACE_OUTER_BOUND('',#4572,.T.);
#3706=FACE_OUTER_BOUND('',#4573,.T.);
#3707=FACE_OUTER_BOUND('',#4574,.T.);
#3708=FACE_OUTER_BOUND('',#4575,.T.);
#3709=FACE_OUTER_BOUND('',#4576,.T.);
#3710=FACE_OUTER_BOUND('',#4578,.T.);
#3711=FACE_OUTER_BOUND('',#4580,.T.);
#3712=FACE_OUTER_BOUND('',#4582,.T.);
#3713=FACE_OUTER_BOUND('',#4583,.T.);
#3714=FACE_OUTER_BOUND('',#4584,.T.);
#3715=FACE_OUTER_BOUND('',#4585,.T.);
#3716=FACE_OUTER_BOUND('',#4586,.T.);
#3717=FACE_OUTER_BOUND('',#4587,.T.);
#3718=FACE_OUTER_BOUND('',#4588,.T.);
#3719=FACE_OUTER_BOUND('',#4589,.T.);
#3720=FACE_OUTER_BOUND('',#4590,.T.);
#3721=FACE_OUTER_BOUND('',#4591,.T.);
#3722=FACE_OUTER_BOUND('',#4592,.T.);
#3723=FACE_OUTER_BOUND('',#4593,.T.);
#3724=FACE_OUTER_BOUND('',#4594,.T.);
#3725=FACE_OUTER_BOUND('',#4595,.T.);
#3726=FACE_OUTER_BOUND('',#4596,.T.);
#3727=FACE_OUTER_BOUND('',#4597,.T.);
#3728=FACE_OUTER_BOUND('',#4598,.T.);
#3729=FACE_OUTER_BOUND('',#4599,.T.);
#3730=FACE_OUTER_BOUND('',#4600,.T.);
#3731=FACE_OUTER_BOUND('',#4601,.T.);
#3732=FACE_OUTER_BOUND('',#4602,.T.);
#3733=FACE_OUTER_BOUND('',#4603,.T.);
#3734=FACE_OUTER_BOUND('',#4605,.T.);
#3735=FACE_OUTER_BOUND('',#4606,.T.);
#3736=FACE_OUTER_BOUND('',#4607,.T.);
#3737=FACE_OUTER_BOUND('',#4608,.T.);
#3738=FACE_OUTER_BOUND('',#4609,.T.);
#3739=FACE_OUTER_BOUND('',#4610,.T.);
#3740=FACE_OUTER_BOUND('',#4611,.T.);
#3741=FACE_OUTER_BOUND('',#4612,.T.);
#3742=FACE_OUTER_BOUND('',#4613,.T.);
#3743=FACE_OUTER_BOUND('',#4614,.T.);
#3744=FACE_OUTER_BOUND('',#4615,.T.);
#3745=FACE_OUTER_BOUND('',#4616,.T.);
#3746=FACE_OUTER_BOUND('',#4617,.T.);
#3747=FACE_OUTER_BOUND('',#4618,.T.);
#3748=FACE_OUTER_BOUND('',#4619,.T.);
#3749=FACE_OUTER_BOUND('',#4620,.T.);
#3750=FACE_OUTER_BOUND('',#4621,.T.);
#3751=FACE_OUTER_BOUND('',#4622,.T.);
#3752=FACE_OUTER_BOUND('',#4624,.T.);
#3753=FACE_OUTER_BOUND('',#4625,.T.);
#3754=FACE_OUTER_BOUND('',#4626,.T.);
#3755=FACE_OUTER_BOUND('',#4627,.T.);
#3756=FACE_OUTER_BOUND('',#4628,.T.);
#3757=FACE_OUTER_BOUND('',#4629,.T.);
#3758=FACE_OUTER_BOUND('',#4630,.T.);
#3759=FACE_OUTER_BOUND('',#4631,.T.);
#3760=FACE_OUTER_BOUND('',#4633,.T.);
#3761=FACE_OUTER_BOUND('',#4634,.T.);
#3762=FACE_OUTER_BOUND('',#4635,.T.);
#3763=FACE_OUTER_BOUND('',#4636,.T.);
#3764=FACE_OUTER_BOUND('',#4637,.T.);
#3765=FACE_OUTER_BOUND('',#4640,.T.);
#3766=FACE_OUTER_BOUND('',#4641,.T.);
#3767=FACE_OUTER_BOUND('',#4644,.T.);
#3768=FACE_OUTER_BOUND('',#4647,.T.);
#3769=FACE_OUTER_BOUND('',#4649,.T.);
#3770=FACE_OUTER_BOUND('',#4650,.T.);
#3771=FACE_OUTER_BOUND('',#4651,.T.);
#3772=FACE_OUTER_BOUND('',#4654,.T.);
#3773=FACE_OUTER_BOUND('',#4656,.T.);
#3774=FACE_OUTER_BOUND('',#4657,.T.);
#3775=FACE_OUTER_BOUND('',#4658,.T.);
#3776=FACE_OUTER_BOUND('',#4659,.T.);
#3777=FACE_OUTER_BOUND('',#4660,.T.);
#3778=FACE_OUTER_BOUND('',#4661,.T.);
#3779=FACE_OUTER_BOUND('',#4663,.T.);
#3780=FACE_OUTER_BOUND('',#4664,.T.);
#3781=FACE_OUTER_BOUND('',#4665,.T.);
#3782=FACE_OUTER_BOUND('',#4666,.T.);
#3783=FACE_OUTER_BOUND('',#4667,.T.);
#3784=FACE_OUTER_BOUND('',#4668,.T.);
#3785=FACE_OUTER_BOUND('',#4670,.T.);
#3786=FACE_OUTER_BOUND('',#4671,.T.);
#3787=FACE_OUTER_BOUND('',#4672,.T.);
#3788=FACE_OUTER_BOUND('',#4673,.T.);
#3789=FACE_OUTER_BOUND('',#4674,.T.);
#3790=FACE_OUTER_BOUND('',#4675,.T.);
#3791=FACE_OUTER_BOUND('',#4676,.T.);
#3792=FACE_OUTER_BOUND('',#4677,.T.);
#3793=FACE_OUTER_BOUND('',#4678,.T.);
#3794=FACE_OUTER_BOUND('',#4679,.T.);
#3795=FACE_OUTER_BOUND('',#4680,.T.);
#3796=FACE_OUTER_BOUND('',#4681,.T.);
#3797=FACE_OUTER_BOUND('',#4682,.T.);
#3798=FACE_OUTER_BOUND('',#4683,.T.);
#3799=FACE_OUTER_BOUND('',#4684,.T.);
#3800=FACE_OUTER_BOUND('',#4685,.T.);
#3801=FACE_OUTER_BOUND('',#4686,.T.);
#3802=FACE_OUTER_BOUND('',#4687,.T.);
#3803=FACE_OUTER_BOUND('',#4688,.T.);
#3804=FACE_OUTER_BOUND('',#4689,.T.);
#3805=FACE_OUTER_BOUND('',#4690,.T.);
#3806=FACE_OUTER_BOUND('',#4691,.T.);
#3807=FACE_OUTER_BOUND('',#4692,.T.);
#3808=FACE_OUTER_BOUND('',#4693,.T.);
#3809=FACE_OUTER_BOUND('',#4695,.T.);
#3810=FACE_OUTER_BOUND('',#4699,.T.);
#3811=FACE_OUTER_BOUND('',#4701,.T.);
#3812=FACE_OUTER_BOUND('',#4702,.T.);
#3813=FACE_OUTER_BOUND('',#4703,.T.);
#3814=FACE_OUTER_BOUND('',#4704,.T.);
#3815=FACE_OUTER_BOUND('',#4705,.T.);
#3816=FACE_OUTER_BOUND('',#4706,.T.);
#3817=FACE_OUTER_BOUND('',#4707,.T.);
#3818=FACE_OUTER_BOUND('',#4708,.T.);
#3819=FACE_OUTER_BOUND('',#4709,.T.);
#3820=FACE_OUTER_BOUND('',#4710,.T.);
#3821=FACE_OUTER_BOUND('',#4711,.T.);
#3822=FACE_OUTER_BOUND('',#4712,.T.);
#3823=FACE_OUTER_BOUND('',#4713,.T.);
#3824=FACE_OUTER_BOUND('',#4714,.T.);
#3825=FACE_OUTER_BOUND('',#4715,.T.);
#3826=FACE_OUTER_BOUND('',#4716,.T.);
#3827=FACE_OUTER_BOUND('',#4717,.T.);
#3828=FACE_OUTER_BOUND('',#4718,.T.);
#3829=FACE_OUTER_BOUND('',#4719,.T.);
#3830=FACE_OUTER_BOUND('',#4720,.T.);
#3831=FACE_OUTER_BOUND('',#4721,.T.);
#3832=FACE_OUTER_BOUND('',#4722,.T.);
#3833=FACE_OUTER_BOUND('',#4723,.T.);
#3834=FACE_OUTER_BOUND('',#4724,.T.);
#3835=FACE_OUTER_BOUND('',#4725,.T.);
#3836=FACE_OUTER_BOUND('',#4726,.T.);
#3837=FACE_OUTER_BOUND('',#4727,.T.);
#3838=FACE_OUTER_BOUND('',#4728,.T.);
#3839=FACE_OUTER_BOUND('',#4729,.T.);
#3840=FACE_OUTER_BOUND('',#4730,.T.);
#3841=FACE_OUTER_BOUND('',#4731,.T.);
#3842=FACE_OUTER_BOUND('',#4732,.T.);
#3843=FACE_OUTER_BOUND('',#4733,.T.);
#3844=FACE_OUTER_BOUND('',#4734,.T.);
#3845=FACE_OUTER_BOUND('',#4735,.T.);
#3846=FACE_OUTER_BOUND('',#4736,.T.);
#3847=FACE_OUTER_BOUND('',#4737,.T.);
#3848=FACE_OUTER_BOUND('',#4738,.T.);
#3849=FACE_OUTER_BOUND('',#4739,.T.);
#3850=FACE_OUTER_BOUND('',#4740,.T.);
#3851=FACE_OUTER_BOUND('',#4741,.T.);
#3852=FACE_OUTER_BOUND('',#4742,.T.);
#3853=FACE_OUTER_BOUND('',#4743,.T.);
#3854=FACE_OUTER_BOUND('',#4744,.T.);
#3855=FACE_OUTER_BOUND('',#4745,.T.);
#3856=FACE_OUTER_BOUND('',#4746,.T.);
#3857=FACE_OUTER_BOUND('',#4747,.T.);
#3858=FACE_OUTER_BOUND('',#4748,.T.);
#3859=FACE_OUTER_BOUND('',#4749,.T.);
#3860=FACE_OUTER_BOUND('',#4750,.T.);
#3861=FACE_OUTER_BOUND('',#4751,.T.);
#3862=FACE_OUTER_BOUND('',#4752,.T.);
#3863=FACE_OUTER_BOUND('',#4753,.T.);
#3864=FACE_OUTER_BOUND('',#4754,.T.);
#3865=FACE_OUTER_BOUND('',#4755,.T.);
#3866=FACE_OUTER_BOUND('',#4756,.T.);
#3867=FACE_OUTER_BOUND('',#4757,.T.);
#3868=FACE_OUTER_BOUND('',#4758,.T.);
#3869=FACE_OUTER_BOUND('',#4759,.T.);
#3870=FACE_OUTER_BOUND('',#4760,.T.);
#3871=FACE_OUTER_BOUND('',#4761,.T.);
#3872=FACE_OUTER_BOUND('',#4762,.T.);
#3873=FACE_OUTER_BOUND('',#4763,.T.);
#3874=FACE_OUTER_BOUND('',#4764,.T.);
#3875=FACE_OUTER_BOUND('',#4765,.T.);
#3876=FACE_OUTER_BOUND('',#4766,.T.);
#3877=FACE_OUTER_BOUND('',#4767,.T.);
#3878=FACE_OUTER_BOUND('',#4768,.T.);
#3879=FACE_OUTER_BOUND('',#4769,.T.);
#3880=FACE_OUTER_BOUND('',#4770,.T.);
#3881=FACE_OUTER_BOUND('',#4771,.T.);
#3882=FACE_OUTER_BOUND('',#4772,.T.);
#3883=FACE_OUTER_BOUND('',#4773,.T.);
#3884=FACE_OUTER_BOUND('',#4774,.T.);
#3885=FACE_OUTER_BOUND('',#4775,.T.);
#3886=FACE_OUTER_BOUND('',#4776,.T.);
#3887=FACE_OUTER_BOUND('',#4777,.T.);
#3888=FACE_OUTER_BOUND('',#4778,.T.);
#3889=FACE_OUTER_BOUND('',#4779,.T.);
#3890=FACE_OUTER_BOUND('',#4780,.T.);
#3891=FACE_OUTER_BOUND('',#4781,.T.);
#3892=FACE_OUTER_BOUND('',#4782,.T.);
#3893=FACE_OUTER_BOUND('',#4783,.T.);
#3894=FACE_OUTER_BOUND('',#4784,.T.);
#3895=FACE_OUTER_BOUND('',#4785,.T.);
#3896=FACE_OUTER_BOUND('',#4786,.T.);
#3897=FACE_OUTER_BOUND('',#4787,.T.);
#3898=FACE_OUTER_BOUND('',#4788,.T.);
#3899=FACE_OUTER_BOUND('',#4789,.T.);
#3900=FACE_OUTER_BOUND('',#4790,.T.);
#3901=FACE_OUTER_BOUND('',#4791,.T.);
#3902=FACE_OUTER_BOUND('',#4792,.T.);
#3903=FACE_OUTER_BOUND('',#4793,.T.);
#3904=FACE_OUTER_BOUND('',#4794,.T.);
#3905=FACE_OUTER_BOUND('',#4795,.T.);
#3906=FACE_OUTER_BOUND('',#4796,.T.);
#3907=FACE_OUTER_BOUND('',#4797,.T.);
#3908=FACE_OUTER_BOUND('',#4798,.T.);
#3909=FACE_OUTER_BOUND('',#4799,.T.);
#3910=FACE_OUTER_BOUND('',#4800,.T.);
#3911=FACE_OUTER_BOUND('',#4801,.T.);
#3912=FACE_OUTER_BOUND('',#4802,.T.);
#3913=FACE_OUTER_BOUND('',#4803,.T.);
#3914=FACE_OUTER_BOUND('',#4804,.T.);
#3915=FACE_OUTER_BOUND('',#4805,.T.);
#3916=FACE_OUTER_BOUND('',#4806,.T.);
#3917=FACE_OUTER_BOUND('',#4807,.T.);
#3918=FACE_OUTER_BOUND('',#4808,.T.);
#3919=FACE_OUTER_BOUND('',#4809,.T.);
#3920=FACE_OUTER_BOUND('',#4810,.T.);
#3921=FACE_OUTER_BOUND('',#4811,.T.);
#3922=FACE_OUTER_BOUND('',#4812,.T.);
#3923=FACE_OUTER_BOUND('',#4813,.T.);
#3924=FACE_OUTER_BOUND('',#4814,.T.);
#3925=FACE_OUTER_BOUND('',#4815,.T.);
#3926=FACE_OUTER_BOUND('',#4816,.T.);
#3927=FACE_OUTER_BOUND('',#4817,.T.);
#3928=FACE_OUTER_BOUND('',#4818,.T.);
#3929=FACE_OUTER_BOUND('',#4819,.T.);
#3930=FACE_OUTER_BOUND('',#4820,.T.);
#3931=FACE_OUTER_BOUND('',#4821,.T.);
#3932=FACE_OUTER_BOUND('',#4822,.T.);
#3933=FACE_OUTER_BOUND('',#4823,.T.);
#3934=FACE_OUTER_BOUND('',#4824,.T.);
#3935=FACE_OUTER_BOUND('',#4825,.T.);
#3936=FACE_OUTER_BOUND('',#4827,.T.);
#3937=FACE_OUTER_BOUND('',#4829,.T.);
#3938=FACE_OUTER_BOUND('',#4830,.T.);
#3939=FACE_OUTER_BOUND('',#4831,.T.);
#3940=FACE_OUTER_BOUND('',#4833,.T.);
#3941=FACE_OUTER_BOUND('',#4834,.T.);
#3942=FACE_OUTER_BOUND('',#4835,.T.);
#3943=FACE_OUTER_BOUND('',#4836,.T.);
#3944=FACE_OUTER_BOUND('',#4837,.T.);
#3945=FACE_OUTER_BOUND('',#4838,.T.);
#3946=FACE_OUTER_BOUND('',#4839,.T.);
#3947=FACE_OUTER_BOUND('',#4840,.T.);
#3948=FACE_OUTER_BOUND('',#4841,.T.);
#3949=FACE_OUTER_BOUND('',#4842,.T.);
#3950=FACE_OUTER_BOUND('',#4843,.T.);
#3951=FACE_OUTER_BOUND('',#4844,.T.);
#3952=FACE_OUTER_BOUND('',#4845,.T.);
#3953=FACE_OUTER_BOUND('',#4846,.T.);
#3954=FACE_OUTER_BOUND('',#4847,.T.);
#3955=FACE_OUTER_BOUND('',#4848,.T.);
#3956=FACE_OUTER_BOUND('',#4849,.T.);
#3957=FACE_OUTER_BOUND('',#4850,.T.);
#3958=FACE_OUTER_BOUND('',#4851,.T.);
#3959=FACE_OUTER_BOUND('',#4852,.T.);
#3960=FACE_OUTER_BOUND('',#4853,.T.);
#3961=FACE_OUTER_BOUND('',#4854,.T.);
#3962=FACE_OUTER_BOUND('',#4855,.T.);
#3963=FACE_OUTER_BOUND('',#4856,.T.);
#3964=FACE_OUTER_BOUND('',#4857,.T.);
#3965=FACE_OUTER_BOUND('',#4858,.T.);
#3966=FACE_OUTER_BOUND('',#4859,.T.);
#3967=FACE_OUTER_BOUND('',#4860,.T.);
#3968=FACE_OUTER_BOUND('',#4861,.T.);
#3969=FACE_OUTER_BOUND('',#4862,.T.);
#3970=FACE_OUTER_BOUND('',#4863,.T.);
#3971=FACE_OUTER_BOUND('',#4864,.T.);
#3972=FACE_OUTER_BOUND('',#4866,.T.);
#3973=FACE_OUTER_BOUND('',#4867,.T.);
#3974=FACE_OUTER_BOUND('',#4868,.T.);
#3975=FACE_OUTER_BOUND('',#4869,.T.);
#3976=FACE_OUTER_BOUND('',#4870,.T.);
#3977=FACE_OUTER_BOUND('',#4871,.T.);
#3978=FACE_OUTER_BOUND('',#4872,.T.);
#3979=FACE_OUTER_BOUND('',#4873,.T.);
#3980=FACE_OUTER_BOUND('',#4874,.T.);
#3981=FACE_OUTER_BOUND('',#4875,.T.);
#3982=FACE_OUTER_BOUND('',#4876,.T.);
#3983=FACE_OUTER_BOUND('',#4877,.T.);
#3984=FACE_OUTER_BOUND('',#4878,.T.);
#3985=FACE_OUTER_BOUND('',#4879,.T.);
#3986=FACE_OUTER_BOUND('',#4880,.T.);
#3987=FACE_OUTER_BOUND('',#4881,.T.);
#3988=FACE_OUTER_BOUND('',#4882,.T.);
#3989=FACE_OUTER_BOUND('',#4883,.T.);
#3990=FACE_OUTER_BOUND('',#4884,.T.);
#3991=FACE_OUTER_BOUND('',#4885,.T.);
#3992=FACE_OUTER_BOUND('',#4886,.T.);
#3993=FACE_OUTER_BOUND('',#4887,.T.);
#3994=FACE_OUTER_BOUND('',#4888,.T.);
#3995=FACE_OUTER_BOUND('',#4889,.T.);
#3996=FACE_OUTER_BOUND('',#4890,.T.);
#3997=FACE_OUTER_BOUND('',#4891,.T.);
#3998=FACE_OUTER_BOUND('',#4892,.T.);
#3999=FACE_OUTER_BOUND('',#4893,.T.);
#4000=FACE_OUTER_BOUND('',#4894,.T.);
#4001=FACE_OUTER_BOUND('',#4895,.T.);
#4002=FACE_OUTER_BOUND('',#4896,.T.);
#4003=FACE_OUTER_BOUND('',#4897,.T.);
#4004=FACE_OUTER_BOUND('',#4901,.T.);
#4005=FACE_OUTER_BOUND('',#4902,.T.);
#4006=FACE_OUTER_BOUND('',#4903,.T.);
#4007=FACE_OUTER_BOUND('',#4904,.T.);
#4008=FACE_OUTER_BOUND('',#4905,.T.);
#4009=FACE_OUTER_BOUND('',#4906,.T.);
#4010=FACE_OUTER_BOUND('',#4907,.T.);
#4011=FACE_OUTER_BOUND('',#4908,.T.);
#4012=FACE_OUTER_BOUND('',#4909,.T.);
#4013=FACE_OUTER_BOUND('',#4910,.T.);
#4014=FACE_OUTER_BOUND('',#4911,.T.);
#4015=FACE_OUTER_BOUND('',#4913,.T.);
#4016=FACE_OUTER_BOUND('',#4914,.T.);
#4017=FACE_OUTER_BOUND('',#4915,.T.);
#4018=FACE_OUTER_BOUND('',#4916,.T.);
#4019=FACE_OUTER_BOUND('',#4917,.T.);
#4020=FACE_OUTER_BOUND('',#4918,.T.);
#4021=FACE_OUTER_BOUND('',#4919,.T.);
#4022=FACE_OUTER_BOUND('',#4920,.T.);
#4023=FACE_OUTER_BOUND('',#4921,.T.);
#4024=FACE_OUTER_BOUND('',#4922,.T.);
#4025=FACE_OUTER_BOUND('',#4923,.T.);
#4026=FACE_OUTER_BOUND('',#4924,.T.);
#4027=FACE_OUTER_BOUND('',#4925,.T.);
#4028=FACE_OUTER_BOUND('',#4926,.T.);
#4029=FACE_OUTER_BOUND('',#4927,.T.);
#4030=FACE_OUTER_BOUND('',#4928,.T.);
#4031=FACE_OUTER_BOUND('',#4929,.T.);
#4032=FACE_OUTER_BOUND('',#4930,.T.);
#4033=FACE_OUTER_BOUND('',#4931,.T.);
#4034=FACE_OUTER_BOUND('',#4932,.T.);
#4035=FACE_OUTER_BOUND('',#4933,.T.);
#4036=FACE_OUTER_BOUND('',#4934,.T.);
#4037=FACE_OUTER_BOUND('',#4935,.T.);
#4038=FACE_OUTER_BOUND('',#4936,.T.);
#4039=FACE_OUTER_BOUND('',#4937,.T.);
#4040=FACE_OUTER_BOUND('',#4938,.T.);
#4041=FACE_OUTER_BOUND('',#4939,.T.);
#4042=FACE_OUTER_BOUND('',#4940,.T.);
#4043=FACE_OUTER_BOUND('',#4941,.T.);
#4044=FACE_OUTER_BOUND('',#4942,.T.);
#4045=FACE_OUTER_BOUND('',#4943,.T.);
#4046=FACE_OUTER_BOUND('',#4944,.T.);
#4047=FACE_OUTER_BOUND('',#4945,.T.);
#4048=FACE_OUTER_BOUND('',#4946,.T.);
#4049=FACE_OUTER_BOUND('',#4947,.T.);
#4050=FACE_OUTER_BOUND('',#4948,.T.);
#4051=FACE_OUTER_BOUND('',#4949,.T.);
#4052=FACE_OUTER_BOUND('',#4950,.T.);
#4053=FACE_OUTER_BOUND('',#4951,.T.);
#4054=FACE_OUTER_BOUND('',#4952,.T.);
#4055=FACE_OUTER_BOUND('',#4953,.T.);
#4056=FACE_OUTER_BOUND('',#4954,.T.);
#4057=FACE_OUTER_BOUND('',#4955,.T.);
#4058=FACE_OUTER_BOUND('',#4956,.T.);
#4059=FACE_OUTER_BOUND('',#4957,.T.);
#4060=FACE_OUTER_BOUND('',#4958,.T.);
#4061=FACE_OUTER_BOUND('',#4959,.T.);
#4062=FACE_OUTER_BOUND('',#4960,.T.);
#4063=FACE_OUTER_BOUND('',#4961,.T.);
#4064=FACE_OUTER_BOUND('',#4962,.T.);
#4065=FACE_OUTER_BOUND('',#4963,.T.);
#4066=FACE_OUTER_BOUND('',#4964,.T.);
#4067=FACE_OUTER_BOUND('',#4965,.T.);
#4068=FACE_OUTER_BOUND('',#4966,.T.);
#4069=FACE_OUTER_BOUND('',#4967,.T.);
#4070=FACE_OUTER_BOUND('',#4968,.T.);
#4071=FACE_OUTER_BOUND('',#4969,.T.);
#4072=FACE_OUTER_BOUND('',#4970,.T.);
#4073=FACE_OUTER_BOUND('',#4971,.T.);
#4074=FACE_OUTER_BOUND('',#4972,.T.);
#4075=FACE_OUTER_BOUND('',#4973,.T.);
#4076=FACE_OUTER_BOUND('',#4974,.T.);
#4077=FACE_OUTER_BOUND('',#4975,.T.);
#4078=FACE_OUTER_BOUND('',#4976,.T.);
#4079=FACE_OUTER_BOUND('',#4977,.T.);
#4080=FACE_OUTER_BOUND('',#4978,.T.);
#4081=FACE_OUTER_BOUND('',#4979,.T.);
#4082=FACE_OUTER_BOUND('',#4980,.T.);
#4083=FACE_OUTER_BOUND('',#4981,.T.);
#4084=FACE_OUTER_BOUND('',#4982,.T.);
#4085=FACE_OUTER_BOUND('',#4983,.T.);
#4086=FACE_OUTER_BOUND('',#4984,.T.);
#4087=FACE_OUTER_BOUND('',#4985,.T.);
#4088=FACE_OUTER_BOUND('',#4986,.T.);
#4089=FACE_OUTER_BOUND('',#4987,.T.);
#4090=FACE_OUTER_BOUND('',#4988,.T.);
#4091=FACE_OUTER_BOUND('',#4989,.T.);
#4092=FACE_OUTER_BOUND('',#4990,.T.);
#4093=FACE_OUTER_BOUND('',#4991,.T.);
#4094=FACE_OUTER_BOUND('',#4992,.T.);
#4095=FACE_OUTER_BOUND('',#4993,.T.);
#4096=FACE_OUTER_BOUND('',#4994,.T.);
#4097=FACE_OUTER_BOUND('',#4995,.T.);
#4098=FACE_OUTER_BOUND('',#4996,.T.);
#4099=FACE_OUTER_BOUND('',#4997,.T.);
#4100=FACE_OUTER_BOUND('',#4998,.T.);
#4101=FACE_OUTER_BOUND('',#4999,.T.);
#4102=FACE_OUTER_BOUND('',#5000,.T.);
#4103=FACE_OUTER_BOUND('',#5001,.T.);
#4104=FACE_OUTER_BOUND('',#5002,.T.);
#4105=FACE_OUTER_BOUND('',#5003,.T.);
#4106=FACE_OUTER_BOUND('',#5004,.T.);
#4107=FACE_OUTER_BOUND('',#5005,.T.);
#4108=FACE_OUTER_BOUND('',#5006,.T.);
#4109=FACE_OUTER_BOUND('',#5007,.T.);
#4110=FACE_OUTER_BOUND('',#5008,.T.);
#4111=FACE_OUTER_BOUND('',#5009,.T.);
#4112=FACE_OUTER_BOUND('',#5010,.T.);
#4113=FACE_OUTER_BOUND('',#5011,.T.);
#4114=FACE_OUTER_BOUND('',#5016,.T.);
#4115=FACE_OUTER_BOUND('',#5018,.T.);
#4116=FACE_OUTER_BOUND('',#5019,.T.);
#4117=FACE_OUTER_BOUND('',#5020,.T.);
#4118=FACE_OUTER_BOUND('',#5021,.T.);
#4119=FACE_OUTER_BOUND('',#5022,.T.);
#4120=FACE_OUTER_BOUND('',#5023,.T.);
#4121=FACE_OUTER_BOUND('',#5024,.T.);
#4122=FACE_OUTER_BOUND('',#5025,.T.);
#4123=FACE_OUTER_BOUND('',#5026,.T.);
#4124=FACE_OUTER_BOUND('',#5027,.T.);
#4125=FACE_OUTER_BOUND('',#5028,.T.);
#4126=FACE_OUTER_BOUND('',#5029,.T.);
#4127=FACE_OUTER_BOUND('',#5030,.T.);
#4128=FACE_OUTER_BOUND('',#5031,.T.);
#4129=FACE_OUTER_BOUND('',#5032,.T.);
#4130=FACE_OUTER_BOUND('',#5033,.T.);
#4131=FACE_OUTER_BOUND('',#5034,.T.);
#4132=FACE_OUTER_BOUND('',#5035,.T.);
#4133=FACE_OUTER_BOUND('',#5036,.T.);
#4134=FACE_OUTER_BOUND('',#5037,.T.);
#4135=FACE_OUTER_BOUND('',#5038,.T.);
#4136=FACE_OUTER_BOUND('',#5039,.T.);
#4137=FACE_OUTER_BOUND('',#5040,.T.);
#4138=FACE_OUTER_BOUND('',#5041,.T.);
#4139=FACE_OUTER_BOUND('',#5042,.T.);
#4140=FACE_OUTER_BOUND('',#5044,.T.);
#4141=FACE_OUTER_BOUND('',#5045,.T.);
#4142=FACE_OUTER_BOUND('',#5046,.T.);
#4143=FACE_OUTER_BOUND('',#5047,.T.);
#4144=FACE_OUTER_BOUND('',#5048,.T.);
#4145=FACE_OUTER_BOUND('',#5049,.T.);
#4146=FACE_OUTER_BOUND('',#5051,.T.);
#4147=FACE_OUTER_BOUND('',#5052,.T.);
#4148=FACE_OUTER_BOUND('',#5053,.T.);
#4149=FACE_OUTER_BOUND('',#5054,.T.);
#4150=FACE_OUTER_BOUND('',#5055,.T.);
#4151=FACE_OUTER_BOUND('',#5056,.T.);
#4152=FACE_OUTER_BOUND('',#5057,.T.);
#4153=FACE_OUTER_BOUND('',#5058,.T.);
#4154=FACE_OUTER_BOUND('',#5059,.T.);
#4155=FACE_OUTER_BOUND('',#5060,.T.);
#4156=FACE_OUTER_BOUND('',#5061,.T.);
#4157=FACE_OUTER_BOUND('',#5062,.T.);
#4158=FACE_OUTER_BOUND('',#5063,.T.);
#4159=FACE_OUTER_BOUND('',#5064,.T.);
#4160=FACE_OUTER_BOUND('',#5065,.T.);
#4161=FACE_OUTER_BOUND('',#5066,.T.);
#4162=FACE_OUTER_BOUND('',#5067,.T.);
#4163=FACE_OUTER_BOUND('',#5068,.T.);
#4164=FACE_OUTER_BOUND('',#5069,.T.);
#4165=FACE_OUTER_BOUND('',#5070,.T.);
#4166=FACE_OUTER_BOUND('',#5071,.T.);
#4167=FACE_OUTER_BOUND('',#5072,.T.);
#4168=FACE_OUTER_BOUND('',#5074,.T.);
#4169=FACE_OUTER_BOUND('',#5075,.T.);
#4170=FACE_OUTER_BOUND('',#5076,.T.);
#4171=FACE_OUTER_BOUND('',#5077,.T.);
#4172=FACE_OUTER_BOUND('',#5079,.T.);
#4173=FACE_OUTER_BOUND('',#5080,.T.);
#4174=FACE_OUTER_BOUND('',#5081,.T.);
#4175=FACE_OUTER_BOUND('',#5082,.T.);
#4176=FACE_OUTER_BOUND('',#5083,.T.);
#4177=FACE_OUTER_BOUND('',#5084,.T.);
#4178=FACE_OUTER_BOUND('',#5085,.T.);
#4179=FACE_OUTER_BOUND('',#5086,.T.);
#4180=FACE_OUTER_BOUND('',#5087,.T.);
#4181=FACE_OUTER_BOUND('',#5088,.T.);
#4182=FACE_OUTER_BOUND('',#5089,.T.);
#4183=FACE_OUTER_BOUND('',#5090,.T.);
#4184=FACE_OUTER_BOUND('',#5091,.T.);
#4185=FACE_OUTER_BOUND('',#5092,.T.);
#4186=FACE_OUTER_BOUND('',#5093,.T.);
#4187=FACE_OUTER_BOUND('',#5094,.T.);
#4188=FACE_OUTER_BOUND('',#5095,.T.);
#4189=FACE_OUTER_BOUND('',#5096,.T.);
#4190=FACE_OUTER_BOUND('',#5097,.T.);
#4191=FACE_OUTER_BOUND('',#5098,.T.);
#4192=FACE_OUTER_BOUND('',#5099,.T.);
#4193=FACE_OUTER_BOUND('',#5100,.T.);
#4194=FACE_OUTER_BOUND('',#5101,.T.);
#4195=FACE_OUTER_BOUND('',#5102,.T.);
#4196=FACE_OUTER_BOUND('',#5103,.T.);
#4197=FACE_OUTER_BOUND('',#5104,.T.);
#4198=FACE_OUTER_BOUND('',#5105,.T.);
#4199=FACE_OUTER_BOUND('',#5106,.T.);
#4200=FACE_OUTER_BOUND('',#5107,.T.);
#4201=FACE_OUTER_BOUND('',#5108,.T.);
#4202=FACE_OUTER_BOUND('',#5109,.T.);
#4203=FACE_OUTER_BOUND('',#5110,.T.);
#4204=FACE_OUTER_BOUND('',#5111,.T.);
#4205=FACE_OUTER_BOUND('',#5112,.T.);
#4206=FACE_OUTER_BOUND('',#5114,.T.);
#4207=FACE_OUTER_BOUND('',#5115,.T.);
#4208=FACE_OUTER_BOUND('',#5116,.T.);
#4209=FACE_OUTER_BOUND('',#5117,.T.);
#4210=FACE_OUTER_BOUND('',#5118,.T.);
#4211=FACE_OUTER_BOUND('',#5119,.T.);
#4212=FACE_OUTER_BOUND('',#5120,.T.);
#4213=FACE_OUTER_BOUND('',#5121,.T.);
#4214=FACE_OUTER_BOUND('',#5122,.T.);
#4215=FACE_OUTER_BOUND('',#5123,.T.);
#4216=FACE_OUTER_BOUND('',#5124,.T.);
#4217=FACE_OUTER_BOUND('',#5125,.T.);
#4218=FACE_OUTER_BOUND('',#5126,.T.);
#4219=FACE_OUTER_BOUND('',#5127,.T.);
#4220=FACE_OUTER_BOUND('',#5128,.T.);
#4221=FACE_OUTER_BOUND('',#5129,.T.);
#4222=FACE_OUTER_BOUND('',#5130,.T.);
#4223=FACE_OUTER_BOUND('',#5131,.T.);
#4224=FACE_OUTER_BOUND('',#5132,.T.);
#4225=FACE_OUTER_BOUND('',#5133,.T.);
#4226=FACE_OUTER_BOUND('',#5134,.T.);
#4227=FACE_OUTER_BOUND('',#5135,.T.);
#4228=FACE_OUTER_BOUND('',#5136,.T.);
#4229=FACE_OUTER_BOUND('',#5137,.T.);
#4230=FACE_OUTER_BOUND('',#5138,.T.);
#4231=FACE_OUTER_BOUND('',#5139,.T.);
#4232=FACE_OUTER_BOUND('',#5140,.T.);
#4233=FACE_OUTER_BOUND('',#5141,.T.);
#4234=FACE_OUTER_BOUND('',#5142,.T.);
#4235=FACE_OUTER_BOUND('',#5143,.T.);
#4236=FACE_OUTER_BOUND('',#5144,.T.);
#4237=FACE_OUTER_BOUND('',#5145,.T.);
#4238=FACE_OUTER_BOUND('',#5146,.T.);
#4239=FACE_OUTER_BOUND('',#5147,.T.);
#4240=FACE_OUTER_BOUND('',#5148,.T.);
#4241=FACE_OUTER_BOUND('',#5149,.T.);
#4242=FACE_OUTER_BOUND('',#5150,.T.);
#4243=FACE_OUTER_BOUND('',#5151,.T.);
#4244=FACE_OUTER_BOUND('',#5152,.T.);
#4245=FACE_OUTER_BOUND('',#5153,.T.);
#4246=FACE_OUTER_BOUND('',#5154,.T.);
#4247=FACE_OUTER_BOUND('',#5155,.T.);
#4248=FACE_OUTER_BOUND('',#5156,.T.);
#4249=FACE_OUTER_BOUND('',#5157,.T.);
#4250=FACE_OUTER_BOUND('',#5158,.T.);
#4251=FACE_OUTER_BOUND('',#5159,.T.);
#4252=FACE_OUTER_BOUND('',#5160,.T.);
#4253=FACE_OUTER_BOUND('',#5161,.T.);
#4254=FACE_OUTER_BOUND('',#5162,.T.);
#4255=FACE_OUTER_BOUND('',#5163,.T.);
#4256=FACE_OUTER_BOUND('',#5165,.T.);
#4257=FACE_OUTER_BOUND('',#5167,.T.);
#4258=FACE_OUTER_BOUND('',#5168,.T.);
#4259=FACE_OUTER_BOUND('',#5169,.T.);
#4260=FACE_OUTER_BOUND('',#5170,.T.);
#4261=FACE_OUTER_BOUND('',#5171,.T.);
#4262=FACE_OUTER_BOUND('',#5172,.T.);
#4263=FACE_OUTER_BOUND('',#5173,.T.);
#4264=FACE_OUTER_BOUND('',#5174,.T.);
#4265=FACE_OUTER_BOUND('',#5175,.T.);
#4266=FACE_OUTER_BOUND('',#5177,.T.);
#4267=FACE_OUTER_BOUND('',#5178,.T.);
#4268=FACE_OUTER_BOUND('',#5180,.T.);
#4269=FACE_OUTER_BOUND('',#5181,.T.);
#4270=FACE_OUTER_BOUND('',#5182,.T.);
#4271=FACE_OUTER_BOUND('',#5184,.T.);
#4272=FACE_OUTER_BOUND('',#5185,.T.);
#4273=FACE_OUTER_BOUND('',#5186,.T.);
#4274=FACE_OUTER_BOUND('',#5188,.T.);
#4275=FACE_OUTER_BOUND('',#5189,.T.);
#4276=FACE_OUTER_BOUND('',#5190,.T.);
#4277=FACE_OUTER_BOUND('',#5191,.T.);
#4278=FACE_OUTER_BOUND('',#5192,.T.);
#4279=FACE_OUTER_BOUND('',#5193,.T.);
#4280=FACE_OUTER_BOUND('',#5194,.T.);
#4281=FACE_OUTER_BOUND('',#5195,.T.);
#4282=FACE_OUTER_BOUND('',#5196,.T.);
#4283=FACE_OUTER_BOUND('',#5197,.T.);
#4284=FACE_OUTER_BOUND('',#5198,.T.);
#4285=FACE_OUTER_BOUND('',#5199,.T.);
#4286=FACE_OUTER_BOUND('',#5200,.T.);
#4287=FACE_OUTER_BOUND('',#5201,.T.);
#4288=FACE_OUTER_BOUND('',#5202,.T.);
#4289=FACE_OUTER_BOUND('',#5204,.T.);
#4290=FACE_OUTER_BOUND('',#5206,.T.);
#4291=FACE_OUTER_BOUND('',#5208,.T.);
#4292=FACE_OUTER_BOUND('',#5209,.T.);
#4293=FACE_OUTER_BOUND('',#5210,.T.);
#4294=FACE_OUTER_BOUND('',#5211,.T.);
#4295=FACE_OUTER_BOUND('',#5212,.T.);
#4296=FACE_OUTER_BOUND('',#5213,.T.);
#4297=FACE_OUTER_BOUND('',#5214,.T.);
#4298=FACE_OUTER_BOUND('',#5215,.T.);
#4299=FACE_OUTER_BOUND('',#5216,.T.);
#4300=FACE_OUTER_BOUND('',#5217,.T.);
#4301=FACE_OUTER_BOUND('',#5218,.T.);
#4302=FACE_OUTER_BOUND('',#5219,.T.);
#4303=FACE_OUTER_BOUND('',#5220,.T.);
#4304=FACE_OUTER_BOUND('',#5222,.T.);
#4305=FACE_OUTER_BOUND('',#5226,.T.);
#4306=FACE_OUTER_BOUND('',#5227,.T.);
#4307=FACE_OUTER_BOUND('',#5230,.T.);
#4308=FACE_OUTER_BOUND('',#5231,.T.);
#4309=FACE_OUTER_BOUND('',#5232,.T.);
#4310=FACE_OUTER_BOUND('',#5233,.T.);
#4311=FACE_OUTER_BOUND('',#5234,.T.);
#4312=FACE_OUTER_BOUND('',#5238,.T.);
#4313=FACE_OUTER_BOUND('',#5239,.T.);
#4314=FACE_OUTER_BOUND('',#5240,.T.);
#4315=FACE_OUTER_BOUND('',#5243,.T.);
#4316=FACE_OUTER_BOUND('',#5244,.T.);
#4317=FACE_OUTER_BOUND('',#5245,.T.);
#4318=FACE_OUTER_BOUND('',#5247,.T.);
#4319=FACE_OUTER_BOUND('',#5248,.T.);
#4320=FACE_OUTER_BOUND('',#5249,.T.);
#4321=FACE_OUTER_BOUND('',#5251,.T.);
#4322=FACE_OUTER_BOUND('',#5252,.T.);
#4323=FACE_OUTER_BOUND('',#5254,.T.);
#4324=FACE_OUTER_BOUND('',#5255,.T.);
#4325=FACE_OUTER_BOUND('',#5256,.T.);
#4326=FACE_OUTER_BOUND('',#5257,.T.);
#4327=FACE_OUTER_BOUND('',#5258,.T.);
#4328=FACE_OUTER_BOUND('',#5259,.T.);
#4329=FACE_OUTER_BOUND('',#5260,.T.);
#4330=FACE_OUTER_BOUND('',#5261,.T.);
#4331=FACE_OUTER_BOUND('',#5262,.T.);
#4332=FACE_OUTER_BOUND('',#5263,.T.);
#4333=FACE_OUTER_BOUND('',#5264,.T.);
#4334=FACE_OUTER_BOUND('',#5267,.T.);
#4335=FACE_OUTER_BOUND('',#5268,.T.);
#4336=FACE_OUTER_BOUND('',#5269,.T.);
#4337=FACE_OUTER_BOUND('',#5270,.T.);
#4338=FACE_OUTER_BOUND('',#5271,.T.);
#4339=FACE_OUTER_BOUND('',#5272,.T.);
#4340=FACE_OUTER_BOUND('',#5273,.T.);
#4341=FACE_OUTER_BOUND('',#5274,.T.);
#4342=FACE_OUTER_BOUND('',#5275,.T.);
#4343=FACE_OUTER_BOUND('',#5276,.T.);
#4344=FACE_OUTER_BOUND('',#5279,.T.);
#4345=FACE_OUTER_BOUND('',#5280,.T.);
#4346=FACE_OUTER_BOUND('',#5281,.T.);
#4347=FACE_OUTER_BOUND('',#5282,.T.);
#4348=FACE_OUTER_BOUND('',#5283,.T.);
#4349=FACE_OUTER_BOUND('',#5284,.T.);
#4350=FACE_OUTER_BOUND('',#5285,.T.);
#4351=FACE_OUTER_BOUND('',#5286,.T.);
#4352=FACE_OUTER_BOUND('',#5287,.T.);
#4353=FACE_OUTER_BOUND('',#5288,.T.);
#4354=FACE_OUTER_BOUND('',#5289,.T.);
#4355=FACE_OUTER_BOUND('',#5290,.T.);
#4356=FACE_OUTER_BOUND('',#5291,.T.);
#4357=FACE_OUTER_BOUND('',#5292,.T.);
#4358=FACE_OUTER_BOUND('',#5293,.T.);
#4359=FACE_OUTER_BOUND('',#5294,.T.);
#4360=FACE_OUTER_BOUND('',#5295,.T.);
#4361=FACE_OUTER_BOUND('',#5296,.T.);
#4362=FACE_OUTER_BOUND('',#5297,.T.);
#4363=FACE_OUTER_BOUND('',#5298,.T.);
#4364=FACE_OUTER_BOUND('',#5299,.T.);
#4365=FACE_OUTER_BOUND('',#5300,.T.);
#4366=FACE_OUTER_BOUND('',#5301,.T.);
#4367=FACE_OUTER_BOUND('',#5302,.T.);
#4368=FACE_OUTER_BOUND('',#5303,.T.);
#4369=FACE_OUTER_BOUND('',#5304,.T.);
#4370=FACE_OUTER_BOUND('',#5305,.T.);
#4371=FACE_OUTER_BOUND('',#5306,.T.);
#4372=FACE_OUTER_BOUND('',#5307,.T.);
#4373=FACE_OUTER_BOUND('',#5308,.T.);
#4374=FACE_OUTER_BOUND('',#5309,.T.);
#4375=FACE_OUTER_BOUND('',#5310,.T.);
#4376=FACE_OUTER_BOUND('',#5311,.T.);
#4377=FACE_OUTER_BOUND('',#5312,.T.);
#4378=FACE_OUTER_BOUND('',#5313,.T.);
#4379=FACE_OUTER_BOUND('',#5314,.T.);
#4380=FACE_OUTER_BOUND('',#5315,.T.);
#4381=FACE_OUTER_BOUND('',#5316,.T.);
#4382=FACE_OUTER_BOUND('',#5317,.T.);
#4383=FACE_OUTER_BOUND('',#5318,.T.);
#4384=FACE_OUTER_BOUND('',#5322,.T.);
#4385=FACE_OUTER_BOUND('',#5323,.T.);
#4386=FACE_OUTER_BOUND('',#5324,.T.);
#4387=FACE_OUTER_BOUND('',#5325,.T.);
#4388=FACE_OUTER_BOUND('',#5326,.T.);
#4389=FACE_OUTER_BOUND('',#5327,.T.);
#4390=FACE_OUTER_BOUND('',#5328,.T.);
#4391=FACE_OUTER_BOUND('',#5329,.T.);
#4392=FACE_OUTER_BOUND('',#5330,.T.);
#4393=FACE_OUTER_BOUND('',#5331,.T.);
#4394=FACE_OUTER_BOUND('',#5332,.T.);
#4395=FACE_OUTER_BOUND('',#5333,.T.);
#4396=FACE_OUTER_BOUND('',#5334,.T.);
#4397=FACE_OUTER_BOUND('',#5335,.T.);
#4398=FACE_OUTER_BOUND('',#5336,.T.);
#4399=FACE_OUTER_BOUND('',#5337,.T.);
#4400=FACE_OUTER_BOUND('',#5338,.T.);
#4401=FACE_OUTER_BOUND('',#5339,.T.);
#4402=FACE_OUTER_BOUND('',#5340,.T.);
#4403=FACE_OUTER_BOUND('',#5341,.T.);
#4404=FACE_OUTER_BOUND('',#5342,.T.);
#4405=FACE_OUTER_BOUND('',#5343,.T.);
#4406=FACE_OUTER_BOUND('',#5344,.T.);
#4407=FACE_OUTER_BOUND('',#5345,.T.);
#4408=FACE_OUTER_BOUND('',#5346,.T.);
#4409=FACE_OUTER_BOUND('',#5347,.T.);
#4410=FACE_OUTER_BOUND('',#5348,.T.);
#4411=FACE_OUTER_BOUND('',#5349,.T.);
#4412=FACE_OUTER_BOUND('',#5350,.T.);
#4413=FACE_OUTER_BOUND('',#5351,.T.);
#4414=FACE_OUTER_BOUND('',#5352,.T.);
#4415=FACE_OUTER_BOUND('',#5353,.T.);
#4416=FACE_OUTER_BOUND('',#5354,.T.);
#4417=FACE_OUTER_BOUND('',#5355,.T.);
#4418=FACE_OUTER_BOUND('',#5356,.T.);
#4419=FACE_OUTER_BOUND('',#5357,.T.);
#4420=FACE_OUTER_BOUND('',#5358,.T.);
#4421=FACE_OUTER_BOUND('',#5359,.T.);
#4422=FACE_OUTER_BOUND('',#5360,.T.);
#4423=FACE_OUTER_BOUND('',#5361,.T.);
#4424=FACE_OUTER_BOUND('',#5362,.T.);
#4425=FACE_OUTER_BOUND('',#5363,.T.);
#4426=FACE_OUTER_BOUND('',#5364,.T.);
#4427=FACE_OUTER_BOUND('',#5365,.T.);
#4428=FACE_OUTER_BOUND('',#5366,.T.);
#4429=FACE_OUTER_BOUND('',#5367,.T.);
#4430=FACE_OUTER_BOUND('',#5368,.T.);
#4431=FACE_OUTER_BOUND('',#5369,.T.);
#4432=FACE_OUTER_BOUND('',#5371,.T.);
#4433=FACE_OUTER_BOUND('',#5372,.T.);
#4434=FACE_OUTER_BOUND('',#5373,.T.);
#4435=FACE_OUTER_BOUND('',#5375,.T.);
#4436=FACE_OUTER_BOUND('',#5376,.T.);
#4437=FACE_OUTER_BOUND('',#5377,.T.);
#4438=FACE_OUTER_BOUND('',#5379,.T.);
#4439=FACE_OUTER_BOUND('',#5380,.T.);
#4440=FACE_OUTER_BOUND('',#5381,.T.);
#4441=FACE_OUTER_BOUND('',#5382,.T.);
#4442=FACE_OUTER_BOUND('',#5383,.T.);
#4443=FACE_OUTER_BOUND('',#5385,.T.);
#4444=FACE_OUTER_BOUND('',#5388,.T.);
#4445=FACE_OUTER_BOUND('',#5389,.T.);
#4446=FACE_OUTER_BOUND('',#5390,.T.);
#4447=FACE_OUTER_BOUND('',#5391,.T.);
#4448=FACE_OUTER_BOUND('',#5392,.T.);
#4449=FACE_OUTER_BOUND('',#5393,.T.);
#4450=FACE_OUTER_BOUND('',#5394,.T.);
#4451=FACE_OUTER_BOUND('',#5395,.T.);
#4452=FACE_OUTER_BOUND('',#5396,.T.);
#4453=FACE_OUTER_BOUND('',#5397,.T.);
#4454=FACE_OUTER_BOUND('',#5398,.T.);
#4455=FACE_OUTER_BOUND('',#5399,.T.);
#4456=FACE_OUTER_BOUND('',#5400,.T.);
#4457=FACE_OUTER_BOUND('',#5401,.T.);
#4458=FACE_OUTER_BOUND('',#5402,.T.);
#4459=FACE_OUTER_BOUND('',#5403,.T.);
#4460=FACE_OUTER_BOUND('',#5404,.T.);
#4461=FACE_OUTER_BOUND('',#5405,.T.);
#4462=FACE_OUTER_BOUND('',#5406,.T.);
#4463=FACE_OUTER_BOUND('',#5407,.T.);
#4464=FACE_OUTER_BOUND('',#5408,.T.);
#4465=FACE_OUTER_BOUND('',#5409,.T.);
#4466=FACE_OUTER_BOUND('',#5410,.T.);
#4467=FACE_OUTER_BOUND('',#5411,.T.);
#4468=FACE_OUTER_BOUND('',#5414,.T.);
#4469=FACE_OUTER_BOUND('',#5415,.T.);
#4470=FACE_OUTER_BOUND('',#5416,.T.);
#4471=FACE_OUTER_BOUND('',#5417,.T.);
#4472=FACE_OUTER_BOUND('',#5418,.T.);
#4473=FACE_OUTER_BOUND('',#5419,.T.);
#4474=FACE_OUTER_BOUND('',#5420,.T.);
#4475=FACE_OUTER_BOUND('',#5421,.T.);
#4476=FACE_OUTER_BOUND('',#5422,.T.);
#4477=FACE_OUTER_BOUND('',#5423,.T.);
#4478=FACE_OUTER_BOUND('',#5424,.T.);
#4479=FACE_OUTER_BOUND('',#5425,.T.);
#4480=FACE_OUTER_BOUND('',#5426,.T.);
#4481=FACE_OUTER_BOUND('',#5427,.T.);
#4482=FACE_OUTER_BOUND('',#5428,.T.);
#4483=FACE_OUTER_BOUND('',#5429,.T.);
#4484=FACE_OUTER_BOUND('',#5430,.T.);
#4485=FACE_OUTER_BOUND('',#5431,.T.);
#4486=FACE_OUTER_BOUND('',#5432,.T.);
#4487=FACE_OUTER_BOUND('',#5433,.T.);
#4488=FACE_OUTER_BOUND('',#5434,.T.);
#4489=FACE_OUTER_BOUND('',#5435,.T.);
#4490=FACE_OUTER_BOUND('',#5436,.T.);
#4491=FACE_OUTER_BOUND('',#5437,.T.);
#4492=FACE_OUTER_BOUND('',#5438,.T.);
#4493=FACE_OUTER_BOUND('',#5439,.T.);
#4494=FACE_OUTER_BOUND('',#5440,.T.);
#4495=FACE_OUTER_BOUND('',#5441,.T.);
#4496=FACE_OUTER_BOUND('',#5442,.T.);
#4497=FACE_OUTER_BOUND('',#5443,.T.);
#4498=FACE_OUTER_BOUND('',#5444,.T.);
#4499=FACE_OUTER_BOUND('',#5445,.T.);
#4500=FACE_OUTER_BOUND('',#5446,.T.);
#4501=FACE_OUTER_BOUND('',#5447,.T.);
#4502=FACE_OUTER_BOUND('',#5449,.T.);
#4503=FACE_OUTER_BOUND('',#5450,.T.);
#4504=FACE_OUTER_BOUND('',#5451,.T.);
#4505=FACE_OUTER_BOUND('',#5452,.T.);
#4506=FACE_OUTER_BOUND('',#5453,.T.);
#4507=FACE_OUTER_BOUND('',#5454,.T.);
#4508=FACE_OUTER_BOUND('',#5455,.T.);
#4509=FACE_OUTER_BOUND('',#5456,.T.);
#4510=FACE_OUTER_BOUND('',#5457,.T.);
#4511=FACE_OUTER_BOUND('',#5458,.T.);
#4512=FACE_OUTER_BOUND('',#5459,.T.);
#4513=FACE_OUTER_BOUND('',#5460,.T.);
#4514=FACE_OUTER_BOUND('',#5462,.T.);
#4515=FACE_OUTER_BOUND('',#5463,.T.);
#4516=FACE_OUTER_BOUND('',#5464,.T.);
#4517=FACE_OUTER_BOUND('',#5466,.T.);
#4518=FACE_OUTER_BOUND('',#5468,.T.);
#4519=FACE_OUTER_BOUND('',#5469,.T.);
#4520=FACE_OUTER_BOUND('',#5470,.T.);
#4521=FACE_OUTER_BOUND('',#5471,.T.);
#4522=FACE_OUTER_BOUND('',#5472,.T.);
#4523=FACE_OUTER_BOUND('',#5473,.T.);
#4524=FACE_OUTER_BOUND('',#5474,.T.);
#4525=FACE_OUTER_BOUND('',#5475,.T.);
#4526=FACE_OUTER_BOUND('',#5476,.T.);
#4527=FACE_OUTER_BOUND('',#5477,.T.);
#4528=FACE_OUTER_BOUND('',#5478,.T.);
#4529=FACE_OUTER_BOUND('',#5479,.T.);
#4530=FACE_OUTER_BOUND('',#5480,.T.);
#4531=FACE_OUTER_BOUND('',#5481,.T.);
#4532=FACE_OUTER_BOUND('',#5482,.T.);
#4533=FACE_OUTER_BOUND('',#5483,.T.);
#4534=FACE_OUTER_BOUND('',#5484,.T.);
#4535=FACE_OUTER_BOUND('',#5485,.T.);
#4536=FACE_OUTER_BOUND('',#5486,.T.);
#4537=FACE_OUTER_BOUND('',#5487,.T.);
#4538=FACE_OUTER_BOUND('',#5488,.T.);
#4539=FACE_OUTER_BOUND('',#5489,.T.);
#4540=FACE_OUTER_BOUND('',#5490,.T.);
#4541=FACE_OUTER_BOUND('',#5491,.T.);
#4542=FACE_OUTER_BOUND('',#5492,.T.);
#4543=FACE_OUTER_BOUND('',#5493,.T.);
#4544=FACE_OUTER_BOUND('',#5494,.T.);
#4545=FACE_OUTER_BOUND('',#5495,.T.);
#4546=FACE_OUTER_BOUND('',#5496,.T.);
#4547=FACE_OUTER_BOUND('',#5498,.T.);
#4548=FACE_OUTER_BOUND('',#5499,.T.);
#4549=FACE_OUTER_BOUND('',#5500,.T.);
#4550=FACE_OUTER_BOUND('',#5501,.T.);
#4551=FACE_OUTER_BOUND('',#5502,.T.);
#4552=FACE_OUTER_BOUND('',#5503,.T.);
#4553=FACE_OUTER_BOUND('',#5504,.T.);
#4554=FACE_OUTER_BOUND('',#5505,.T.);
#4555=FACE_OUTER_BOUND('',#5506,.T.);
#4556=FACE_OUTER_BOUND('',#5508,.T.);
#4557=EDGE_LOOP('',(#9833,#9834,#9835,#9836));
#4558=EDGE_LOOP('',(#9837,#9838,#9839,#9840));
#4559=EDGE_LOOP('',(#9841,#9842,#9843,#9844));
#4560=EDGE_LOOP('',(#9845,#9846,#9847,#9848));
#4561=EDGE_LOOP('',(#9849,#9850,#9851,#9852));
#4562=EDGE_LOOP('',(#9853,#9854,#9855,#9856,#9857,#9858));
#4563=EDGE_LOOP('',(#9859,#9860,#9861,#9862));
#4564=EDGE_LOOP('',(#9863,#9864,#9865,#9866,#9867,#9868,#9869));
#4565=EDGE_LOOP('',(#9870,#9871,#9872,#9873));
#4566=EDGE_LOOP('',(#9874,#9875,#9876,#9877,#9878,#9879,#9880,#9881,#9882,
#9883));
#4567=EDGE_LOOP('',(#9884,#9885,#9886,#9887));
#4568=EDGE_LOOP('',(#9888,#9889,#9890,#9891));
#4569=EDGE_LOOP('',(#9892,#9893,#9894,#9895));
#4570=EDGE_LOOP('',(#9896,#9897,#9898,#9899));
#4571=EDGE_LOOP('',(#9900,#9901,#9902,#9903));
#4572=EDGE_LOOP('',(#9904,#9905,#9906,#9907));
#4573=EDGE_LOOP('',(#9908,#9909,#9910,#9911));
#4574=EDGE_LOOP('',(#9912,#9913,#9914,#9915));
#4575=EDGE_LOOP('',(#9916,#9917,#9918,#9919));
#4576=EDGE_LOOP('',(#9920));
#4577=EDGE_LOOP('',(#9921));
#4578=EDGE_LOOP('',(#9922));
#4579=EDGE_LOOP('',(#9923));
#4580=EDGE_LOOP('',(#9924));
#4581=EDGE_LOOP('',(#9925));
#4582=EDGE_LOOP('',(#9926));
#4583=EDGE_LOOP('',(#9927));
#4584=EDGE_LOOP('',(#9928,#9929,#9930,#9931));
#4585=EDGE_LOOP('',(#9932,#9933,#9934,#9935));
#4586=EDGE_LOOP('',(#9936,#9937,#9938,#9939));
#4587=EDGE_LOOP('',(#9940,#9941,#9942,#9943));
#4588=EDGE_LOOP('',(#9944,#9945,#9946,#9947));
#4589=EDGE_LOOP('',(#9948,#9949,#9950,#9951,#9952));
#4590=EDGE_LOOP('',(#9953,#9954,#9955,#9956));
#4591=EDGE_LOOP('',(#9957,#9958,#9959,#9960));
#4592=EDGE_LOOP('',(#9961,#9962,#9963,#9964));
#4593=EDGE_LOOP('',(#9965,#9966,#9967,#9968));
#4594=EDGE_LOOP('',(#9969,#9970,#9971,#9972));
#4595=EDGE_LOOP('',(#9973,#9974,#9975,#9976));
#4596=EDGE_LOOP('',(#9977,#9978,#9979,#9980));
#4597=EDGE_LOOP('',(#9981,#9982,#9983,#9984,#9985,#9986));
#4598=EDGE_LOOP('',(#9987,#9988,#9989,#9990));
#4599=EDGE_LOOP('',(#9991,#9992,#9993,#9994));
#4600=EDGE_LOOP('',(#9995,#9996,#9997,#9998));
#4601=EDGE_LOOP('',(#9999,#10000,#10001,#10002));
#4602=EDGE_LOOP('',(#10003,#10004,#10005,#10006));
#4603=EDGE_LOOP('',(#10007));
#4604=EDGE_LOOP('',(#10008));
#4605=EDGE_LOOP('',(#10009,#10010,#10011,#10012));
#4606=EDGE_LOOP('',(#10013,#10014,#10015,#10016));
#4607=EDGE_LOOP('',(#10017,#10018,#10019,#10020,#10021,#10022));
#4608=EDGE_LOOP('',(#10023,#10024,#10025,#10026));
#4609=EDGE_LOOP('',(#10027,#10028,#10029,#10030));
#4610=EDGE_LOOP('',(#10031,#10032,#10033,#10034));
#4611=EDGE_LOOP('',(#10035,#10036,#10037,#10038,#10039,#10040));
#4612=EDGE_LOOP('',(#10041,#10042,#10043,#10044,#10045,#10046));
#4613=EDGE_LOOP('',(#10047,#10048,#10049,#10050));
#4614=EDGE_LOOP('',(#10051,#10052,#10053,#10054,#10055,#10056));
#4615=EDGE_LOOP('',(#10057,#10058,#10059,#10060));
#4616=EDGE_LOOP('',(#10061,#10062,#10063,#10064));
#4617=EDGE_LOOP('',(#10065,#10066,#10067,#10068));
#4618=EDGE_LOOP('',(#10069,#10070,#10071,#10072,#10073,#10074,#10075,#10076));
#4619=EDGE_LOOP('',(#10077,#10078,#10079,#10080,#10081,#10082));
#4620=EDGE_LOOP('',(#10083,#10084,#10085,#10086,#10087));
#4621=EDGE_LOOP('',(#10088,#10089,#10090,#10091));
#4622=EDGE_LOOP('',(#10092));
#4623=EDGE_LOOP('',(#10093));
#4624=EDGE_LOOP('',(#10094,#10095,#10096));
#4625=EDGE_LOOP('',(#10097,#10098,#10099,#10100));
#4626=EDGE_LOOP('',(#10101,#10102,#10103));
#4627=EDGE_LOOP('',(#10104,#10105,#10106,#10107));
#4628=EDGE_LOOP('',(#10108,#10109,#10110,#10111));
#4629=EDGE_LOOP('',(#10112,#10113,#10114,#10115));
#4630=EDGE_LOOP('',(#10116,#10117,#10118,#10119));
#4631=EDGE_LOOP('',(#10120,#10121,#10122,#10123));
#4632=EDGE_LOOP('',(#10124,#10125,#10126,#10127));
#4633=EDGE_LOOP('',(#10128,#10129,#10130,#10131));
#4634=EDGE_LOOP('',(#10132,#10133,#10134,#10135));
#4635=EDGE_LOOP('',(#10136,#10137,#10138));
#4636=EDGE_LOOP('',(#10139,#10140,#10141,#10142));
#4637=EDGE_LOOP('',(#10143,#10144,#10145,#10146,#10147,#10148,#10149,#10150));
#4638=EDGE_LOOP('',(#10151));
#4639=EDGE_LOOP('',(#10152));
#4640=EDGE_LOOP('',(#10153));
#4641=EDGE_LOOP('',(#10154));
#4642=EDGE_LOOP('',(#10155));
#4643=EDGE_LOOP('',(#10156));
#4644=EDGE_LOOP('',(#10157,#10158,#10159,#10160,#10161,#10162,#10163,#10164));
#4645=EDGE_LOOP('',(#10165));
#4646=EDGE_LOOP('',(#10166));
#4647=EDGE_LOOP('',(#10167));
#4648=EDGE_LOOP('',(#10168));
#4649=EDGE_LOOP('',(#10169,#10170,#10171,#10172));
#4650=EDGE_LOOP('',(#10173,#10174,#10175,#10176));
#4651=EDGE_LOOP('',(#10177,#10178,#10179,#10180));
#4652=EDGE_LOOP('',(#10181,#10182,#10183,#10184));
#4653=EDGE_LOOP('',(#10185,#10186,#10187,#10188));
#4654=EDGE_LOOP('',(#10189));
#4655=EDGE_LOOP('',(#10190));
#4656=EDGE_LOOP('',(#10191,#10192,#10193,#10194));
#4657=EDGE_LOOP('',(#10195,#10196,#10197,#10198));
#4658=EDGE_LOOP('',(#10199,#10200,#10201,#10202));
#4659=EDGE_LOOP('',(#10203,#10204,#10205,#10206));
#4660=EDGE_LOOP('',(#10207,#10208,#10209,#10210));
#4661=EDGE_LOOP('',(#10211));
#4662=EDGE_LOOP('',(#10212,#10213,#10214,#10215,#10216,#10217,#10218,#10219,
#10220,#10221,#10222,#10223,#10224,#10225,#10226,#10227,#10228,#10229,#10230,
#10231));
#4663=EDGE_LOOP('',(#10232,#10233,#10234,#10235));
#4664=EDGE_LOOP('',(#10236,#10237,#10238,#10239,#10240));
#4665=EDGE_LOOP('',(#10241,#10242,#10243,#10244,#10245,#10246));
#4666=EDGE_LOOP('',(#10247,#10248,#10249,#10250,#10251));
#4667=EDGE_LOOP('',(#10252));
#4668=EDGE_LOOP('',(#10253));
#4669=EDGE_LOOP('',(#10254));
#4670=EDGE_LOOP('',(#10255,#10256,#10257,#10258));
#4671=EDGE_LOOP('',(#10259,#10260,#10261,#10262));
#4672=EDGE_LOOP('',(#10263,#10264,#10265,#10266));
#4673=EDGE_LOOP('',(#10267,#10268,#10269,#10270));
#4674=EDGE_LOOP('',(#10271,#10272,#10273,#10274));
#4675=EDGE_LOOP('',(#10275,#10276,#10277,#10278));
#4676=EDGE_LOOP('',(#10279,#10280,#10281,#10282));
#4677=EDGE_LOOP('',(#10283,#10284,#10285,#10286));
#4678=EDGE_LOOP('',(#10287,#10288,#10289,#10290));
#4679=EDGE_LOOP('',(#10291,#10292,#10293,#10294));
#4680=EDGE_LOOP('',(#10295,#10296,#10297,#10298));
#4681=EDGE_LOOP('',(#10299,#10300,#10301,#10302));
#4682=EDGE_LOOP('',(#10303,#10304,#10305,#10306));
#4683=EDGE_LOOP('',(#10307,#10308,#10309,#10310));
#4684=EDGE_LOOP('',(#10311,#10312,#10313,#10314));
#4685=EDGE_LOOP('',(#10315,#10316,#10317,#10318));
#4686=EDGE_LOOP('',(#10319,#10320,#10321,#10322));
#4687=EDGE_LOOP('',(#10323,#10324,#10325,#10326));
#4688=EDGE_LOOP('',(#10327,#10328,#10329,#10330,#10331,#10332,#10333,#10334,
#10335,#10336,#10337,#10338,#10339,#10340,#10341,#10342,#10343,#10344,#10345,
#10346));
#4689=EDGE_LOOP('',(#10347,#10348,#10349,#10350));
#4690=EDGE_LOOP('',(#10351,#10352,#10353,#10354));
#4691=EDGE_LOOP('',(#10355,#10356,#10357,#10358,#10359,#10360,#10361,#10362));
#4692=EDGE_LOOP('',(#10363,#10364,#10365,#10366,#10367,#10368,#10369,#10370));
#4693=EDGE_LOOP('',(#10371));
#4694=EDGE_LOOP('',(#10372,#10373,#10374,#10375,#10376,#10377,#10378,#10379,
#10380,#10381,#10382,#10383,#10384,#10385,#10386,#10387,#10388,#10389,#10390,
#10391));
#4695=EDGE_LOOP('',(#10392,#10393,#10394,#10395,#10396,#10397,#10398,#10399,
#10400,#10401,#10402,#10403,#10404,#10405,#10406,#10407));
#4696=EDGE_LOOP('',(#10408,#10409,#10410,#10411,#10412,#10413,#10414,#10415));
#4697=EDGE_LOOP('',(#10416,#10417,#10418,#10419));
#4698=EDGE_LOOP('',(#10420,#10421,#10422,#10423,#10424,#10425,#10426,#10427,
#10428,#10429,#10430,#10431));
#4699=EDGE_LOOP('',(#10432));
#4700=EDGE_LOOP('',(#10433,#10434,#10435,#10436,#10437,#10438,#10439,#10440,
#10441,#10442,#10443,#10444,#10445,#10446,#10447,#10448,#10449,#10450,#10451,
#10452));
#4701=EDGE_LOOP('',(#10453,#10454,#10455,#10456,#10457,#10458,#10459,#10460));
#4702=EDGE_LOOP('',(#10461,#10462,#10463,#10464));
#4703=EDGE_LOOP('',(#10465,#10466,#10467,#10468));
#4704=EDGE_LOOP('',(#10469,#10470,#10471,#10472));
#4705=EDGE_LOOP('',(#10473,#10474,#10475));
#4706=EDGE_LOOP('',(#10476,#10477,#10478,#10479));
#4707=EDGE_LOOP('',(#10480,#10481,#10482,#10483));
#4708=EDGE_LOOP('',(#10484,#10485,#10486,#10487,#10488,#10489,#10490,#10491,
#10492,#10493,#10494,#10495,#10496,#10497,#10498,#10499,#10500,#10501,#10502,
#10503));
#4709=EDGE_LOOP('',(#10504,#10505,#10506,#10507));
#4710=EDGE_LOOP('',(#10508,#10509,#10510,#10511));
#4711=EDGE_LOOP('',(#10512,#10513,#10514,#10515));
#4712=EDGE_LOOP('',(#10516,#10517,#10518,#10519));
#4713=EDGE_LOOP('',(#10520,#10521,#10522,#10523));
#4714=EDGE_LOOP('',(#10524,#10525,#10526,#10527));
#4715=EDGE_LOOP('',(#10528,#10529,#10530,#10531));
#4716=EDGE_LOOP('',(#10532,#10533,#10534,#10535));
#4717=EDGE_LOOP('',(#10536,#10537,#10538,#10539));
#4718=EDGE_LOOP('',(#10540,#10541,#10542,#10543));
#4719=EDGE_LOOP('',(#10544,#10545,#10546,#10547));
#4720=EDGE_LOOP('',(#10548,#10549,#10550,#10551));
#4721=EDGE_LOOP('',(#10552,#10553,#10554,#10555));
#4722=EDGE_LOOP('',(#10556,#10557,#10558,#10559));
#4723=EDGE_LOOP('',(#10560,#10561,#10562,#10563));
#4724=EDGE_LOOP('',(#10564,#10565,#10566,#10567));
#4725=EDGE_LOOP('',(#10568,#10569,#10570,#10571));
#4726=EDGE_LOOP('',(#10572,#10573,#10574,#10575));
#4727=EDGE_LOOP('',(#10576,#10577));
#4728=EDGE_LOOP('',(#10578,#10579,#10580,#10581));
#4729=EDGE_LOOP('',(#10582,#10583,#10584,#10585));
#4730=EDGE_LOOP('',(#10586));
#4731=EDGE_LOOP('',(#10587,#10588,#10589,#10590,#10591));
#4732=EDGE_LOOP('',(#10592,#10593));
#4733=EDGE_LOOP('',(#10594));
#4734=EDGE_LOOP('',(#10595,#10596,#10597,#10598));
#4735=EDGE_LOOP('',(#10599,#10600));
#4736=EDGE_LOOP('',(#10601,#10602,#10603,#10604,#10605));
#4737=EDGE_LOOP('',(#10606,#10607));
#4738=EDGE_LOOP('',(#10608,#10609,#10610,#10611));
#4739=EDGE_LOOP('',(#10612,#10613));
#4740=EDGE_LOOP('',(#10614,#10615,#10616,#10617));
#4741=EDGE_LOOP('',(#10618,#10619,#10620,#10621,#10622,#10623,#10624,#10625,
#10626,#10627,#10628,#10629,#10630,#10631,#10632,#10633,#10634,#10635,#10636,
#10637));
#4742=EDGE_LOOP('',(#10638,#10639,#10640,#10641));
#4743=EDGE_LOOP('',(#10642,#10643,#10644,#10645));
#4744=EDGE_LOOP('',(#10646,#10647,#10648,#10649));
#4745=EDGE_LOOP('',(#10650,#10651,#10652,#10653));
#4746=EDGE_LOOP('',(#10654,#10655,#10656,#10657));
#4747=EDGE_LOOP('',(#10658,#10659,#10660,#10661));
#4748=EDGE_LOOP('',(#10662,#10663,#10664,#10665));
#4749=EDGE_LOOP('',(#10666,#10667,#10668,#10669));
#4750=EDGE_LOOP('',(#10670,#10671,#10672,#10673));
#4751=EDGE_LOOP('',(#10674,#10675,#10676,#10677));
#4752=EDGE_LOOP('',(#10678,#10679,#10680,#10681));
#4753=EDGE_LOOP('',(#10682,#10683,#10684,#10685));
#4754=EDGE_LOOP('',(#10686,#10687,#10688,#10689));
#4755=EDGE_LOOP('',(#10690,#10691,#10692,#10693));
#4756=EDGE_LOOP('',(#10694,#10695,#10696,#10697));
#4757=EDGE_LOOP('',(#10698,#10699,#10700,#10701));
#4758=EDGE_LOOP('',(#10702,#10703,#10704,#10705));
#4759=EDGE_LOOP('',(#10706,#10707,#10708,#10709));
#4760=EDGE_LOOP('',(#10710,#10711,#10712,#10713));
#4761=EDGE_LOOP('',(#10714,#10715,#10716,#10717));
#4762=EDGE_LOOP('',(#10718,#10719));
#4763=EDGE_LOOP('',(#10720,#10721,#10722));
#4764=EDGE_LOOP('',(#10723,#10724,#10725));
#4765=EDGE_LOOP('',(#10726,#10727,#10728));
#4766=EDGE_LOOP('',(#10729,#10730,#10731));
#4767=EDGE_LOOP('',(#10732,#10733,#10734,#10735,#10736,#10737,#10738,#10739));
#4768=EDGE_LOOP('',(#10740,#10741,#10742));
#4769=EDGE_LOOP('',(#10743,#10744,#10745,#10746,#10747,#10748));
#4770=EDGE_LOOP('',(#10749,#10750,#10751,#10752));
#4771=EDGE_LOOP('',(#10753,#10754,#10755,#10756));
#4772=EDGE_LOOP('',(#10757,#10758,#10759,#10760));
#4773=EDGE_LOOP('',(#10761,#10762,#10763,#10764,#10765));
#4774=EDGE_LOOP('',(#10766,#10767,#10768,#10769));
#4775=EDGE_LOOP('',(#10770,#10771,#10772,#10773));
#4776=EDGE_LOOP('',(#10774,#10775,#10776,#10777));
#4777=EDGE_LOOP('',(#10778,#10779,#10780,#10781));
#4778=EDGE_LOOP('',(#10782,#10783,#10784,#10785));
#4779=EDGE_LOOP('',(#10786,#10787,#10788,#10789));
#4780=EDGE_LOOP('',(#10790,#10791,#10792,#10793));
#4781=EDGE_LOOP('',(#10794,#10795,#10796,#10797));
#4782=EDGE_LOOP('',(#10798,#10799,#10800,#10801,#10802,#10803));
#4783=EDGE_LOOP('',(#10804,#10805,#10806,#10807,#10808,#10809,#10810,#10811));
#4784=EDGE_LOOP('',(#10812,#10813,#10814,#10815));
#4785=EDGE_LOOP('',(#10816,#10817,#10818,#10819));
#4786=EDGE_LOOP('',(#10820,#10821,#10822,#10823,#10824,#10825,#10826,#10827));
#4787=EDGE_LOOP('',(#10828,#10829,#10830,#10831,#10832,#10833));
#4788=EDGE_LOOP('',(#10834,#10835,#10836,#10837,#10838,#10839));
#4789=EDGE_LOOP('',(#10840,#10841,#10842,#10843,#10844,#10845));
#4790=EDGE_LOOP('',(#10846,#10847,#10848,#10849));
#4791=EDGE_LOOP('',(#10850,#10851,#10852,#10853));
#4792=EDGE_LOOP('',(#10854,#10855,#10856,#10857,#10858,#10859));
#4793=EDGE_LOOP('',(#10860,#10861,#10862,#10863));
#4794=EDGE_LOOP('',(#10864,#10865,#10866,#10867));
#4795=EDGE_LOOP('',(#10868,#10869,#10870,#10871));
#4796=EDGE_LOOP('',(#10872,#10873,#10874,#10875));
#4797=EDGE_LOOP('',(#10876,#10877,#10878,#10879));
#4798=EDGE_LOOP('',(#10880,#10881,#10882,#10883));
#4799=EDGE_LOOP('',(#10884,#10885,#10886,#10887));
#4800=EDGE_LOOP('',(#10888,#10889,#10890,#10891));
#4801=EDGE_LOOP('',(#10892,#10893,#10894,#10895));
#4802=EDGE_LOOP('',(#10896,#10897,#10898,#10899));
#4803=EDGE_LOOP('',(#10900,#10901,#10902,#10903));
#4804=EDGE_LOOP('',(#10904,#10905,#10906,#10907));
#4805=EDGE_LOOP('',(#10908,#10909,#10910,#10911));
#4806=EDGE_LOOP('',(#10912,#10913,#10914,#10915));
#4807=EDGE_LOOP('',(#10916,#10917,#10918,#10919));
#4808=EDGE_LOOP('',(#10920,#10921,#10922,#10923));
#4809=EDGE_LOOP('',(#10924,#10925,#10926,#10927));
#4810=EDGE_LOOP('',(#10928,#10929,#10930,#10931));
#4811=EDGE_LOOP('',(#10932,#10933,#10934,#10935));
#4812=EDGE_LOOP('',(#10936,#10937,#10938,#10939,#10940,#10941));
#4813=EDGE_LOOP('',(#10942,#10943,#10944,#10945));
#4814=EDGE_LOOP('',(#10946,#10947,#10948,#10949));
#4815=EDGE_LOOP('',(#10950,#10951,#10952,#10953,#10954));
#4816=EDGE_LOOP('',(#10955,#10956,#10957,#10958));
#4817=EDGE_LOOP('',(#10959,#10960,#10961,#10962));
#4818=EDGE_LOOP('',(#10963,#10964,#10965,#10966));
#4819=EDGE_LOOP('',(#10967,#10968,#10969,#10970));
#4820=EDGE_LOOP('',(#10971,#10972,#10973,#10974));
#4821=EDGE_LOOP('',(#10975,#10976,#10977,#10978));
#4822=EDGE_LOOP('',(#10979,#10980,#10981,#10982));
#4823=EDGE_LOOP('',(#10983,#10984,#10985,#10986));
#4824=EDGE_LOOP('',(#10987,#10988,#10989,#10990));
#4825=EDGE_LOOP('',(#10991,#10992,#10993,#10994,#10995,#10996,#10997,#10998));
#4826=EDGE_LOOP('',(#10999,#11000,#11001,#11002,#11003,#11004,#11005,#11006));
#4827=EDGE_LOOP('',(#11007,#11008,#11009,#11010,#11011,#11012,#11013,#11014));
#4828=EDGE_LOOP('',(#11015));
#4829=EDGE_LOOP('',(#11016,#11017,#11018,#11019));
#4830=EDGE_LOOP('',(#11020,#11021,#11022,#11023,#11024));
#4831=EDGE_LOOP('',(#11025,#11026,#11027,#11028,#11029,#11030,#11031));
#4832=EDGE_LOOP('',(#11032));
#4833=EDGE_LOOP('',(#11033,#11034,#11035,#11036,#11037,#11038,#11039,#11040));
#4834=EDGE_LOOP('',(#11041,#11042));
#4835=EDGE_LOOP('',(#11043,#11044,#11045,#11046,#11047,#11048));
#4836=EDGE_LOOP('',(#11049,#11050,#11051,#11052,#11053,#11054,#11055,#11056));
#4837=EDGE_LOOP('',(#11057,#11058,#11059,#11060,#11061,#11062,#11063,#11064,
#11065,#11066,#11067,#11068,#11069,#11070,#11071));
#4838=EDGE_LOOP('',(#11072,#11073,#11074,#11075,#11076,#11077,#11078,#11079));
#4839=EDGE_LOOP('',(#11080,#11081,#11082,#11083));
#4840=EDGE_LOOP('',(#11084,#11085,#11086,#11087));
#4841=EDGE_LOOP('',(#11088,#11089,#11090,#11091));
#4842=EDGE_LOOP('',(#11092,#11093,#11094,#11095,#11096,#11097,#11098));
#4843=EDGE_LOOP('',(#11099,#11100,#11101,#11102));
#4844=EDGE_LOOP('',(#11103,#11104,#11105,#11106));
#4845=EDGE_LOOP('',(#11107,#11108,#11109,#11110));
#4846=EDGE_LOOP('',(#11111,#11112,#11113,#11114,#11115,#11116,#11117));
#4847=EDGE_LOOP('',(#11118,#11119,#11120,#11121,#11122));
#4848=EDGE_LOOP('',(#11123,#11124,#11125,#11126));
#4849=EDGE_LOOP('',(#11127,#11128,#11129,#11130,#11131));
#4850=EDGE_LOOP('',(#11132,#11133,#11134,#11135));
#4851=EDGE_LOOP('',(#11136,#11137,#11138,#11139));
#4852=EDGE_LOOP('',(#11140,#11141,#11142,#11143));
#4853=EDGE_LOOP('',(#11144,#11145,#11146,#11147));
#4854=EDGE_LOOP('',(#11148,#11149,#11150,#11151,#11152));
#4855=EDGE_LOOP('',(#11153,#11154,#11155,#11156));
#4856=EDGE_LOOP('',(#11157,#11158,#11159,#11160,#11161));
#4857=EDGE_LOOP('',(#11162,#11163,#11164,#11165,#11166,#11167));
#4858=EDGE_LOOP('',(#11168,#11169,#11170,#11171,#11172,#11173,#11174,#11175));
#4859=EDGE_LOOP('',(#11176,#11177,#11178,#11179,#11180));
#4860=EDGE_LOOP('',(#11181,#11182,#11183,#11184,#11185));
#4861=EDGE_LOOP('',(#11186,#11187,#11188,#11189));
#4862=EDGE_LOOP('',(#11190,#11191,#11192,#11193,#11194,#11195,#11196,#11197));
#4863=EDGE_LOOP('',(#11198,#11199,#11200,#11201,#11202,#11203));
#4864=EDGE_LOOP('',(#11204,#11205,#11206,#11207,#11208,#11209,#11210,#11211,
#11212,#11213,#11214,#11215,#11216,#11217,#11218,#11219,#11220,#11221));
#4865=EDGE_LOOP('',(#11222,#11223,#11224,#11225,#11226,#11227,#11228,#11229));
#4866=EDGE_LOOP('',(#11230,#11231,#11232,#11233,#11234,#11235,#11236,#11237));
#4867=EDGE_LOOP('',(#11238,#11239,#11240,#11241,#11242));
#4868=EDGE_LOOP('',(#11243,#11244,#11245,#11246,#11247));
#4869=EDGE_LOOP('',(#11248,#11249,#11250,#11251));
#4870=EDGE_LOOP('',(#11252,#11253,#11254,#11255));
#4871=EDGE_LOOP('',(#11256,#11257,#11258,#11259,#11260,#11261));
#4872=EDGE_LOOP('',(#11262,#11263,#11264,#11265));
#4873=EDGE_LOOP('',(#11266,#11267,#11268,#11269,#11270,#11271));
#4874=EDGE_LOOP('',(#11272,#11273,#11274,#11275));
#4875=EDGE_LOOP('',(#11276,#11277,#11278,#11279));
#4876=EDGE_LOOP('',(#11280,#11281,#11282,#11283));
#4877=EDGE_LOOP('',(#11284,#11285,#11286,#11287));
#4878=EDGE_LOOP('',(#11288,#11289,#11290,#11291));
#4879=EDGE_LOOP('',(#11292,#11293,#11294,#11295));
#4880=EDGE_LOOP('',(#11296,#11297,#11298,#11299));
#4881=EDGE_LOOP('',(#11300,#11301,#11302,#11303));
#4882=EDGE_LOOP('',(#11304,#11305,#11306,#11307));
#4883=EDGE_LOOP('',(#11308,#11309,#11310,#11311,#11312,#11313));
#4884=EDGE_LOOP('',(#11314,#11315,#11316,#11317,#11318));
#4885=EDGE_LOOP('',(#11319,#11320,#11321,#11322,#11323,#11324,#11325,#11326,
#11327,#11328,#11329,#11330));
#4886=EDGE_LOOP('',(#11331,#11332,#11333,#11334,#11335,#11336));
#4887=EDGE_LOOP('',(#11337,#11338,#11339,#11340));
#4888=EDGE_LOOP('',(#11341,#11342,#11343,#11344));
#4889=EDGE_LOOP('',(#11345,#11346,#11347,#11348));
#4890=EDGE_LOOP('',(#11349,#11350,#11351,#11352,#11353,#11354));
#4891=EDGE_LOOP('',(#11355,#11356,#11357,#11358));
#4892=EDGE_LOOP('',(#11359,#11360,#11361,#11362));
#4893=EDGE_LOOP('',(#11363,#11364,#11365,#11366,#11367,#11368));
#4894=EDGE_LOOP('',(#11369,#11370,#11371,#11372));
#4895=EDGE_LOOP('',(#11373,#11374,#11375,#11376,#11377,#11378));
#4896=EDGE_LOOP('',(#11379,#11380,#11381,#11382));
#4897=EDGE_LOOP('',(#11383,#11384,#11385,#11386,#11387,#11388,#11389,#11390,
#11391,#11392,#11393,#11394,#11395,#11396,#11397,#11398));
#4898=EDGE_LOOP('',(#11399,#11400,#11401,#11402));
#4899=EDGE_LOOP('',(#11403,#11404,#11405,#11406));
#4900=EDGE_LOOP('',(#11407,#11408,#11409,#11410));
#4901=EDGE_LOOP('',(#11411,#11412,#11413,#11414,#11415,#11416,#11417,#11418));
#4902=EDGE_LOOP('',(#11419,#11420,#11421,#11422,#11423,#11424,#11425,#11426));
#4903=EDGE_LOOP('',(#11427,#11428,#11429,#11430,#11431,#11432,#11433,#11434,
#11435));
#4904=EDGE_LOOP('',(#11436,#11437,#11438,#11439,#11440,#11441,#11442));
#4905=EDGE_LOOP('',(#11443,#11444,#11445,#11446,#11447));
#4906=EDGE_LOOP('',(#11448,#11449,#11450,#11451,#11452));
#4907=EDGE_LOOP('',(#11453,#11454,#11455,#11456));
#4908=EDGE_LOOP('',(#11457,#11458,#11459,#11460,#11461));
#4909=EDGE_LOOP('',(#11462,#11463,#11464,#11465,#11466,#11467));
#4910=EDGE_LOOP('',(#11468,#11469,#11470,#11471,#11472,#11473,#11474,#11475,
#11476,#11477,#11478,#11479,#11480,#11481,#11482));
#4911=EDGE_LOOP('',(#11483,#11484,#11485,#11486,#11487,#11488,#11489,#11490,
#11491,#11492,#11493,#11494,#11495,#11496,#11497));
#4912=EDGE_LOOP('',(#11498,#11499,#11500));
#4913=EDGE_LOOP('',(#11501,#11502,#11503,#11504,#11505));
#4914=EDGE_LOOP('',(#11506,#11507,#11508,#11509));
#4915=EDGE_LOOP('',(#11510,#11511,#11512,#11513));
#4916=EDGE_LOOP('',(#11514,#11515,#11516,#11517));
#4917=EDGE_LOOP('',(#11518,#11519,#11520,#11521,#11522,#11523,#11524,#11525,
#11526,#11527,#11528,#11529,#11530,#11531));
#4918=EDGE_LOOP('',(#11532,#11533,#11534,#11535,#11536,#11537,#11538,#11539));
#4919=EDGE_LOOP('',(#11540,#11541,#11542,#11543));
#4920=EDGE_LOOP('',(#11544,#11545,#11546,#11547));
#4921=EDGE_LOOP('',(#11548,#11549,#11550,#11551));
#4922=EDGE_LOOP('',(#11552,#11553,#11554,#11555,#11556,#11557,#11558,#11559,
#11560,#11561,#11562));
#4923=EDGE_LOOP('',(#11563,#11564,#11565,#11566,#11567));
#4924=EDGE_LOOP('',(#11568,#11569,#11570,#11571,#11572));
#4925=EDGE_LOOP('',(#11573,#11574,#11575,#11576,#11577));
#4926=EDGE_LOOP('',(#11578,#11579,#11580,#11581,#11582));
#4927=EDGE_LOOP('',(#11583,#11584,#11585,#11586,#11587,#11588,#11589,#11590,
#11591,#11592,#11593,#11594,#11595,#11596,#11597,#11598,#11599,#11600));
#4928=EDGE_LOOP('',(#11601,#11602,#11603,#11604,#11605,#11606,#11607));
#4929=EDGE_LOOP('',(#11608,#11609,#11610,#11611));
#4930=EDGE_LOOP('',(#11612,#11613,#11614,#11615));
#4931=EDGE_LOOP('',(#11616,#11617,#11618,#11619));
#4932=EDGE_LOOP('',(#11620,#11621,#11622,#11623,#11624,#11625));
#4933=EDGE_LOOP('',(#11626,#11627,#11628,#11629,#11630));
#4934=EDGE_LOOP('',(#11631,#11632,#11633,#11634,#11635,#11636));
#4935=EDGE_LOOP('',(#11637,#11638,#11639,#11640));
#4936=EDGE_LOOP('',(#11641,#11642,#11643,#11644));
#4937=EDGE_LOOP('',(#11645,#11646));
#4938=EDGE_LOOP('',(#11647,#11648,#11649,#11650,#11651));
#4939=EDGE_LOOP('',(#11652,#11653,#11654,#11655,#11656));
#4940=EDGE_LOOP('',(#11657,#11658));
#4941=EDGE_LOOP('',(#11659,#11660,#11661,#11662,#11663,#11664));
#4942=EDGE_LOOP('',(#11665,#11666,#11667,#11668));
#4943=EDGE_LOOP('',(#11669,#11670,#11671,#11672));
#4944=EDGE_LOOP('',(#11673,#11674,#11675,#11676));
#4945=EDGE_LOOP('',(#11677,#11678,#11679,#11680));
#4946=EDGE_LOOP('',(#11681,#11682,#11683,#11684));
#4947=EDGE_LOOP('',(#11685,#11686,#11687,#11688));
#4948=EDGE_LOOP('',(#11689,#11690,#11691,#11692));
#4949=EDGE_LOOP('',(#11693,#11694,#11695));
#4950=EDGE_LOOP('',(#11696,#11697,#11698,#11699));
#4951=EDGE_LOOP('',(#11700,#11701,#11702,#11703));
#4952=EDGE_LOOP('',(#11704,#11705,#11706,#11707));
#4953=EDGE_LOOP('',(#11708,#11709,#11710,#11711));
#4954=EDGE_LOOP('',(#11712,#11713,#11714,#11715));
#4955=EDGE_LOOP('',(#11716,#11717,#11718,#11719));
#4956=EDGE_LOOP('',(#11720,#11721,#11722,#11723));
#4957=EDGE_LOOP('',(#11724,#11725,#11726,#11727));
#4958=EDGE_LOOP('',(#11728,#11729,#11730,#11731));
#4959=EDGE_LOOP('',(#11732,#11733,#11734,#11735));
#4960=EDGE_LOOP('',(#11736,#11737,#11738,#11739));
#4961=EDGE_LOOP('',(#11740,#11741,#11742,#11743));
#4962=EDGE_LOOP('',(#11744,#11745,#11746,#11747));
#4963=EDGE_LOOP('',(#11748,#11749,#11750,#11751));
#4964=EDGE_LOOP('',(#11752,#11753,#11754,#11755,#11756));
#4965=EDGE_LOOP('',(#11757,#11758,#11759,#11760,#11761,#11762));
#4966=EDGE_LOOP('',(#11763,#11764,#11765));
#4967=EDGE_LOOP('',(#11766,#11767,#11768,#11769));
#4968=EDGE_LOOP('',(#11770,#11771,#11772,#11773,#11774,#11775));
#4969=EDGE_LOOP('',(#11776,#11777,#11778));
#4970=EDGE_LOOP('',(#11779,#11780,#11781));
#4971=EDGE_LOOP('',(#11782,#11783,#11784));
#4972=EDGE_LOOP('',(#11785,#11786,#11787,#11788));
#4973=EDGE_LOOP('',(#11789,#11790,#11791,#11792));
#4974=EDGE_LOOP('',(#11793,#11794,#11795,#11796,#11797));
#4975=EDGE_LOOP('',(#11798,#11799,#11800,#11801));
#4976=EDGE_LOOP('',(#11802,#11803,#11804,#11805));
#4977=EDGE_LOOP('',(#11806,#11807,#11808,#11809,#11810,#11811));
#4978=EDGE_LOOP('',(#11812,#11813,#11814,#11815,#11816));
#4979=EDGE_LOOP('',(#11817,#11818,#11819,#11820));
#4980=EDGE_LOOP('',(#11821));
#4981=EDGE_LOOP('',(#11822,#11823));
#4982=EDGE_LOOP('',(#11824,#11825,#11826,#11827));
#4983=EDGE_LOOP('',(#11828,#11829,#11830,#11831,#11832));
#4984=EDGE_LOOP('',(#11833,#11834,#11835,#11836,#11837));
#4985=EDGE_LOOP('',(#11838,#11839,#11840,#11841));
#4986=EDGE_LOOP('',(#11842,#11843,#11844,#11845));
#4987=EDGE_LOOP('',(#11846,#11847,#11848,#11849));
#4988=EDGE_LOOP('',(#11850,#11851,#11852,#11853));
#4989=EDGE_LOOP('',(#11854,#11855,#11856,#11857));
#4990=EDGE_LOOP('',(#11858,#11859,#11860,#11861,#11862));
#4991=EDGE_LOOP('',(#11863,#11864,#11865,#11866));
#4992=EDGE_LOOP('',(#11867,#11868,#11869,#11870));
#4993=EDGE_LOOP('',(#11871,#11872,#11873,#11874));
#4994=EDGE_LOOP('',(#11875,#11876,#11877,#11878));
#4995=EDGE_LOOP('',(#11879,#11880,#11881,#11882,#11883));
#4996=EDGE_LOOP('',(#11884,#11885,#11886));
#4997=EDGE_LOOP('',(#11887,#11888,#11889,#11890));
#4998=EDGE_LOOP('',(#11891,#11892,#11893,#11894,#11895,#11896,#11897,#11898));
#4999=EDGE_LOOP('',(#11899,#11900,#11901,#11902));
#5000=EDGE_LOOP('',(#11903,#11904,#11905,#11906));
#5001=EDGE_LOOP('',(#11907,#11908,#11909,#11910));
#5002=EDGE_LOOP('',(#11911,#11912,#11913,#11914));
#5003=EDGE_LOOP('',(#11915,#11916,#11917,#11918));
#5004=EDGE_LOOP('',(#11919,#11920,#11921,#11922));
#5005=EDGE_LOOP('',(#11923,#11924,#11925,#11926));
#5006=EDGE_LOOP('',(#11927,#11928,#11929,#11930));
#5007=EDGE_LOOP('',(#11931,#11932,#11933,#11934,#11935));
#5008=EDGE_LOOP('',(#11936,#11937,#11938,#11939,#11940));
#5009=EDGE_LOOP('',(#11941,#11942,#11943,#11944,#11945,#11946,#11947,#11948));
#5010=EDGE_LOOP('',(#11949,#11950,#11951));
#5011=EDGE_LOOP('',(#11952,#11953,#11954,#11955,#11956,#11957));
#5012=EDGE_LOOP('',(#11958,#11959,#11960,#11961));
#5013=EDGE_LOOP('',(#11962,#11963,#11964,#11965));
#5014=EDGE_LOOP('',(#11966,#11967,#11968,#11969));
#5015=EDGE_LOOP('',(#11970));
#5016=EDGE_LOOP('',(#11971,#11972,#11973,#11974,#11975,#11976,#11977,#11978));
#5017=EDGE_LOOP('',(#11979));
#5018=EDGE_LOOP('',(#11980,#11981,#11982,#11983));
#5019=EDGE_LOOP('',(#11984,#11985,#11986,#11987));
#5020=EDGE_LOOP('',(#11988,#11989,#11990,#11991));
#5021=EDGE_LOOP('',(#11992,#11993,#11994,#11995,#11996,#11997,#11998,#11999,
#12000,#12001,#12002,#12003,#12004,#12005,#12006));
#5022=EDGE_LOOP('',(#12007,#12008,#12009,#12010));
#5023=EDGE_LOOP('',(#12011,#12012,#12013,#12014));
#5024=EDGE_LOOP('',(#12015,#12016,#12017,#12018));
#5025=EDGE_LOOP('',(#12019,#12020,#12021,#12022));
#5026=EDGE_LOOP('',(#12023,#12024,#12025,#12026));
#5027=EDGE_LOOP('',(#12027,#12028,#12029,#12030));
#5028=EDGE_LOOP('',(#12031,#12032,#12033,#12034,#12035,#12036));
#5029=EDGE_LOOP('',(#12037,#12038,#12039,#12040));
#5030=EDGE_LOOP('',(#12041,#12042,#12043,#12044));
#5031=EDGE_LOOP('',(#12045,#12046,#12047,#12048));
#5032=EDGE_LOOP('',(#12049,#12050,#12051,#12052));
#5033=EDGE_LOOP('',(#12053,#12054,#12055,#12056));
#5034=EDGE_LOOP('',(#12057,#12058,#12059,#12060));
#5035=EDGE_LOOP('',(#12061,#12062,#12063,#12064,#12065));
#5036=EDGE_LOOP('',(#12066,#12067,#12068));
#5037=EDGE_LOOP('',(#12069,#12070,#12071,#12072,#12073));
#5038=EDGE_LOOP('',(#12074,#12075,#12076,#12077));
#5039=EDGE_LOOP('',(#12078,#12079,#12080,#12081,#12082));
#5040=EDGE_LOOP('',(#12083,#12084,#12085,#12086));
#5041=EDGE_LOOP('',(#12087,#12088,#12089,#12090));
#5042=EDGE_LOOP('',(#12091,#12092,#12093,#12094,#12095,#12096,#12097));
#5043=EDGE_LOOP('',(#12098));
#5044=EDGE_LOOP('',(#12099,#12100,#12101,#12102,#12103));
#5045=EDGE_LOOP('',(#12104,#12105,#12106,#12107,#12108));
#5046=EDGE_LOOP('',(#12109,#12110,#12111,#12112));
#5047=EDGE_LOOP('',(#12113,#12114,#12115,#12116));
#5048=EDGE_LOOP('',(#12117,#12118,#12119,#12120));
#5049=EDGE_LOOP('',(#12121,#12122,#12123,#12124,#12125,#12126,#12127,#12128,
#12129,#12130,#12131,#12132,#12133,#12134,#12135,#12136,#12137,#12138,#12139,
#12140,#12141,#12142,#12143,#12144,#12145,#12146,#12147,#12148,#12149,#12150,
#12151));
#5050=EDGE_LOOP('',(#12152));
#5051=EDGE_LOOP('',(#12153,#12154,#12155,#12156,#12157));
#5052=EDGE_LOOP('',(#12158,#12159,#12160,#12161));
#5053=EDGE_LOOP('',(#12162,#12163,#12164,#12165));
#5054=EDGE_LOOP('',(#12166,#12167,#12168,#12169));
#5055=EDGE_LOOP('',(#12170,#12171,#12172,#12173));
#5056=EDGE_LOOP('',(#12174,#12175,#12176,#12177));
#5057=EDGE_LOOP('',(#12178,#12179,#12180,#12181));
#5058=EDGE_LOOP('',(#12182,#12183,#12184,#12185));
#5059=EDGE_LOOP('',(#12186,#12187,#12188,#12189));
#5060=EDGE_LOOP('',(#12190,#12191,#12192,#12193));
#5061=EDGE_LOOP('',(#12194,#12195,#12196,#12197));
#5062=EDGE_LOOP('',(#12198,#12199,#12200,#12201));
#5063=EDGE_LOOP('',(#12202,#12203,#12204,#12205,#12206));
#5064=EDGE_LOOP('',(#12207,#12208,#12209,#12210,#12211));
#5065=EDGE_LOOP('',(#12212,#12213,#12214,#12215,#12216,#12217));
#5066=EDGE_LOOP('',(#12218,#12219,#12220,#12221,#12222));
#5067=EDGE_LOOP('',(#12223,#12224,#12225,#12226));
#5068=EDGE_LOOP('',(#12227,#12228,#12229,#12230));
#5069=EDGE_LOOP('',(#12231,#12232,#12233,#12234));
#5070=EDGE_LOOP('',(#12235));
#5071=EDGE_LOOP('',(#12236));
#5072=EDGE_LOOP('',(#12237));
#5073=EDGE_LOOP('',(#12238,#12239,#12240,#12241,#12242,#12243,#12244,#12245,
#12246,#12247,#12248,#12249));
#5074=EDGE_LOOP('',(#12250,#12251,#12252,#12253,#12254));
#5075=EDGE_LOOP('',(#12255,#12256,#12257,#12258));
#5076=EDGE_LOOP('',(#12259,#12260,#12261,#12262,#12263));
#5077=EDGE_LOOP('',(#12264));
#5078=EDGE_LOOP('',(#12265));
#5079=EDGE_LOOP('',(#12266,#12267,#12268,#12269));
#5080=EDGE_LOOP('',(#12270,#12271,#12272,#12273));
#5081=EDGE_LOOP('',(#12274,#12275,#12276,#12277));
#5082=EDGE_LOOP('',(#12278,#12279,#12280,#12281));
#5083=EDGE_LOOP('',(#12282,#12283,#12284,#12285));
#5084=EDGE_LOOP('',(#12286,#12287,#12288,#12289));
#5085=EDGE_LOOP('',(#12290,#12291,#12292,#12293));
#5086=EDGE_LOOP('',(#12294,#12295,#12296,#12297));
#5087=EDGE_LOOP('',(#12298,#12299,#12300,#12301));
#5088=EDGE_LOOP('',(#12302,#12303,#12304,#12305));
#5089=EDGE_LOOP('',(#12306,#12307,#12308,#12309));
#5090=EDGE_LOOP('',(#12310,#12311,#12312,#12313));
#5091=EDGE_LOOP('',(#12314,#12315,#12316,#12317,#12318,#12319,#12320,#12321,
#12322,#12323,#12324,#12325));
#5092=EDGE_LOOP('',(#12326));
#5093=EDGE_LOOP('',(#12327,#12328,#12329,#12330,#12331,#12332,#12333,#12334,
#12335,#12336,#12337,#12338));
#5094=EDGE_LOOP('',(#12339,#12340,#12341,#12342,#12343,#12344,#12345,#12346));
#5095=EDGE_LOOP('',(#12347,#12348,#12349,#12350,#12351,#12352,#12353,#12354,
#12355,#12356,#12357,#12358,#12359,#12360,#12361,#12362,#12363,#12364,#12365,
#12366));
#5096=EDGE_LOOP('',(#12367,#12368,#12369,#12370,#12371,#12372,#12373,#12374,
#12375,#12376,#12377,#12378));
#5097=EDGE_LOOP('',(#12379,#12380,#12381,#12382,#12383,#12384,#12385,#12386,
#12387,#12388,#12389,#12390));
#5098=EDGE_LOOP('',(#12391,#12392,#12393,#12394,#12395,#12396,#12397,#12398,
#12399,#12400,#12401,#12402));
#5099=EDGE_LOOP('',(#12403,#12404,#12405,#12406));
#5100=EDGE_LOOP('',(#12407,#12408,#12409,#12410));
#5101=EDGE_LOOP('',(#12411,#12412,#12413,#12414));
#5102=EDGE_LOOP('',(#12415,#12416,#12417,#12418));
#5103=EDGE_LOOP('',(#12419,#12420,#12421,#12422));
#5104=EDGE_LOOP('',(#12423,#12424,#12425,#12426));
#5105=EDGE_LOOP('',(#12427,#12428,#12429,#12430,#12431,#12432,#12433,#12434));
#5106=EDGE_LOOP('',(#12435,#12436,#12437,#12438));
#5107=EDGE_LOOP('',(#12439,#12440,#12441,#12442));
#5108=EDGE_LOOP('',(#12443,#12444,#12445,#12446,#12447,#12448,#12449,#12450));
#5109=EDGE_LOOP('',(#12451,#12452,#12453,#12454));
#5110=EDGE_LOOP('',(#12455,#12456,#12457,#12458));
#5111=EDGE_LOOP('',(#12459,#12460,#12461,#12462,#12463,#12464,#12465,#12466));
#5112=EDGE_LOOP('',(#12467));
#5113=EDGE_LOOP('',(#12468));
#5114=EDGE_LOOP('',(#12469,#12470,#12471,#12472));
#5115=EDGE_LOOP('',(#12473,#12474,#12475,#12476));
#5116=EDGE_LOOP('',(#12477,#12478,#12479,#12480));
#5117=EDGE_LOOP('',(#12481,#12482,#12483,#12484,#12485,#12486,#12487,#12488));
#5118=EDGE_LOOP('',(#12489,#12490,#12491,#12492,#12493,#12494));
#5119=EDGE_LOOP('',(#12495,#12496,#12497,#12498));
#5120=EDGE_LOOP('',(#12499,#12500,#12501,#12502,#12503,#12504,#12505,#12506,
#12507));
#5121=EDGE_LOOP('',(#12508,#12509,#12510,#12511));
#5122=EDGE_LOOP('',(#12512,#12513,#12514,#12515));
#5123=EDGE_LOOP('',(#12516,#12517,#12518,#12519));
#5124=EDGE_LOOP('',(#12520,#12521,#12522,#12523,#12524,#12525,#12526,#12527,
#12528));
#5125=EDGE_LOOP('',(#12529,#12530,#12531,#12532,#12533,#12534));
#5126=EDGE_LOOP('',(#12535,#12536,#12537,#12538,#12539,#12540,#12541,#12542));
#5127=EDGE_LOOP('',(#12543,#12544,#12545,#12546));
#5128=EDGE_LOOP('',(#12547,#12548,#12549,#12550));
#5129=EDGE_LOOP('',(#12551,#12552,#12553,#12554));
#5130=EDGE_LOOP('',(#12555,#12556,#12557,#12558));
#5131=EDGE_LOOP('',(#12559,#12560,#12561,#12562));
#5132=EDGE_LOOP('',(#12563,#12564,#12565,#12566,#12567,#12568,#12569,#12570,
#12571,#12572));
#5133=EDGE_LOOP('',(#12573,#12574,#12575,#12576));
#5134=EDGE_LOOP('',(#12577,#12578,#12579,#12580,#12581,#12582,#12583,#12584));
#5135=EDGE_LOOP('',(#12585,#12586,#12587,#12588,#12589,#12590,#12591,#12592,
#12593,#12594));
#5136=EDGE_LOOP('',(#12595,#12596,#12597,#12598,#12599,#12600,#12601,#12602));
#5137=EDGE_LOOP('',(#12603,#12604,#12605,#12606));
#5138=EDGE_LOOP('',(#12607,#12608,#12609,#12610));
#5139=EDGE_LOOP('',(#12611,#12612,#12613,#12614));
#5140=EDGE_LOOP('',(#12615,#12616,#12617,#12618));
#5141=EDGE_LOOP('',(#12619,#12620,#12621,#12622,#12623,#12624,#12625,#12626,
#12627,#12628));
#5142=EDGE_LOOP('',(#12629,#12630,#12631,#12632));
#5143=EDGE_LOOP('',(#12633,#12634,#12635,#12636,#12637,#12638,#12639,#12640));
#5144=EDGE_LOOP('',(#12641,#12642,#12643,#12644,#12645,#12646,#12647,#12648,
#12649,#12650));
#5145=EDGE_LOOP('',(#12651,#12652,#12653,#12654,#12655,#12656,#12657,#12658,
#12659));
#5146=EDGE_LOOP('',(#12660,#12661,#12662,#12663,#12664,#12665,#12666,#12667,
#12668));
#5147=EDGE_LOOP('',(#12669,#12670,#12671,#12672,#12673,#12674,#12675,#12676));
#5148=EDGE_LOOP('',(#12677,#12678,#12679,#12680));
#5149=EDGE_LOOP('',(#12681,#12682,#12683,#12684));
#5150=EDGE_LOOP('',(#12685,#12686,#12687,#12688));
#5151=EDGE_LOOP('',(#12689,#12690,#12691,#12692));
#5152=EDGE_LOOP('',(#12693,#12694,#12695,#12696,#12697,#12698,#12699,#12700));
#5153=EDGE_LOOP('',(#12701,#12702,#12703,#12704,#12705,#12706));
#5154=EDGE_LOOP('',(#12707,#12708,#12709,#12710));
#5155=EDGE_LOOP('',(#12711,#12712,#12713,#12714));
#5156=EDGE_LOOP('',(#12715,#12716,#12717,#12718));
#5157=EDGE_LOOP('',(#12719,#12720,#12721,#12722));
#5158=EDGE_LOOP('',(#12723,#12724,#12725,#12726,#12727,#12728));
#5159=EDGE_LOOP('',(#12729,#12730,#12731,#12732,#12733,#12734,#12735,#12736));
#5160=EDGE_LOOP('',(#12737,#12738,#12739,#12740));
#5161=EDGE_LOOP('',(#12741,#12742,#12743,#12744));
#5162=EDGE_LOOP('',(#12745));
#5163=EDGE_LOOP('',(#12746));
#5164=EDGE_LOOP('',(#12747));
#5165=EDGE_LOOP('',(#12748));
#5166=EDGE_LOOP('',(#12749));
#5167=EDGE_LOOP('',(#12750));
#5168=EDGE_LOOP('',(#12751,#12752,#12753,#12754));
#5169=EDGE_LOOP('',(#12755,#12756,#12757,#12758));
#5170=EDGE_LOOP('',(#12759,#12760,#12761,#12762));
#5171=EDGE_LOOP('',(#12763,#12764,#12765,#12766));
#5172=EDGE_LOOP('',(#12767,#12768,#12769,#12770));
#5173=EDGE_LOOP('',(#12771,#12772,#12773,#12774));
#5174=EDGE_LOOP('',(#12775,#12776,#12777,#12778));
#5175=EDGE_LOOP('',(#12779,#12780,#12781,#12782,#12783,#12784,#12785,#12786));
#5176=EDGE_LOOP('',(#12787));
#5177=EDGE_LOOP('',(#12788,#12789,#12790,#12791));
#5178=EDGE_LOOP('',(#12792,#12793,#12794,#12795,#12796,#12797,#12798,#12799));
#5179=EDGE_LOOP('',(#12800,#12801,#12802,#12803));
#5180=EDGE_LOOP('',(#12804,#12805,#12806,#12807));
#5181=EDGE_LOOP('',(#12808,#12809,#12810,#12811));
#5182=EDGE_LOOP('',(#12812,#12813,#12814,#12815));
#5183=EDGE_LOOP('',(#12816));
#5184=EDGE_LOOP('',(#12817,#12818,#12819,#12820));
#5185=EDGE_LOOP('',(#12821,#12822,#12823,#12824));
#5186=EDGE_LOOP('',(#12825,#12826,#12827,#12828,#12829,#12830,#12831,#12832,
#12833));
#5187=EDGE_LOOP('',(#12834,#12835));
#5188=EDGE_LOOP('',(#12836,#12837,#12838,#12839));
#5189=EDGE_LOOP('',(#12840,#12841,#12842,#12843));
#5190=EDGE_LOOP('',(#12844,#12845,#12846,#12847,#12848,#12849));
#5191=EDGE_LOOP('',(#12850,#12851,#12852,#12853));
#5192=EDGE_LOOP('',(#12854,#12855,#12856,#12857,#12858));
#5193=EDGE_LOOP('',(#12859,#12860,#12861,#12862));
#5194=EDGE_LOOP('',(#12863,#12864,#12865,#12866));
#5195=EDGE_LOOP('',(#12867,#12868,#12869,#12870));
#5196=EDGE_LOOP('',(#12871,#12872,#12873,#12874));
#5197=EDGE_LOOP('',(#12875,#12876,#12877,#12878));
#5198=EDGE_LOOP('',(#12879,#12880,#12881,#12882));
#5199=EDGE_LOOP('',(#12883,#12884,#12885,#12886));
#5200=EDGE_LOOP('',(#12887,#12888,#12889,#12890));
#5201=EDGE_LOOP('',(#12891,#12892,#12893,#12894));
#5202=EDGE_LOOP('',(#12895));
#5203=EDGE_LOOP('',(#12896));
#5204=EDGE_LOOP('',(#12897));
#5205=EDGE_LOOP('',(#12898));
#5206=EDGE_LOOP('',(#12899));
#5207=EDGE_LOOP('',(#12900));
#5208=EDGE_LOOP('',(#12901,#12902,#12903,#12904));
#5209=EDGE_LOOP('',(#12905,#12906,#12907,#12908));
#5210=EDGE_LOOP('',(#12909,#12910,#12911,#12912));
#5211=EDGE_LOOP('',(#12913,#12914,#12915,#12916,#12917));
#5212=EDGE_LOOP('',(#12918,#12919,#12920,#12921));
#5213=EDGE_LOOP('',(#12922,#12923,#12924,#12925));
#5214=EDGE_LOOP('',(#12926,#12927,#12928,#12929));
#5215=EDGE_LOOP('',(#12930,#12931,#12932,#12933));
#5216=EDGE_LOOP('',(#12934,#12935,#12936,#12937));
#5217=EDGE_LOOP('',(#12938,#12939,#12940,#12941));
#5218=EDGE_LOOP('',(#12942,#12943,#12944,#12945));
#5219=EDGE_LOOP('',(#12946,#12947,#12948,#12949));
#5220=EDGE_LOOP('',(#12950,#12951,#12952,#12953));
#5221=EDGE_LOOP('',(#12954));
#5222=EDGE_LOOP('',(#12955,#12956,#12957,#12958,#12959,#12960,#12961,#12962,
#12963,#12964,#12965));
#5223=EDGE_LOOP('',(#12966));
#5224=EDGE_LOOP('',(#12967));
#5225=EDGE_LOOP('',(#12968));
#5226=EDGE_LOOP('',(#12969,#12970,#12971,#12972));
#5227=EDGE_LOOP('',(#12973,#12974,#12975,#12976,#12977,#12978));
#5228=EDGE_LOOP('',(#12979));
#5229=EDGE_LOOP('',(#12980));
#5230=EDGE_LOOP('',(#12981,#12982,#12983,#12984,#12985,#12986,#12987,#12988,
#12989,#12990));
#5231=EDGE_LOOP('',(#12991,#12992,#12993,#12994,#12995));
#5232=EDGE_LOOP('',(#12996,#12997,#12998));
#5233=EDGE_LOOP('',(#12999,#13000,#13001,#13002));
#5234=EDGE_LOOP('',(#13003,#13004,#13005,#13006,#13007,#13008,#13009,#13010));
#5235=EDGE_LOOP('',(#13011));
#5236=EDGE_LOOP('',(#13012));
#5237=EDGE_LOOP('',(#13013));
#5238=EDGE_LOOP('',(#13014,#13015,#13016,#13017,#13018));
#5239=EDGE_LOOP('',(#13019,#13020,#13021,#13022));
#5240=EDGE_LOOP('',(#13023,#13024,#13025,#13026,#13027,#13028,#13029,#13030,
#13031,#13032,#13033,#13034,#13035,#13036,#13037,#13038,#13039));
#5241=EDGE_LOOP('',(#13040));
#5242=EDGE_LOOP('',(#13041));
#5243=EDGE_LOOP('',(#13042,#13043,#13044,#13045));
#5244=EDGE_LOOP('',(#13046,#13047,#13048,#13049,#13050));
#5245=EDGE_LOOP('',(#13051,#13052,#13053,#13054,#13055,#13056,#13057,#13058));
#5246=EDGE_LOOP('',(#13059));
#5247=EDGE_LOOP('',(#13060,#13061,#13062,#13063,#13064));
#5248=EDGE_LOOP('',(#13065,#13066,#13067,#13068));
#5249=EDGE_LOOP('',(#13069,#13070,#13071,#13072,#13073,#13074));
#5250=EDGE_LOOP('',(#13075));
#5251=EDGE_LOOP('',(#13076,#13077,#13078,#13079));
#5252=EDGE_LOOP('',(#13080,#13081,#13082,#13083,#13084,#13085,#13086,#13087,
#13088));
#5253=EDGE_LOOP('',(#13089));
#5254=EDGE_LOOP('',(#13090,#13091,#13092,#13093));
#5255=EDGE_LOOP('',(#13094,#13095,#13096,#13097,#13098,#13099,#13100,#13101,
#13102));
#5256=EDGE_LOOP('',(#13103,#13104,#13105));
#5257=EDGE_LOOP('',(#13106,#13107,#13108,#13109,#13110,#13111,#13112));
#5258=EDGE_LOOP('',(#13113,#13114,#13115,#13116,#13117,#13118));
#5259=EDGE_LOOP('',(#13119,#13120,#13121,#13122));
#5260=EDGE_LOOP('',(#13123,#13124,#13125,#13126,#13127,#13128,#13129,#13130,
#13131,#13132,#13133,#13134,#13135,#13136,#13137));
#5261=EDGE_LOOP('',(#13138,#13139,#13140,#13141,#13142));
#5262=EDGE_LOOP('',(#13143,#13144,#13145,#13146,#13147,#13148,#13149,#13150,
#13151,#13152));
#5263=EDGE_LOOP('',(#13153,#13154,#13155,#13156));
#5264=EDGE_LOOP('',(#13157,#13158,#13159,#13160,#13161,#13162,#13163,#13164,
#13165,#13166,#13167,#13168,#13169,#13170,#13171,#13172,#13173,#13174,#13175,
#13176,#13177,#13178,#13179,#13180,#13181));
#5265=EDGE_LOOP('',(#13182,#13183,#13184,#13185));
#5266=EDGE_LOOP('',(#13186,#13187));
#5267=EDGE_LOOP('',(#13188,#13189,#13190,#13191));
#5268=EDGE_LOOP('',(#13192,#13193,#13194,#13195,#13196,#13197,#13198,#13199));
#5269=EDGE_LOOP('',(#13200,#13201,#13202,#13203));
#5270=EDGE_LOOP('',(#13204,#13205,#13206,#13207));
#5271=EDGE_LOOP('',(#13208,#13209,#13210,#13211,#13212));
#5272=EDGE_LOOP('',(#13213,#13214,#13215,#13216,#13217));
#5273=EDGE_LOOP('',(#13218,#13219,#13220,#13221,#13222,#13223,#13224));
#5274=EDGE_LOOP('',(#13225,#13226,#13227,#13228,#13229,#13230));
#5275=EDGE_LOOP('',(#13231,#13232,#13233,#13234));
#5276=EDGE_LOOP('',(#13235,#13236,#13237,#13238));
#5277=EDGE_LOOP('',(#13239,#13240));
#5278=EDGE_LOOP('',(#13241,#13242));
#5279=EDGE_LOOP('',(#13243,#13244,#13245,#13246,#13247));
#5280=EDGE_LOOP('',(#13248,#13249,#13250,#13251));
#5281=EDGE_LOOP('',(#13252,#13253,#13254,#13255,#13256,#13257,#13258,#13259));
#5282=EDGE_LOOP('',(#13260,#13261,#13262,#13263));
#5283=EDGE_LOOP('',(#13264,#13265,#13266,#13267));
#5284=EDGE_LOOP('',(#13268,#13269,#13270,#13271,#13272,#13273,#13274));
#5285=EDGE_LOOP('',(#13275,#13276,#13277,#13278,#13279,#13280,#13281,#13282,
#13283,#13284,#13285,#13286,#13287));
#5286=EDGE_LOOP('',(#13288,#13289,#13290,#13291,#13292,#13293,#13294));
#5287=EDGE_LOOP('',(#13295,#13296,#13297,#13298,#13299,#13300,#13301,#13302,
#13303,#13304));
#5288=EDGE_LOOP('',(#13305,#13306,#13307,#13308,#13309,#13310));
#5289=EDGE_LOOP('',(#13311,#13312,#13313,#13314));
#5290=EDGE_LOOP('',(#13315,#13316,#13317,#13318));
#5291=EDGE_LOOP('',(#13319,#13320,#13321));
#5292=EDGE_LOOP('',(#13322,#13323,#13324,#13325));
#5293=EDGE_LOOP('',(#13326,#13327,#13328,#13329));
#5294=EDGE_LOOP('',(#13330,#13331,#13332));
#5295=EDGE_LOOP('',(#13333,#13334,#13335,#13336));
#5296=EDGE_LOOP('',(#13337,#13338,#13339));
#5297=EDGE_LOOP('',(#13340,#13341,#13342,#13343));
#5298=EDGE_LOOP('',(#13344,#13345,#13346,#13347,#13348,#13349));
#5299=EDGE_LOOP('',(#13350,#13351,#13352,#13353,#13354));
#5300=EDGE_LOOP('',(#13355,#13356,#13357,#13358,#13359));
#5301=EDGE_LOOP('',(#13360,#13361,#13362,#13363,#13364));
#5302=EDGE_LOOP('',(#13365,#13366,#13367,#13368));
#5303=EDGE_LOOP('',(#13369,#13370,#13371,#13372));
#5304=EDGE_LOOP('',(#13373,#13374,#13375,#13376));
#5305=EDGE_LOOP('',(#13377,#13378,#13379,#13380));
#5306=EDGE_LOOP('',(#13381,#13382,#13383,#13384));
#5307=EDGE_LOOP('',(#13385,#13386,#13387,#13388));
#5308=EDGE_LOOP('',(#13389,#13390,#13391,#13392));
#5309=EDGE_LOOP('',(#13393,#13394,#13395,#13396));
#5310=EDGE_LOOP('',(#13397,#13398,#13399,#13400));
#5311=EDGE_LOOP('',(#13401));
#5312=EDGE_LOOP('',(#13402));
#5313=EDGE_LOOP('',(#13403));
#5314=EDGE_LOOP('',(#13404,#13405,#13406,#13407));
#5315=EDGE_LOOP('',(#13408,#13409,#13410,#13411));
#5316=EDGE_LOOP('',(#13412,#13413,#13414,#13415));
#5317=EDGE_LOOP('',(#13416,#13417,#13418,#13419));
#5318=EDGE_LOOP('',(#13420,#13421,#13422,#13423,#13424,#13425,#13426,#13427));
#5319=EDGE_LOOP('',(#13428));
#5320=EDGE_LOOP('',(#13429));
#5321=EDGE_LOOP('',(#13430));
#5322=EDGE_LOOP('',(#13431,#13432,#13433,#13434));
#5323=EDGE_LOOP('',(#13435,#13436,#13437,#13438));
#5324=EDGE_LOOP('',(#13439,#13440,#13441,#13442));
#5325=EDGE_LOOP('',(#13443,#13444,#13445,#13446));
#5326=EDGE_LOOP('',(#13447,#13448));
#5327=EDGE_LOOP('',(#13449,#13450,#13451,#13452,#13453));
#5328=EDGE_LOOP('',(#13454,#13455,#13456,#13457,#13458));
#5329=EDGE_LOOP('',(#13459,#13460,#13461,#13462,#13463));
#5330=EDGE_LOOP('',(#13464,#13465,#13466,#13467));
#5331=EDGE_LOOP('',(#13468,#13469,#13470,#13471));
#5332=EDGE_LOOP('',(#13472,#13473,#13474,#13475));
#5333=EDGE_LOOP('',(#13476,#13477,#13478,#13479,#13480));
#5334=EDGE_LOOP('',(#13481,#13482));
#5335=EDGE_LOOP('',(#13483));
#5336=EDGE_LOOP('',(#13484,#13485,#13486,#13487));
#5337=EDGE_LOOP('',(#13488,#13489,#13490));
#5338=EDGE_LOOP('',(#13491,#13492,#13493,#13494));
#5339=EDGE_LOOP('',(#13495,#13496,#13497,#13498));
#5340=EDGE_LOOP('',(#13499,#13500,#13501));
#5341=EDGE_LOOP('',(#13502,#13503,#13504,#13505));
#5342=EDGE_LOOP('',(#13506,#13507,#13508,#13509));
#5343=EDGE_LOOP('',(#13510,#13511,#13512));
#5344=EDGE_LOOP('',(#13513,#13514,#13515,#13516));
#5345=EDGE_LOOP('',(#13517,#13518,#13519,#13520));
#5346=EDGE_LOOP('',(#13521,#13522,#13523));
#5347=EDGE_LOOP('',(#13524,#13525,#13526,#13527));
#5348=EDGE_LOOP('',(#13528,#13529,#13530,#13531));
#5349=EDGE_LOOP('',(#13532,#13533,#13534));
#5350=EDGE_LOOP('',(#13535,#13536,#13537,#13538));
#5351=EDGE_LOOP('',(#13539,#13540,#13541,#13542));
#5352=EDGE_LOOP('',(#13543,#13544,#13545));
#5353=EDGE_LOOP('',(#13546,#13547,#13548,#13549));
#5354=EDGE_LOOP('',(#13550,#13551,#13552,#13553));
#5355=EDGE_LOOP('',(#13554,#13555,#13556,#13557));
#5356=EDGE_LOOP('',(#13558,#13559,#13560));
#5357=EDGE_LOOP('',(#13561,#13562,#13563,#13564));
#5358=EDGE_LOOP('',(#13565,#13566,#13567,#13568));
#5359=EDGE_LOOP('',(#13569,#13570,#13571));
#5360=EDGE_LOOP('',(#13572,#13573,#13574,#13575));
#5361=EDGE_LOOP('',(#13576,#13577,#13578));
#5362=EDGE_LOOP('',(#13579,#13580,#13581,#13582));
#5363=EDGE_LOOP('',(#13583,#13584,#13585,#13586));
#5364=EDGE_LOOP('',(#13587,#13588,#13589,#13590));
#5365=EDGE_LOOP('',(#13591,#13592,#13593,#13594));
#5366=EDGE_LOOP('',(#13595,#13596,#13597,#13598));
#5367=EDGE_LOOP('',(#13599,#13600,#13601,#13602,#13603,#13604,#13605,#13606,
#13607));
#5368=EDGE_LOOP('',(#13608,#13609,#13610,#13611));
#5369=EDGE_LOOP('',(#13612,#13613,#13614,#13615,#13616,#13617,#13618,#13619));
#5370=EDGE_LOOP('',(#13620));
#5371=EDGE_LOOP('',(#13621,#13622,#13623,#13624,#13625));
#5372=EDGE_LOOP('',(#13626,#13627,#13628));
#5373=EDGE_LOOP('',(#13629,#13630,#13631,#13632));
#5374=EDGE_LOOP('',(#13633));
#5375=EDGE_LOOP('',(#13634,#13635,#13636,#13637,#13638,#13639));
#5376=EDGE_LOOP('',(#13640,#13641,#13642));
#5377=EDGE_LOOP('',(#13643,#13644,#13645,#13646,#13647,#13648,#13649));
#5378=EDGE_LOOP('',(#13650));
#5379=EDGE_LOOP('',(#13651,#13652,#13653,#13654));
#5380=EDGE_LOOP('',(#13655,#13656,#13657));
#5381=EDGE_LOOP('',(#13658,#13659,#13660,#13661,#13662));
#5382=EDGE_LOOP('',(#13663,#13664,#13665,#13666,#13667,#13668));
#5383=EDGE_LOOP('',(#13669));
#5384=EDGE_LOOP('',(#13670));
#5385=EDGE_LOOP('',(#13671,#13672,#13673,#13674,#13675,#13676,#13677,#13678));
#5386=EDGE_LOOP('',(#13679));
#5387=EDGE_LOOP('',(#13680));
#5388=EDGE_LOOP('',(#13681,#13682,#13683,#13684));
#5389=EDGE_LOOP('',(#13685,#13686,#13687,#13688));
#5390=EDGE_LOOP('',(#13689,#13690,#13691,#13692));
#5391=EDGE_LOOP('',(#13693,#13694,#13695));
#5392=EDGE_LOOP('',(#13696,#13697,#13698,#13699));
#5393=EDGE_LOOP('',(#13700,#13701,#13702,#13703));
#5394=EDGE_LOOP('',(#13704,#13705,#13706,#13707));
#5395=EDGE_LOOP('',(#13708,#13709,#13710,#13711));
#5396=EDGE_LOOP('',(#13712,#13713,#13714,#13715,#13716,#13717));
#5397=EDGE_LOOP('',(#13718,#13719,#13720));
#5398=EDGE_LOOP('',(#13721,#13722,#13723));
#5399=EDGE_LOOP('',(#13724,#13725,#13726,#13727));
#5400=EDGE_LOOP('',(#13728,#13729,#13730));
#5401=EDGE_LOOP('',(#13731,#13732,#13733,#13734,#13735,#13736,#13737,#13738,
#13739));
#5402=EDGE_LOOP('',(#13740,#13741,#13742,#13743));
#5403=EDGE_LOOP('',(#13744,#13745,#13746,#13747,#13748,#13749,#13750));
#5404=EDGE_LOOP('',(#13751,#13752,#13753,#13754,#13755,#13756,#13757,#13758,
#13759,#13760));
#5405=EDGE_LOOP('',(#13761,#13762,#13763,#13764));
#5406=EDGE_LOOP('',(#13765,#13766,#13767,#13768,#13769,#13770));
#5407=EDGE_LOOP('',(#13771,#13772,#13773,#13774));
#5408=EDGE_LOOP('',(#13775,#13776,#13777,#13778));
#5409=EDGE_LOOP('',(#13779,#13780,#13781,#13782));
#5410=EDGE_LOOP('',(#13783,#13784,#13785,#13786,#13787,#13788,#13789,#13790,
#13791,#13792,#13793,#13794,#13795,#13796,#13797,#13798));
#5411=EDGE_LOOP('',(#13799,#13800,#13801,#13802,#13803,#13804,#13805,#13806,
#13807,#13808,#13809,#13810,#13811,#13812));
#5412=EDGE_LOOP('',(#13813));
#5413=EDGE_LOOP('',(#13814));
#5414=EDGE_LOOP('',(#13815,#13816,#13817,#13818));
#5415=EDGE_LOOP('',(#13819,#13820,#13821,#13822));
#5416=EDGE_LOOP('',(#13823,#13824,#13825,#13826,#13827,#13828,#13829,#13830));
#5417=EDGE_LOOP('',(#13831,#13832,#13833,#13834));
#5418=EDGE_LOOP('',(#13835,#13836,#13837,#13838));
#5419=EDGE_LOOP('',(#13839,#13840,#13841,#13842,#13843,#13844,#13845));
#5420=EDGE_LOOP('',(#13846,#13847,#13848,#13849));
#5421=EDGE_LOOP('',(#13850,#13851,#13852,#13853));
#5422=EDGE_LOOP('',(#13854,#13855,#13856,#13857));
#5423=EDGE_LOOP('',(#13858,#13859,#13860,#13861,#13862,#13863,#13864,#13865,
#13866,#13867));
#5424=EDGE_LOOP('',(#13868,#13869,#13870,#13871,#13872,#13873,#13874,#13875));
#5425=EDGE_LOOP('',(#13876,#13877,#13878,#13879,#13880,#13881,#13882,#13883));
#5426=EDGE_LOOP('',(#13884,#13885,#13886,#13887,#13888,#13889,#13890,#13891));
#5427=EDGE_LOOP('',(#13892,#13893,#13894));
#5428=EDGE_LOOP('',(#13895,#13896,#13897,#13898));
#5429=EDGE_LOOP('',(#13899,#13900,#13901,#13902,#13903));
#5430=EDGE_LOOP('',(#13904,#13905,#13906,#13907));
#5431=EDGE_LOOP('',(#13908,#13909,#13910,#13911,#13912));
#5432=EDGE_LOOP('',(#13913,#13914,#13915,#13916,#13917));
#5433=EDGE_LOOP('',(#13918,#13919,#13920,#13921));
#5434=EDGE_LOOP('',(#13922,#13923,#13924,#13925));
#5435=EDGE_LOOP('',(#13926,#13927,#13928,#13929));
#5436=EDGE_LOOP('',(#13930,#13931,#13932,#13933));
#5437=EDGE_LOOP('',(#13934,#13935,#13936,#13937));
#5438=EDGE_LOOP('',(#13938,#13939,#13940,#13941));
#5439=EDGE_LOOP('',(#13942,#13943,#13944,#13945,#13946,#13947));
#5440=EDGE_LOOP('',(#13948,#13949,#13950,#13951));
#5441=EDGE_LOOP('',(#13952,#13953,#13954,#13955));
#5442=EDGE_LOOP('',(#13956,#13957,#13958,#13959));
#5443=EDGE_LOOP('',(#13960,#13961,#13962,#13963));
#5444=EDGE_LOOP('',(#13964,#13965,#13966,#13967));
#5445=EDGE_LOOP('',(#13968,#13969,#13970,#13971,#13972,#13973,#13974,#13975,
#13976,#13977));
#5446=EDGE_LOOP('',(#13978,#13979,#13980,#13981,#13982,#13983));
#5447=EDGE_LOOP('',(#13984));
#5448=EDGE_LOOP('',(#13985));
#5449=EDGE_LOOP('',(#13986,#13987,#13988,#13989,#13990));
#5450=EDGE_LOOP('',(#13991,#13992,#13993,#13994,#13995));
#5451=EDGE_LOOP('',(#13996,#13997,#13998,#13999));
#5452=EDGE_LOOP('',(#14000,#14001,#14002,#14003,#14004,#14005,#14006));
#5453=EDGE_LOOP('',(#14007,#14008,#14009,#14010));
#5454=EDGE_LOOP('',(#14011,#14012,#14013,#14014));
#5455=EDGE_LOOP('',(#14015,#14016,#14017,#14018,#14019));
#5456=EDGE_LOOP('',(#14020,#14021));
#5457=EDGE_LOOP('',(#14022,#14023,#14024,#14025,#14026,#14027,#14028,#14029));
#5458=EDGE_LOOP('',(#14030,#14031,#14032,#14033,#14034,#14035,#14036,#14037,
#14038,#14039,#14040,#14041,#14042,#14043,#14044));
#5459=EDGE_LOOP('',(#14045,#14046));
#5460=EDGE_LOOP('',(#14047,#14048,#14049,#14050,#14051,#14052,#14053,#14054,
#14055));
#5461=EDGE_LOOP('',(#14056));
#5462=EDGE_LOOP('',(#14057,#14058,#14059,#14060));
#5463=EDGE_LOOP('',(#14061,#14062,#14063,#14064));
#5464=EDGE_LOOP('',(#14065));
#5465=EDGE_LOOP('',(#14066));
#5466=EDGE_LOOP('',(#14067));
#5467=EDGE_LOOP('',(#14068));
#5468=EDGE_LOOP('',(#14069,#14070,#14071,#14072));
#5469=EDGE_LOOP('',(#14073,#14074,#14075,#14076));
#5470=EDGE_LOOP('',(#14077,#14078,#14079,#14080));
#5471=EDGE_LOOP('',(#14081,#14082,#14083,#14084));
#5472=EDGE_LOOP('',(#14085,#14086,#14087,#14088));
#5473=EDGE_LOOP('',(#14089,#14090,#14091,#14092));
#5474=EDGE_LOOP('',(#14093,#14094,#14095,#14096));
#5475=EDGE_LOOP('',(#14097,#14098,#14099,#14100));
#5476=EDGE_LOOP('',(#14101,#14102,#14103,#14104,#14105,#14106,#14107,#14108));
#5477=EDGE_LOOP('',(#14109,#14110,#14111,#14112,#14113,#14114,#14115,#14116));
#5478=EDGE_LOOP('',(#14117,#14118,#14119,#14120,#14121,#14122,#14123,#14124));
#5479=EDGE_LOOP('',(#14125,#14126));
#5480=EDGE_LOOP('',(#14127,#14128,#14129,#14130,#14131));
#5481=EDGE_LOOP('',(#14132,#14133,#14134,#14135,#14136));
#5482=EDGE_LOOP('',(#14137,#14138,#14139,#14140,#14141));
#5483=EDGE_LOOP('',(#14142,#14143,#14144,#14145,#14146,#14147));
#5484=EDGE_LOOP('',(#14148,#14149,#14150,#14151));
#5485=EDGE_LOOP('',(#14152,#14153,#14154,#14155,#14156));
#5486=EDGE_LOOP('',(#14157,#14158,#14159,#14160));
#5487=EDGE_LOOP('',(#14161));
#5488=EDGE_LOOP('',(#14162,#14163));
#5489=EDGE_LOOP('',(#14164,#14165));
#5490=EDGE_LOOP('',(#14166,#14167));
#5491=EDGE_LOOP('',(#14168,#14169,#14170));
#5492=EDGE_LOOP('',(#14171,#14172));
#5493=EDGE_LOOP('',(#14173,#14174));
#5494=EDGE_LOOP('',(#14175,#14176,#14177));
#5495=EDGE_LOOP('',(#14178,#14179,#14180));
#5496=EDGE_LOOP('',(#14181));
#5497=EDGE_LOOP('',(#14182));
#5498=EDGE_LOOP('',(#14183,#14184,#14185,#14186,#14187,#14188,#14189));
#5499=EDGE_LOOP('',(#14190,#14191,#14192,#14193,#14194,#14195,#14196));
#5500=EDGE_LOOP('',(#14197,#14198,#14199,#14200,#14201,#14202,#14203));
#5501=EDGE_LOOP('',(#14204,#14205,#14206,#14207,#14208,#14209,#14210));
#5502=EDGE_LOOP('',(#14211,#14212,#14213,#14214,#14215,#14216,#14217));
#5503=EDGE_LOOP('',(#14218,#14219,#14220,#14221,#14222,#14223,#14224));
#5504=EDGE_LOOP('',(#14225,#14226,#14227));
#5505=EDGE_LOOP('',(#14228,#14229,#14230));
#5506=EDGE_LOOP('',(#14231));
#5507=EDGE_LOOP('',(#14232,#14233,#14234,#14235,#14236,#14237,#14238,#14239,
#14240,#14241,#14242,#14243,#14244,#14245,#14246,#14247,#14248,#14249));
#5508=EDGE_LOOP('',(#14250,#14251,#14252));
#5509=CIRCLE('',#15340,6.25);
#5510=CIRCLE('',#15341,1.);
#5511=CIRCLE('',#15342,6.25);
#5512=CIRCLE('',#15344,6.25);
#5513=CIRCLE('',#15346,6.25);
#5514=CIRCLE('',#15348,2.25);
#5515=CIRCLE('',#15349,2.25);
#5516=CIRCLE('',#15351,3.);
#5517=CIRCLE('',#15352,3.);
#5518=CIRCLE('',#15354,7.5);
#5519=CIRCLE('',#15355,5.25);
#5520=CIRCLE('',#15356,5.25);
#5521=CIRCLE('',#15358,10.0000000011845);
#5522=CIRCLE('',#15359,10.0000000011845);
#5523=CIRCLE('',#15362,10.4947894497429);
#5524=CIRCLE('',#15363,5.25);
#5525=CIRCLE('',#15364,10.4947894499283);
#5526=CIRCLE('',#15367,4.);
#5527=CIRCLE('',#15368,4.);
#5528=CIRCLE('',#15370,5.25);
#5529=CIRCLE('',#15374,5.04017795657138);
#5530=CIRCLE('',#15375,5.04017795657138);
#5531=CIRCLE('',#15377,4.);
#5532=CIRCLE('',#15379,0.300000000000003);
#5533=CIRCLE('',#15380,0.300000000000003);
#5534=CIRCLE('',#15382,0.300000000000003);
#5535=CIRCLE('',#15383,0.300000000000003);
#5536=CIRCLE('',#15385,4.);
#5537=CIRCLE('',#15386,4.);
#5538=CIRCLE('',#15388,4.5);
#5539=CIRCLE('',#15389,0.75);
#5540=CIRCLE('',#15390,4.5);
#5541=CIRCLE('',#15392,4.19999999999999);
#5542=CIRCLE('',#15393,4.2);
#5543=CIRCLE('',#15395,4.5);
#5544=CIRCLE('',#15397,5.8);
#5545=CIRCLE('',#15398,5.8);
#5546=CIRCLE('',#15442,5.);
#5547=CIRCLE('',#15443,5.);
#5548=CIRCLE('',#15444,0.249999999999999);
#5549=CIRCLE('',#15446,5.);
#5550=CIRCLE('',#15447,5.);
#5551=CIRCLE('',#15450,10.0000000011845);
#5552=CIRCLE('',#15451,10.0000000011845);
#5553=CIRCLE('',#15473,4.);
#5554=CIRCLE('',#15474,4.);
#5555=CIRCLE('',#15476,7.66224510179708);
#5556=CIRCLE('',#15477,7.97930918062551);
#5557=CIRCLE('',#15478,7.98595584236444);
#5558=CIRCLE('',#15479,7.98595584236446);
#5559=CIRCLE('',#15480,7.97930918062549);
#5560=CIRCLE('',#15481,7.66224510179716);
#5561=CIRCLE('',#15482,7.97930918062553);
#5562=CIRCLE('',#15483,7.98595584236444);
#5563=CIRCLE('',#15484,7.98595584236446);
#5564=CIRCLE('',#15485,7.97930918062551);
#5565=CIRCLE('',#15486,7.66224510179724);
#5566=CIRCLE('',#15487,7.97930918062551);
#5567=CIRCLE('',#15488,7.98595584236446);
#5568=CIRCLE('',#15489,7.98595584236444);
#5569=CIRCLE('',#15490,7.97930918062553);
#5570=CIRCLE('',#15491,7.66224510179716);
#5571=CIRCLE('',#15492,7.97930918062549);
#5572=CIRCLE('',#15493,7.98595584236446);
#5573=CIRCLE('',#15494,7.98595584236444);
#5574=CIRCLE('',#15495,7.97930918062551);
#5575=CIRCLE('',#15497,2.2);
#5576=CIRCLE('',#15498,0.40000000000004);
#5577=CIRCLE('',#15499,1.8001015361136);
#5578=CIRCLE('',#15501,1.78525);
#5579=CIRCLE('',#15502,1.78525);
#5580=CIRCLE('',#15504,2.);
#5581=CIRCLE('',#15505,2.);
#5582=CIRCLE('',#15507,2.);
#5583=CIRCLE('',#15539,3.);
#5584=CIRCLE('',#15540,3.);
#5585=CIRCLE('',#15541,3.);
#5586=CIRCLE('',#15542,3.);
#5587=CIRCLE('',#15543,3.);
#5588=CIRCLE('',#15544,3.);
#5589=CIRCLE('',#15546,5.7963350489771);
#5590=CIRCLE('',#15547,5.98747390390977);
#5591=CIRCLE('',#15548,5.99149706962117);
#5592=CIRCLE('',#15549,5.99149706962117);
#5593=CIRCLE('',#15550,5.98747390390977);
#5594=CIRCLE('',#15551,5.79633504897711);
#5595=CIRCLE('',#15552,5.98747390390978);
#5596=CIRCLE('',#15553,5.99149706962117);
#5597=CIRCLE('',#15554,5.99149706962117);
#5598=CIRCLE('',#15555,5.98747390390977);
#5599=CIRCLE('',#15556,5.79633504897713);
#5600=CIRCLE('',#15557,5.98747390390977);
#5601=CIRCLE('',#15558,5.99149706962117);
#5602=CIRCLE('',#15559,5.99149706962117);
#5603=CIRCLE('',#15560,5.98747390390978);
#5604=CIRCLE('',#15561,5.79633504897711);
#5605=CIRCLE('',#15562,5.98747390390977);
#5606=CIRCLE('',#15563,5.99149706962117);
#5607=CIRCLE('',#15564,5.99149706962117);
#5608=CIRCLE('',#15565,5.98747390390977);
#5609=CIRCLE('',#15567,4.);
#5610=CIRCLE('',#15568,4.);
#5611=CIRCLE('',#15569,4.);
#5612=CIRCLE('',#15570,4.);
#5613=CIRCLE('',#15571,4.);
#5614=CIRCLE('',#15572,4.);
#5615=CIRCLE('',#15573,4.);
#5616=CIRCLE('',#15574,4.);
#5617=CIRCLE('',#15575,4.);
#5618=CIRCLE('',#15576,4.);
#5619=CIRCLE('',#15577,4.);
#5620=CIRCLE('',#15578,4.);
#5621=CIRCLE('',#15580,3.);
#5622=CIRCLE('',#15581,5.7963350489771);
#5623=CIRCLE('',#15582,5.98747390390977);
#5624=CIRCLE('',#15583,5.99149706962117);
#5625=CIRCLE('',#15584,5.99149706962117);
#5626=CIRCLE('',#15585,5.98747390390977);
#5627=CIRCLE('',#15586,5.79633504897711);
#5628=CIRCLE('',#15587,5.98747390390978);
#5629=CIRCLE('',#15588,5.99149706962117);
#5630=CIRCLE('',#15589,5.99149706962117);
#5631=CIRCLE('',#15590,5.98747390390977);
#5632=CIRCLE('',#15591,5.79633504897713);
#5633=CIRCLE('',#15592,5.98747390390977);
#5634=CIRCLE('',#15593,5.99149706962117);
#5635=CIRCLE('',#15594,5.99149706962117);
#5636=CIRCLE('',#15595,5.98747390390978);
#5637=CIRCLE('',#15596,5.79633504897711);
#5638=CIRCLE('',#15597,5.98747390390977);
#5639=CIRCLE('',#15598,5.99149706962117);
#5640=CIRCLE('',#15599,5.99149706962117);
#5641=CIRCLE('',#15600,5.98747390390977);
#5642=CIRCLE('',#15602,3.);
#5643=CIRCLE('',#15603,3.);
#5644=CIRCLE('',#15604,3.);
#5645=CIRCLE('',#15605,3.);
#5646=CIRCLE('',#15606,3.);
#5647=CIRCLE('',#15681,9.6875);
#5648=CIRCLE('',#15682,9.6875);
#5649=CIRCLE('',#15683,9.6875);
#5650=CIRCLE('',#15684,9.6875);
#5651=CIRCLE('',#15686,2.067);
#5652=CIRCLE('',#15687,2.067);
#5653=CIRCLE('',#15689,5.);
#5654=CIRCLE('',#15690,5.);
#5655=CIRCLE('',#15692,9.);
#5656=CIRCLE('',#15693,9.);
#5657=CIRCLE('',#15695,9.);
#5658=CIRCLE('',#15696,9.);
#5659=CIRCLE('',#15697,9.);
#5660=CIRCLE('',#15711,2.);
#5661=CIRCLE('',#15712,2.);
#5662=CIRCLE('',#15728,2.8);
#5663=CIRCLE('',#15729,2.5);
#5664=CIRCLE('',#15733,2.8);
#5665=CIRCLE('',#15734,2.5);
#5666=CIRCLE('',#15736,2.5);
#5667=CIRCLE('',#15737,2.8);
#5668=CIRCLE('',#15742,2.8);
#5669=CIRCLE('',#15743,2.5);
#5670=CIRCLE('',#15751,8.99999999999999);
#5671=CIRCLE('',#15752,8.99999999999999);
#5672=CIRCLE('',#15755,9.);
#5673=CIRCLE('',#15756,9.);
#5674=CIRCLE('',#15758,8.99999999999999);
#5675=CIRCLE('',#15759,8.99999999999999);
#5676=CIRCLE('',#15762,0.500000000000001);
#5677=CIRCLE('',#15763,0.500000000000001);
#5678=CIRCLE('',#15765,0.500000000000001);
#5679=CIRCLE('',#15766,0.500000000000001);
#5680=CIRCLE('',#15769,0.500000000000001);
#5681=CIRCLE('',#15770,0.500000000000001);
#5682=CIRCLE('',#15772,0.500000000000001);
#5683=CIRCLE('',#15773,0.500000000000001);
#5684=CIRCLE('',#15779,3.5);
#5685=CIRCLE('',#15800,3.5);
#5686=CIRCLE('',#15801,3.5);
#5687=CIRCLE('',#15803,3.5);
#5688=CIRCLE('',#15810,2.);
#5689=CIRCLE('',#15811,0.799999999999998);
#5690=CIRCLE('',#15813,2.);
#5691=CIRCLE('',#15818,0.799999999999998);
#5692=CIRCLE('',#15834,2.5);
#5693=CIRCLE('',#15837,2.5);
#5694=CIRCLE('',#15840,2.5);
#5695=CIRCLE('',#15842,2.5);
#5696=CIRCLE('',#15860,0.800000000000002);
#5697=CIRCLE('',#15861,0.800000000000002);
#5698=CIRCLE('',#15862,8.2);
#5699=CIRCLE('',#15863,0.800000000000002);
#5700=CIRCLE('',#15864,0.800000000000002);
#5701=CIRCLE('',#15865,0.800000000000002);
#5702=CIRCLE('',#15866,0.800000000000002);
#5703=CIRCLE('',#15868,0.799999999999999);
#5704=CIRCLE('',#15869,0.799999999999999);
#5705=CIRCLE('',#15870,0.799999999999999);
#5706=CIRCLE('',#15871,0.799999999999999);
#5707=CIRCLE('',#15872,8.2);
#5708=CIRCLE('',#15873,0.799999999999999);
#5709=CIRCLE('',#15874,0.799999999999999);
#5710=CIRCLE('',#15876,2.7);
#5711=CIRCLE('',#15877,0.800000000000002);
#5712=CIRCLE('',#15879,0.799999999999999);
#5713=CIRCLE('',#15880,3.2);
#5714=CIRCLE('',#15882,0.800000000000002);
#5715=CIRCLE('',#15883,1.2);
#5716=CIRCLE('',#15885,14.2);
#5717=CIRCLE('',#15886,0.799999999999999);
#5718=CIRCLE('',#15888,4.);
#5719=CIRCLE('',#15889,4.);
#5720=CIRCLE('',#15891,4.);
#5721=CIRCLE('',#15892,4.);
#5722=CIRCLE('',#15893,3.7);
#5723=CIRCLE('',#15895,4.);
#5724=CIRCLE('',#15896,4.);
#5725=CIRCLE('',#15898,2.8);
#5726=CIRCLE('',#15899,2.8);
#5727=CIRCLE('',#15900,2.8);
#5728=CIRCLE('',#15901,2.8);
#5729=CIRCLE('',#15902,2.8);
#5730=CIRCLE('',#15903,2.8);
#5731=CIRCLE('',#15904,2.8);
#5732=CIRCLE('',#15906,2.5);
#5733=CIRCLE('',#15907,2.5);
#5734=CIRCLE('',#15908,2.5);
#5735=CIRCLE('',#15909,2.5);
#5736=CIRCLE('',#15910,2.5);
#5737=CIRCLE('',#15912,4.5);
#5738=CIRCLE('',#15913,0.5);
#5739=CIRCLE('',#15915,10.5);
#5740=CIRCLE('',#15916,10.);
#5741=CIRCLE('',#15918,6.5);
#5742=CIRCLE('',#15919,6.);
#5743=CIRCLE('',#15921,17.);
#5744=CIRCLE('',#15922,17.);
#5745=CIRCLE('',#15924,17.);
#5746=CIRCLE('',#15925,17.);
#5747=CIRCLE('',#15927,17.);
#5748=CIRCLE('',#15928,17.);
#5749=CIRCLE('',#15929,17.);
#5750=CIRCLE('',#15931,3.8);
#5751=CIRCLE('',#15932,3.3);
#5752=CIRCLE('',#15933,3.3);
#5753=CIRCLE('',#15935,4.);
#5754=CIRCLE('',#15936,0.5);
#5755=CIRCLE('',#15937,4.5);
#5756=CIRCLE('',#15938,0.5);
#5757=CIRCLE('',#15940,1.);
#5758=CIRCLE('',#15941,1.5);
#5759=CIRCLE('',#15943,1.5);
#5760=CIRCLE('',#15944,1.5);
#5761=CIRCLE('',#15946,3.8);
#5762=CIRCLE('',#15947,3.8);
#5763=CIRCLE('',#15948,3.8);
#5764=CIRCLE('',#15949,3.8);
#5765=CIRCLE('',#15951,0.499999999999999);
#5766=CIRCLE('',#15952,0.499999999999999);
#5767=CIRCLE('',#15954,1.);
#5768=CIRCLE('',#15955,1.);
#5769=CIRCLE('',#15957,16.5);
#5770=CIRCLE('',#15958,0.499999999999999);
#5771=CIRCLE('',#15960,3.);
#5772=CIRCLE('',#15962,2.5);
#5773=CIRCLE('',#15963,2.5);
#5774=CIRCLE('',#15964,2.5);
#5775=CIRCLE('',#15965,2.5);
#5776=CIRCLE('',#15966,2.5);
#5777=CIRCLE('',#15967,2.5);
#5778=CIRCLE('',#15972,3.);
#5779=CIRCLE('',#15973,0.499999999999997);
#5780=CIRCLE('',#15975,5.5);
#5781=CIRCLE('',#15976,6.);
#5782=CIRCLE('',#15978,10.5);
#5783=CIRCLE('',#15979,11.);
#5784=CIRCLE('',#15980,0.499999999999988);
#5785=CIRCLE('',#15981,0.499999999999996);
#5786=CIRCLE('',#15982,0.499999999999997);
#5787=CIRCLE('',#15983,0.49999999999999);
#5788=CIRCLE('',#15999,11.);
#5789=CIRCLE('',#16000,10.5);
#5790=CIRCLE('',#16006,6.);
#5791=CIRCLE('',#16007,6.5);
#5792=CIRCLE('',#16009,0.5);
#5793=CIRCLE('',#16010,1.5);
#5794=CIRCLE('',#16011,0.500000000000001);
#5795=CIRCLE('',#16012,1.);
#5796=CIRCLE('',#16015,18.);
#5797=CIRCLE('',#16017,0.5);
#5798=CIRCLE('',#16020,0.5);
#5799=CIRCLE('',#16026,3.);
#5800=CIRCLE('',#16028,1.);
#5801=CIRCLE('',#16029,1.);
#5802=CIRCLE('',#16034,0.500000000000002);
#5803=CIRCLE('',#16035,3.);
#5804=CIRCLE('',#16037,0.5);
#5805=CIRCLE('',#16042,0.5);
#5806=CIRCLE('',#16047,1.5);
#5807=CIRCLE('',#16049,16.5);
#5808=CIRCLE('',#16050,0.499999999999999);
#5809=CIRCLE('',#16052,16.5);
#5810=CIRCLE('',#16053,0.500000000000001);
#5811=CIRCLE('',#16055,3.);
#5812=CIRCLE('',#16056,0.499999999999999);
#5813=CIRCLE('',#16060,14.5);
#5814=CIRCLE('',#16061,13.5);
#5815=CIRCLE('',#16063,10.5);
#5816=CIRCLE('',#16064,10.5);
#5817=CIRCLE('',#16067,10.);
#5818=CIRCLE('',#16068,0.500000000000001);
#5819=CIRCLE('',#16070,1.);
#5820=CIRCLE('',#16071,1.);
#5821=CIRCLE('',#16073,1.);
#5822=CIRCLE('',#16074,1.);
#5823=CIRCLE('',#16076,1.);
#5824=CIRCLE('',#16087,1.5);
#5825=CIRCLE('',#16088,0.5);
#5826=CIRCLE('',#16090,0.5);
#5827=CIRCLE('',#16091,4.3);
#5828=CIRCLE('',#16094,3.8);
#5829=CIRCLE('',#16095,3.8);
#5830=CIRCLE('',#16097,1.5);
#5831=CIRCLE('',#16098,1.5);
#5832=CIRCLE('',#16100,1.);
#5833=CIRCLE('',#16103,5.5);
#5834=CIRCLE('',#16104,6.);
#5835=CIRCLE('',#16105,11.);
#5836=CIRCLE('',#16106,5.5);
#5837=CIRCLE('',#16108,1.);
#5838=CIRCLE('',#16109,4.5);
#5839=CIRCLE('',#16112,10.5);
#5840=CIRCLE('',#16114,10.5);
#5841=CIRCLE('',#16115,10.5);
#5842=CIRCLE('',#16117,14.5);
#5843=CIRCLE('',#16118,6.5);
#5844=CIRCLE('',#16120,6.5);
#5845=CIRCLE('',#16121,10.);
#5846=CIRCLE('',#16123,10.);
#5847=CIRCLE('',#16126,6.);
#5848=CIRCLE('',#16127,6.);
#5849=CIRCLE('',#16130,6.);
#5850=CIRCLE('',#16131,6.);
#5851=CIRCLE('',#16148,1.50083490556055);
#5852=CIRCLE('',#16151,0.5);
#5853=CIRCLE('',#16166,13.5);
#5854=CIRCLE('',#16178,3.);
#5855=CIRCLE('',#16179,5.56214886532177);
#5856=CIRCLE('',#16180,5.9897829676876);
#5857=CIRCLE('',#16181,5.9897829676876);
#5858=CIRCLE('',#16182,5.5621488653218);
#5859=CIRCLE('',#16183,5.98978296768761);
#5860=CIRCLE('',#16184,5.9897829676876);
#5861=CIRCLE('',#16185,5.56214886532182);
#5862=CIRCLE('',#16186,5.9897829676876);
#5863=CIRCLE('',#16187,5.98978296768761);
#5864=CIRCLE('',#16188,5.5621488653218);
#5865=CIRCLE('',#16189,5.9897829676876);
#5866=CIRCLE('',#16190,5.9897829676876);
#5867=CIRCLE('',#16192,1.5);
#5868=CIRCLE('',#16193,1.1935);
#5869=CIRCLE('',#16194,1.5);
#5870=CIRCLE('',#16196,3.);
#5871=CIRCLE('',#16198,1.5);
#5872=CIRCLE('',#16216,4.5);
#5873=CIRCLE('',#16217,4.5);
#5874=CIRCLE('',#16218,4.5);
#5875=CIRCLE('',#16219,4.5);
#5876=CIRCLE('',#16220,4.5);
#5877=CIRCLE('',#16222,4.5);
#5878=CIRCLE('',#16223,4.5);
#5879=CIRCLE('',#16224,4.5);
#5880=CIRCLE('',#16225,4.5);
#5881=CIRCLE('',#16227,4.5);
#5882=CIRCLE('',#16228,4.5);
#5883=CIRCLE('',#16229,4.5);
#5884=CIRCLE('',#16230,4.5);
#5885=CIRCLE('',#16231,4.5);
#5886=CIRCLE('',#16232,4.5);
#5887=CIRCLE('',#16233,4.5);
#5888=CIRCLE('',#16234,4.5);
#5889=CIRCLE('',#16236,4.5);
#5890=CIRCLE('',#16237,4.5);
#5891=CIRCLE('',#16238,4.5);
#5892=CIRCLE('',#16239,4.5);
#5893=CIRCLE('',#16240,4.5);
#5894=CIRCLE('',#16242,5.5);
#5895=CIRCLE('',#16243,5.5);
#5896=CIRCLE('',#16244,5.5);
#5897=CIRCLE('',#16245,5.5);
#5898=CIRCLE('',#16247,5.5);
#5899=CIRCLE('',#16248,5.5);
#5900=CIRCLE('',#16249,5.5);
#5901=CIRCLE('',#16250,5.5);
#5902=CIRCLE('',#16252,2.);
#5903=CIRCLE('',#16253,2.);
#5904=CIRCLE('',#16255,2.5);
#5905=CIRCLE('',#16256,2.5);
#5906=CIRCLE('',#16258,1.75);
#5907=CIRCLE('',#16259,1.75);
#5908=CIRCLE('',#16261,1.);
#5909=CIRCLE('',#16262,1.);
#5910=CIRCLE('',#16264,0.999999999999999);
#5911=CIRCLE('',#16265,1.);
#5912=CIRCLE('',#16267,1.);
#5913=CIRCLE('',#16268,0.999999999999999);
#5914=CIRCLE('',#16270,5.5);
#5915=CIRCLE('',#16271,5.50000000000001);
#5916=CIRCLE('',#16272,5.50000000000001);
#5917=CIRCLE('',#16273,5.5);
#5918=CIRCLE('',#16275,0.999999999999999);
#5919=CIRCLE('',#16276,1.);
#5920=CIRCLE('',#16278,1.);
#5921=CIRCLE('',#16279,0.999999999999999);
#5922=CIRCLE('',#16281,5.5);
#5923=CIRCLE('',#16282,5.50000000000001);
#5924=CIRCLE('',#16283,5.50000000000001);
#5925=CIRCLE('',#16284,5.5);
#5926=CIRCLE('',#16286,1.);
#5927=CIRCLE('',#16287,1.);
#5928=CIRCLE('',#16289,3.5);
#5929=CIRCLE('',#16290,3.5);
#5930=CIRCLE('',#16292,4.5);
#5931=CIRCLE('',#16293,4.5);
#5932=CIRCLE('',#16294,4.5);
#5933=CIRCLE('',#16295,4.5);
#5934=CIRCLE('',#16300,0.5);
#5935=CIRCLE('',#16301,0.5);
#5936=CIRCLE('',#16304,0.5);
#5937=CIRCLE('',#16308,0.5);
#5938=CIRCLE('',#16318,0.5);
#5939=CIRCLE('',#16319,0.5);
#5940=CIRCLE('',#16322,0.5);
#5941=CIRCLE('',#16326,0.5);
#5942=CIRCLE('',#16331,0.5);
#5943=CIRCLE('',#16332,0.5);
#5944=CIRCLE('',#16335,0.5);
#5945=CIRCLE('',#16339,0.5);
#5946=CIRCLE('',#16347,0.5);
#5947=CIRCLE('',#16348,0.5);
#5948=CIRCLE('',#16351,0.5);
#5949=CIRCLE('',#16354,0.5);
#5950=CIRCLE('',#16369,0.500000000000002);
#5951=CIRCLE('',#16370,0.5);
#5952=CIRCLE('',#16373,0.500000000000002);
#5953=CIRCLE('',#16374,0.5);
#5954=CIRCLE('',#16377,0.500000000000002);
#5955=CIRCLE('',#16378,0.500000000000002);
#5956=CIRCLE('',#16380,0.5);
#5957=CIRCLE('',#16382,0.5);
#5958=CIRCLE('',#16390,14.5);
#5959=CIRCLE('',#16391,9.5);
#5960=CIRCLE('',#16393,5.);
#5961=CIRCLE('',#16394,5.);
#5962=CIRCLE('',#16396,5.5);
#5963=CIRCLE('',#16397,5.5);
#5964=CIRCLE('',#16399,2.5);
#5965=CIRCLE('',#16401,2.4585);
#5966=CIRCLE('',#16402,2.4585);
#5967=CIRCLE('',#16404,6.5);
#5968=CIRCLE('',#16406,1.621);
#5969=CIRCLE('',#16407,1.621);
#5970=CIRCLE('',#16409,2.4585);
#5971=CIRCLE('',#16410,2.4585);
#5972=CIRCLE('',#16412,3.5);
#5973=CIRCLE('',#16413,3.5);
#5974=CIRCLE('',#16415,3.50000000000384);
#5975=CIRCLE('',#16416,3.50000000000384);
#5976=CIRCLE('',#16418,7.);
#5977=CIRCLE('',#16419,7.);
#5978=CIRCLE('',#16421,2.5);
#5979=CIRCLE('',#16422,2.3);
#5980=CIRCLE('',#16424,1.6);
#5981=CIRCLE('',#16425,1.6);
#5982=CIRCLE('',#16427,2.5);
#5983=CIRCLE('',#16429,1.75);
#5984=CIRCLE('',#16430,1.75);
#5985=CIRCLE('',#16441,21.);
#5986=CIRCLE('',#16442,21.);
#5987=CIRCLE('',#16445,5.5);
#5988=CIRCLE('',#16446,5.5);
#5989=CIRCLE('',#16449,21.);
#5990=CIRCLE('',#16450,21.);
#5991=CIRCLE('',#16452,5.00000000000001);
#5992=CIRCLE('',#16453,5.);
#5993=CIRCLE('',#16461,19.);
#5994=CIRCLE('',#16464,19.);
#5995=CIRCLE('',#16465,7.00000000000384);
#5996=CIRCLE('',#16466,19.);
#5997=CIRCLE('',#16468,19.);
#5998=CIRCLE('',#16469,19.);
#5999=CIRCLE('',#16475,7.00000000000384);
#6000=CIRCLE('',#16476,19.);
#6001=CIRCLE('',#16482,19.);
#6002=CIRCLE('',#16486,19.);
#6003=CIRCLE('',#16491,17.0599057548774);
#6004=CIRCLE('',#16492,0.500000000000001);
#6005=CIRCLE('',#16493,0.500000000000001);
#6006=CIRCLE('',#16494,16.5718869058529);
#6007=CIRCLE('',#16496,19.5);
#6008=CIRCLE('',#16497,19.5);
#6009=CIRCLE('',#16499,2.50461426675156);
#6010=CIRCLE('',#16500,2.60305176675156);
#6011=CIRCLE('',#16501,2.50461426675156);
#6012=CIRCLE('',#16503,2.20465088114115);
#6013=CIRCLE('',#16505,19.3089875327072);
#6014=CIRCLE('',#16506,16.6910124672929);
#6015=CIRCLE('',#16507,16.6910124672929);
#6016=CIRCLE('',#16508,16.6910124672929);
#6017=CIRCLE('',#16509,16.6910124672929);
#6018=CIRCLE('',#16511,19.5);
#6019=CIRCLE('',#16512,3.);
#6020=CIRCLE('',#16514,16.5);
#6021=CIRCLE('',#16515,16.5);
#6022=CIRCLE('',#16516,16.5);
#6023=CIRCLE('',#16517,16.5);
#6024=CIRCLE('',#16518,16.5);
#6025=CIRCLE('',#16519,5.45169314906474);
#6026=CIRCLE('',#16520,16.5);
#6027=CIRCLE('',#16521,16.5);
#6028=CIRCLE('',#16522,16.5);
#6029=CIRCLE('',#16523,16.5);
#6030=CIRCLE('',#16524,16.5);
#6031=CIRCLE('',#16526,4.5992601276539);
#6032=CIRCLE('',#16528,19.5);
#6033=CIRCLE('',#16529,0.5);
#6034=CIRCLE('',#16531,5.);
#6035=CIRCLE('',#16533,5.5);
#6036=CIRCLE('',#16534,1.);
#6037=CIRCLE('',#16535,4.5);
#6038=CIRCLE('',#16536,1.);
#6039=CIRCLE('',#16538,0.5);
#6040=CIRCLE('',#16539,19.5);
#6041=CIRCLE('',#16540,1.00000000000008);
#6042=CIRCLE('',#16541,6.65199991070048);
#6043=CIRCLE('',#16542,1.00000000000005);
#6044=CIRCLE('',#16544,17.5);
#6045=CIRCLE('',#16545,1.);
#6046=CIRCLE('',#16547,8.);
#6047=CIRCLE('',#16548,6.65097177940297);
#6048=CIRCLE('',#16550,9.);
#6049=CIRCLE('',#16552,1.);
#6050=CIRCLE('',#16553,0.500000000000001);
#6051=CIRCLE('',#16554,0.5);
#6052=CIRCLE('',#16556,14.5);
#6053=CIRCLE('',#16557,14.5);
#6054=CIRCLE('',#16558,0.500000000000013);
#6055=CIRCLE('',#16559,4.31029789941839);
#6056=CIRCLE('',#16560,0.499999999999922);
#6057=CIRCLE('',#16562,6.5);
#6058=CIRCLE('',#16563,0.499999999999999);
#6059=CIRCLE('',#16564,6.);
#6060=CIRCLE('',#16565,0.5);
#6061=CIRCLE('',#16567,2.9);
#6062=CIRCLE('',#16568,2.9);
#6063=CIRCLE('',#16574,6.5);
#6064=CIRCLE('',#16575,6.5);
#6065=CIRCLE('',#16577,5.);
#6066=CIRCLE('',#16580,2.67271103248174);
#6067=CIRCLE('',#16583,2.);
#6068=CIRCLE('',#16585,2.);
#6069=CIRCLE('',#16586,2.);
#6070=CIRCLE('',#16588,2.2295);
#6071=CIRCLE('',#16589,2.2295);
#6072=CIRCLE('',#16591,17.5);
#6073=CIRCLE('',#16592,17.5);
#6074=CIRCLE('',#16594,0.500000000000001);
#6075=CIRCLE('',#16595,0.499999999999998);
#6076=CIRCLE('',#16596,0.500000000000003);
#6077=CIRCLE('',#16598,0.5);
#6078=CIRCLE('',#16599,0.5);
#6079=CIRCLE('',#16601,0.499999999999999);
#6080=CIRCLE('',#16602,0.5);
#6081=CIRCLE('',#16604,0.499999999999998);
#6082=CIRCLE('',#16605,0.5);
#6083=CIRCLE('',#16609,0.499999999999998);
#6084=CIRCLE('',#16610,0.499999999999998);
#6085=CIRCLE('',#16612,3.3235);
#6086=CIRCLE('',#16613,3.3235);
#6087=CIRCLE('',#16615,0.5);
#6088=CIRCLE('',#16617,0.5);
#6089=CIRCLE('',#16619,4.);
#6090=CIRCLE('',#16621,4.);
#6091=CIRCLE('',#16623,5.5);
#6092=CIRCLE('',#16625,2.5);
#6093=CIRCLE('',#16626,2.5);
#6094=CIRCLE('',#16628,0.5);
#6095=CIRCLE('',#16630,2.067);
#6096=CIRCLE('',#16631,2.067);
#6097=CIRCLE('',#16633,5.);
#6098=CIRCLE('',#16634,14.8183541121548);
#6099=CIRCLE('',#16636,17.4363291775691);
#6100=CIRCLE('',#16638,1.);
#6101=CIRCLE('',#16640,2.5);
#6102=CIRCLE('',#16641,2.5);
#6103=CIRCLE('',#16643,2.);
#6104=CIRCLE('',#16644,2.);
#6105=CIRCLE('',#16649,0.5);
#6106=CIRCLE('',#16651,0.5);
#6107=CIRCLE('',#16654,21.);
#6108=CIRCLE('',#16655,21.);
#6109=CIRCLE('',#16657,5.5);
#6110=CIRCLE('',#16658,21.);
#6111=CIRCLE('',#16661,5.5);
#6112=CIRCLE('',#16664,21.);
#6113=CIRCLE('',#16666,0.499999999999999);
#6114=CIRCLE('',#16667,0.5);
#6115=CIRCLE('',#16668,0.5);
#6116=CIRCLE('',#16669,0.5);
#6117=CIRCLE('',#16670,0.500000000000001);
#6118=CIRCLE('',#16672,0.500000000000001);
#6119=CIRCLE('',#16673,17.);
#6120=CIRCLE('',#16677,1.);
#6121=CIRCLE('',#16678,1.);
#6122=CIRCLE('',#16679,20.);
#6123=CIRCLE('',#16681,0.5);
#6124=CIRCLE('',#16682,0.500000000000001);
#6125=CIRCLE('',#16683,0.5);
#6126=CIRCLE('',#16686,0.500000000000002);
#6127=CIRCLE('',#16688,0.5);
#6128=CIRCLE('',#16689,0.5);
#6129=CIRCLE('',#16690,0.5);
#6130=CIRCLE('',#16692,0.5);
#6131=CIRCLE('',#16696,0.5);
#6132=CIRCLE('',#16697,0.5);
#6133=CIRCLE('',#16699,0.5);
#6134=CIRCLE('',#16703,0.5);
#6135=CIRCLE('',#16704,0.5);
#6136=CIRCLE('',#16710,0.499999999999998);
#6137=CIRCLE('',#16711,0.499999999999998);
#6138=CIRCLE('',#16712,0.5);
#6139=CIRCLE('',#16715,0.499999999999996);
#6140=CIRCLE('',#16716,0.499999999999998);
#6141=CIRCLE('',#16718,0.5);
#6142=CIRCLE('',#16719,0.5);
#6143=CIRCLE('',#16722,0.499999999999999);
#6144=CIRCLE('',#16724,0.499999999999998);
#6145=CIRCLE('',#16726,0.5);
#6146=CIRCLE('',#16732,0.5);
#6147=CIRCLE('',#16734,0.500000000000002);
#6148=CIRCLE('',#16735,0.500000000000001);
#6149=CIRCLE('',#16737,0.499999999999999);
#6150=CIRCLE('',#16744,1.);
#6151=CIRCLE('',#16747,1.);
#6152=CIRCLE('',#16750,0.959917621886371);
#6153=CIRCLE('',#16753,5.);
#6154=CIRCLE('',#16760,5.);
#6155=CIRCLE('',#16762,0.499999999999999);
#6156=CIRCLE('',#16763,6.);
#6157=CIRCLE('',#16764,0.499999999999999);
#6158=CIRCLE('',#16770,0.5);
#6159=CIRCLE('',#16772,0.499999999999998);
#6160=CIRCLE('',#16773,0.5);
#6161=CIRCLE('',#16774,0.500000000000001);
#6162=CIRCLE('',#16776,0.5);
#6163=CIRCLE('',#16795,0.499999999999998);
#6164=CIRCLE('',#16799,1.);
#6165=CIRCLE('',#16800,20.);
#6166=CIRCLE('',#16801,4.5);
#6167=CIRCLE('',#16805,2.39349905057784);
#6168=CIRCLE('',#16811,17.5);
#6169=CIRCLE('',#16815,0.5);
#6170=CIRCLE('',#16817,1.);
#6171=CIRCLE('',#16818,1.);
#6172=CIRCLE('',#16821,0.999999999999999);
#6173=CIRCLE('',#16824,1.);
#6174=CIRCLE('',#16833,1.);
#6175=CIRCLE('',#16835,1.);
#6176=CIRCLE('',#16837,1.);
#6177=CIRCLE('',#16839,1.);
#6178=CIRCLE('',#16843,1.);
#6179=CIRCLE('',#16844,0.999999999999999);
#6180=CIRCLE('',#16846,2.30308838114115);
#6181=CIRCLE('',#16854,4.5);
#6182=CIRCLE('',#16858,3.5);
#6183=CIRCLE('',#16859,3.5);
#6184=CIRCLE('',#16861,1.6);
#6185=CIRCLE('',#16862,1.6);
#6186=CIRCLE('',#16867,3.15);
#6187=CIRCLE('',#16868,3.35);
#6188=CIRCLE('',#16870,5.6);
#6189=CIRCLE('',#16871,5.8);
#6190=CIRCLE('',#16873,5.8);
#6191=CIRCLE('',#16874,5.6);
#6192=CIRCLE('',#16876,3.35);
#6193=CIRCLE('',#16877,3.15);
#6194=CIRCLE('',#16886,2.5);
#6195=CIRCLE('',#16887,2.5);
#6196=CIRCLE('',#16888,2.5);
#6197=CIRCLE('',#16889,2.5);
#6198=CIRCLE('',#16890,2.5);
#6199=CIRCLE('',#16891,2.5);
#6200=CIRCLE('',#16893,2.88);
#6201=CIRCLE('',#16895,4.4);
#6202=CIRCLE('',#16896,0.600000000000098);
#6203=CIRCLE('',#16897,5.);
#6204=CIRCLE('',#16898,5.);
#6205=CIRCLE('',#16900,5.);
#6206=CIRCLE('',#16902,3.0139499546386);
#6207=CIRCLE('',#16903,0.249999999998187);
#6208=CIRCLE('',#16904,3.);
#6209=CIRCLE('',#16905,3.);
#6210=CIRCLE('',#16907,3.);
#6211=CIRCLE('',#16908,3.);
#6212=CIRCLE('',#16910,3.4);
#6213=CIRCLE('',#16911,0.249999999999786);
#6214=CIRCLE('',#16912,3.1639499546386);
#6215=CIRCLE('',#16914,2.3865);
#6216=CIRCLE('',#16918,2.88);
#6217=CIRCLE('',#16920,2.88);
#6218=CIRCLE('',#16922,2.88);
#6219=CIRCLE('',#16925,2.88);
#6220=CIRCLE('',#16927,2.88);
#6221=VERTEX_POINT('',#21390);
#6222=VERTEX_POINT('',#21392);
#6223=VERTEX_POINT('',#21396);
#6224=VERTEX_POINT('',#21400);
#6225=VERTEX_POINT('',#21404);
#6226=VERTEX_POINT('',#21406);
#6227=VERTEX_POINT('',#21410);
#6228=VERTEX_POINT('',#21412);
#6229=VERTEX_POINT('',#21416);
#6230=VERTEX_POINT('',#21418);
#6231=VERTEX_POINT('',#21420);
#6232=VERTEX_POINT('',#21422);
#6233=VERTEX_POINT('',#21447);
#6234=VERTEX_POINT('',#21448);
#6235=VERTEX_POINT('',#21450);
#6236=VERTEX_POINT('',#21452);
#6237=VERTEX_POINT('',#21456);
#6238=VERTEX_POINT('',#21458);
#6239=VERTEX_POINT('',#21460);
#6240=VERTEX_POINT('',#21462);
#6241=VERTEX_POINT('',#21466);
#6242=VERTEX_POINT('',#21468);
#6243=VERTEX_POINT('',#21472);
#6244=VERTEX_POINT('',#21474);
#6245=VERTEX_POINT('',#21479);
#6246=VERTEX_POINT('',#21481);
#6247=VERTEX_POINT('',#21485);
#6248=VERTEX_POINT('',#21489);
#6249=VERTEX_POINT('',#21491);
#6250=VERTEX_POINT('',#21495);
#6251=VERTEX_POINT('',#21497);
#6252=VERTEX_POINT('',#21501);
#6253=VERTEX_POINT('',#21503);
#6254=VERTEX_POINT('',#21507);
#6255=VERTEX_POINT('',#21509);
#6256=VERTEX_POINT('',#21513);
#6257=VERTEX_POINT('',#21515);
#6258=VERTEX_POINT('',#21519);
#6259=VERTEX_POINT('',#21523);
#6260=VERTEX_POINT('',#21525);
#6261=VERTEX_POINT('',#21534);
#6262=VERTEX_POINT('',#21535);
#6263=VERTEX_POINT('',#21537);
#6264=VERTEX_POINT('',#21539);
#6265=VERTEX_POINT('',#21543);
#6266=VERTEX_POINT('',#21544);
#6267=VERTEX_POINT('',#21549);
#6268=VERTEX_POINT('',#21553);
#6269=VERTEX_POINT('',#21557);
#6270=VERTEX_POINT('',#21558);
#6271=VERTEX_POINT('',#21560);
#6272=VERTEX_POINT('',#21562);
#6273=VERTEX_POINT('',#21566);
#6274=VERTEX_POINT('',#21567);
#6275=VERTEX_POINT('',#21569);
#6276=VERTEX_POINT('',#21574);
#6277=VERTEX_POINT('',#21578);
#6278=VERTEX_POINT('',#21579);
#6279=VERTEX_POINT('',#21581);
#6280=VERTEX_POINT('',#21583);
#6281=VERTEX_POINT('',#21587);
#6282=VERTEX_POINT('',#21588);
#6283=VERTEX_POINT('',#21593);
#6284=VERTEX_POINT('',#21594);
#6285=VERTEX_POINT('',#21599);
#6286=VERTEX_POINT('',#21601);
#6287=VERTEX_POINT('',#21605);
#6288=VERTEX_POINT('',#21612);
#6289=VERTEX_POINT('',#21614);
#6290=VERTEX_POINT('',#21621);
#6291=VERTEX_POINT('',#21622);
#6292=VERTEX_POINT('',#21627);
#6293=VERTEX_POINT('',#21631);
#6294=VERTEX_POINT('',#21638);
#6295=VERTEX_POINT('',#21639);
#6296=VERTEX_POINT('',#21641);
#6297=VERTEX_POINT('',#21643);
#6298=VERTEX_POINT('',#21647);
#6299=VERTEX_POINT('',#21648);
#6300=VERTEX_POINT('',#21650);
#6301=VERTEX_POINT('',#21652);
#6302=VERTEX_POINT('',#21656);
#6303=VERTEX_POINT('',#21658);
#6304=VERTEX_POINT('',#21660);
#6305=VERTEX_POINT('',#21662);
#6306=VERTEX_POINT('',#21668);
#6307=VERTEX_POINT('',#21670);
#6308=VERTEX_POINT('',#21674);
#6309=VERTEX_POINT('',#21676);
#6310=VERTEX_POINT('',#21680);
#6311=VERTEX_POINT('',#21686);
#6312=VERTEX_POINT('',#21690);
#6313=VERTEX_POINT('',#21699);
#6314=VERTEX_POINT('',#21701);
#6315=VERTEX_POINT('',#27645);
#6316=VERTEX_POINT('',#27789);
#6317=VERTEX_POINT('',#33843);
#6318=VERTEX_POINT('',#33844);
#6319=VERTEX_POINT('',#33846);
#6320=VERTEX_POINT('',#33848);
#6321=VERTEX_POINT('',#33852);
#6322=VERTEX_POINT('',#33854);
#6323=VERTEX_POINT('',#33858);
#6324=VERTEX_POINT('',#33860);
#6325=VERTEX_POINT('',#33865);
#6326=VERTEX_POINT('',#33866);
#6327=VERTEX_POINT('',#33868);
#6328=VERTEX_POINT('',#33870);
#6329=VERTEX_POINT('',#33889);
#6330=VERTEX_POINT('',#33890);
#6331=VERTEX_POINT('',#33892);
#6332=VERTEX_POINT('',#33894);
#6333=VERTEX_POINT('',#33898);
#6334=VERTEX_POINT('',#33900);
#6335=VERTEX_POINT('',#33904);
#6336=VERTEX_POINT('',#33909);
#6337=VERTEX_POINT('',#33918);
#6338=VERTEX_POINT('',#33920);
#6339=VERTEX_POINT('',#33924);
#6340=VERTEX_POINT('',#33925);
#6341=VERTEX_POINT('',#33927);
#6342=VERTEX_POINT('',#33929);
#6343=VERTEX_POINT('',#33931);
#6344=VERTEX_POINT('',#33933);
#6345=VERTEX_POINT('',#33935);
#6346=VERTEX_POINT('',#33937);
#6347=VERTEX_POINT('',#33939);
#6348=VERTEX_POINT('',#33941);
#6349=VERTEX_POINT('',#33943);
#6350=VERTEX_POINT('',#33945);
#6351=VERTEX_POINT('',#33947);
#6352=VERTEX_POINT('',#33949);
#6353=VERTEX_POINT('',#33951);
#6354=VERTEX_POINT('',#33953);
#6355=VERTEX_POINT('',#33955);
#6356=VERTEX_POINT('',#33957);
#6357=VERTEX_POINT('',#33959);
#6358=VERTEX_POINT('',#33961);
#6359=VERTEX_POINT('',#33965);
#6360=VERTEX_POINT('',#33967);
#6361=VERTEX_POINT('',#33971);
#6362=VERTEX_POINT('',#33973);
#6363=VERTEX_POINT('',#33977);
#6364=VERTEX_POINT('',#33978);
#6365=VERTEX_POINT('',#33983);
#6366=VERTEX_POINT('',#33989);
#6367=VERTEX_POINT('',#33991);
#6368=VERTEX_POINT('',#33995);
#6369=VERTEX_POINT('',#33996);
#6370=VERTEX_POINT('',#34001);
#6371=VERTEX_POINT('',#34005);
#6372=VERTEX_POINT('',#34009);
#6373=VERTEX_POINT('',#34013);
#6374=VERTEX_POINT('',#34017);
#6375=VERTEX_POINT('',#34021);
#6376=VERTEX_POINT('',#34025);
#6377=VERTEX_POINT('',#34029);
#6378=VERTEX_POINT('',#34033);
#6379=VERTEX_POINT('',#34037);
#6380=VERTEX_POINT('',#34041);
#6381=VERTEX_POINT('',#34045);
#6382=VERTEX_POINT('',#34049);
#6383=VERTEX_POINT('',#34053);
#6384=VERTEX_POINT('',#34057);
#6385=VERTEX_POINT('',#34063);
#6386=VERTEX_POINT('',#34078);
#6387=VERTEX_POINT('',#34079);
#6388=VERTEX_POINT('',#34081);
#6389=VERTEX_POINT('',#34083);
#6390=VERTEX_POINT('',#34085);
#6391=VERTEX_POINT('',#34087);
#6392=VERTEX_POINT('',#34089);
#6393=VERTEX_POINT('',#34091);
#6394=VERTEX_POINT('',#34095);
#6395=VERTEX_POINT('',#34096);
#6396=VERTEX_POINT('',#34098);
#6397=VERTEX_POINT('',#34100);
#6398=VERTEX_POINT('',#34102);
#6399=VERTEX_POINT('',#34105);
#6400=VERTEX_POINT('',#34109);
#6401=VERTEX_POINT('',#34110);
#6402=VERTEX_POINT('',#34112);
#6403=VERTEX_POINT('',#34114);
#6404=VERTEX_POINT('',#34116);
#6405=VERTEX_POINT('',#34118);
#6406=VERTEX_POINT('',#34120);
#6407=VERTEX_POINT('',#34122);
#6408=VERTEX_POINT('',#34124);
#6409=VERTEX_POINT('',#34126);
#6410=VERTEX_POINT('',#34128);
#6411=VERTEX_POINT('',#34130);
#6412=VERTEX_POINT('',#34132);
#6413=VERTEX_POINT('',#34134);
#6414=VERTEX_POINT('',#34136);
#6415=VERTEX_POINT('',#34138);
#6416=VERTEX_POINT('',#34140);
#6417=VERTEX_POINT('',#34142);
#6418=VERTEX_POINT('',#34144);
#6419=VERTEX_POINT('',#34146);
#6420=VERTEX_POINT('',#34150);
#6421=VERTEX_POINT('',#34152);
#6422=VERTEX_POINT('',#34154);
#6423=VERTEX_POINT('',#34157);
#6424=VERTEX_POINT('',#34159);
#6425=VERTEX_POINT('',#34161);
#6426=VERTEX_POINT('',#34163);
#6427=VERTEX_POINT('',#34166);
#6428=VERTEX_POINT('',#34168);
#6429=VERTEX_POINT('',#34171);
#6430=VERTEX_POINT('',#34174);
#6431=VERTEX_POINT('',#34175);
#6432=VERTEX_POINT('',#34177);
#6433=VERTEX_POINT('',#34180);
#6434=VERTEX_POINT('',#34182);
#6435=VERTEX_POINT('',#34185);
#6436=VERTEX_POINT('',#34188);
#6437=VERTEX_POINT('',#34189);
#6438=VERTEX_POINT('',#34191);
#6439=VERTEX_POINT('',#34193);
#6440=VERTEX_POINT('',#34196);
#6441=VERTEX_POINT('',#34197);
#6442=VERTEX_POINT('',#34201);
#6443=VERTEX_POINT('',#34203);
#6444=VERTEX_POINT('',#34205);
#6445=VERTEX_POINT('',#34207);
#6446=VERTEX_POINT('',#34209);
#6447=VERTEX_POINT('',#34211);
#6448=VERTEX_POINT('',#34217);
#6449=VERTEX_POINT('',#34219);
#6450=VERTEX_POINT('',#34220);
#6451=VERTEX_POINT('',#34222);
#6452=VERTEX_POINT('',#34224);
#6453=VERTEX_POINT('',#34226);
#6454=VERTEX_POINT('',#34228);
#6455=VERTEX_POINT('',#34230);
#6456=VERTEX_POINT('',#34232);
#6457=VERTEX_POINT('',#34234);
#6458=VERTEX_POINT('',#34236);
#6459=VERTEX_POINT('',#34238);
#6460=VERTEX_POINT('',#34240);
#6461=VERTEX_POINT('',#34242);
#6462=VERTEX_POINT('',#34244);
#6463=VERTEX_POINT('',#34246);
#6464=VERTEX_POINT('',#34248);
#6465=VERTEX_POINT('',#34250);
#6466=VERTEX_POINT('',#34252);
#6467=VERTEX_POINT('',#34254);
#6468=VERTEX_POINT('',#34256);
#6469=VERTEX_POINT('',#34262);
#6470=VERTEX_POINT('',#34277);
#6471=VERTEX_POINT('',#34279);
#6472=VERTEX_POINT('',#34283);
#6473=VERTEX_POINT('',#34287);
#6474=VERTEX_POINT('',#34289);
#6475=VERTEX_POINT('',#34291);
#6476=VERTEX_POINT('',#34293);
#6477=VERTEX_POINT('',#34295);
#6478=VERTEX_POINT('',#34297);
#6479=VERTEX_POINT('',#34299);
#6480=VERTEX_POINT('',#34301);
#6481=VERTEX_POINT('',#34303);
#6482=VERTEX_POINT('',#34305);
#6483=VERTEX_POINT('',#34307);
#6484=VERTEX_POINT('',#34309);
#6485=VERTEX_POINT('',#34311);
#6486=VERTEX_POINT('',#34313);
#6487=VERTEX_POINT('',#34315);
#6488=VERTEX_POINT('',#34317);
#6489=VERTEX_POINT('',#34319);
#6490=VERTEX_POINT('',#34377);
#6491=VERTEX_POINT('',#34378);
#6492=VERTEX_POINT('',#34380);
#6493=VERTEX_POINT('',#34382);
#6494=VERTEX_POINT('',#34384);
#6495=VERTEX_POINT('',#34386);
#6496=VERTEX_POINT('',#34388);
#6497=VERTEX_POINT('',#34390);
#6498=VERTEX_POINT('',#34392);
#6499=VERTEX_POINT('',#34394);
#6500=VERTEX_POINT('',#34396);
#6501=VERTEX_POINT('',#34398);
#6502=VERTEX_POINT('',#34400);
#6503=VERTEX_POINT('',#34402);
#6504=VERTEX_POINT('',#34404);
#6505=VERTEX_POINT('',#34406);
#6506=VERTEX_POINT('',#34408);
#6507=VERTEX_POINT('',#34410);
#6508=VERTEX_POINT('',#34412);
#6509=VERTEX_POINT('',#34414);
#6510=VERTEX_POINT('',#34477);
#6511=VERTEX_POINT('',#34478);
#6512=VERTEX_POINT('',#34480);
#6513=VERTEX_POINT('',#34482);
#6514=VERTEX_POINT('',#34484);
#6515=VERTEX_POINT('',#34486);
#6516=VERTEX_POINT('',#34490);
#6517=VERTEX_POINT('',#34492);
#6518=VERTEX_POINT('',#34496);
#6519=VERTEX_POINT('',#34497);
#6520=VERTEX_POINT('',#34499);
#6521=VERTEX_POINT('',#34501);
#6522=VERTEX_POINT('',#34505);
#6523=VERTEX_POINT('',#34506);
#6524=VERTEX_POINT('',#34508);
#6525=VERTEX_POINT('',#34510);
#6526=VERTEX_POINT('',#34514);
#6527=VERTEX_POINT('',#34515);
#6528=VERTEX_POINT('',#34517);
#6529=VERTEX_POINT('',#34519);
#6530=VERTEX_POINT('',#34521);
#6531=VERTEX_POINT('',#34525);
#6532=VERTEX_POINT('',#34526);
#6533=VERTEX_POINT('',#34528);
#6534=VERTEX_POINT('',#34530);
#6535=VERTEX_POINT('',#34534);
#6536=VERTEX_POINT('',#34536);
#6537=VERTEX_POINT('',#34540);
#6538=VERTEX_POINT('',#34542);
#6539=VERTEX_POINT('',#34546);
#6540=VERTEX_POINT('',#34547);
#6541=VERTEX_POINT('',#34549);
#6542=VERTEX_POINT('',#34551);
#6543=VERTEX_POINT('',#34555);
#6544=VERTEX_POINT('',#34556);
#6545=VERTEX_POINT('',#34561);
#6546=VERTEX_POINT('',#34562);
#6547=VERTEX_POINT('',#34567);
#6548=VERTEX_POINT('',#34568);
#6549=VERTEX_POINT('',#34570);
#6550=VERTEX_POINT('',#34572);
#6551=VERTEX_POINT('',#34576);
#6552=VERTEX_POINT('',#34577);
#6553=VERTEX_POINT('',#34579);
#6554=VERTEX_POINT('',#34581);
#6555=VERTEX_POINT('',#34586);
#6556=VERTEX_POINT('',#34588);
#6557=VERTEX_POINT('',#34593);
#6558=VERTEX_POINT('',#34595);
#6559=VERTEX_POINT('',#34597);
#6560=VERTEX_POINT('',#34599);
#6561=VERTEX_POINT('',#34603);
#6562=VERTEX_POINT('',#34604);
#6563=VERTEX_POINT('',#34609);
#6564=VERTEX_POINT('',#34610);
#6565=VERTEX_POINT('',#34615);
#6566=VERTEX_POINT('',#34616);
#6567=VERTEX_POINT('',#34618);
#6568=VERTEX_POINT('',#34621);
#6569=VERTEX_POINT('',#34623);
#6570=VERTEX_POINT('',#34625);
#6571=VERTEX_POINT('',#34629);
#6572=VERTEX_POINT('',#34630);
#6573=VERTEX_POINT('',#34632);
#6574=VERTEX_POINT('',#34634);
#6575=VERTEX_POINT('',#34639);
#6576=VERTEX_POINT('',#34640);
#6577=VERTEX_POINT('',#34642);
#6578=VERTEX_POINT('',#34644);
#6579=VERTEX_POINT('',#34646);
#6580=VERTEX_POINT('',#34648);
#6581=VERTEX_POINT('',#34652);
#6582=VERTEX_POINT('',#34653);
#6583=VERTEX_POINT('',#34655);
#6584=VERTEX_POINT('',#34657);
#6585=VERTEX_POINT('',#34659);
#6586=VERTEX_POINT('',#34661);
#6587=VERTEX_POINT('',#34665);
#6588=VERTEX_POINT('',#34667);
#6589=VERTEX_POINT('',#34671);
#6590=VERTEX_POINT('',#34672);
#6591=VERTEX_POINT('',#34674);
#6592=VERTEX_POINT('',#34676);
#6593=VERTEX_POINT('',#34680);
#6594=VERTEX_POINT('',#34681);
#6595=VERTEX_POINT('',#34683);
#6596=VERTEX_POINT('',#34685);
#6597=VERTEX_POINT('',#34690);
#6598=VERTEX_POINT('',#34694);
#6599=VERTEX_POINT('',#34696);
#6600=VERTEX_POINT('',#34702);
#6601=VERTEX_POINT('',#34706);
#6602=VERTEX_POINT('',#34707);
#6603=VERTEX_POINT('',#34714);
#6604=VERTEX_POINT('',#34715);
#6605=VERTEX_POINT('',#34717);
#6606=VERTEX_POINT('',#34719);
#6607=VERTEX_POINT('',#34723);
#6608=VERTEX_POINT('',#34725);
#6609=VERTEX_POINT('',#34729);
#6610=VERTEX_POINT('',#34731);
#6611=VERTEX_POINT('',#34735);
#6612=VERTEX_POINT('',#34737);
#6613=VERTEX_POINT('',#34741);
#6614=VERTEX_POINT('',#34743);
#6615=VERTEX_POINT('',#34747);
#6616=VERTEX_POINT('',#34749);
#6617=VERTEX_POINT('',#34753);
#6618=VERTEX_POINT('',#34755);
#6619=VERTEX_POINT('',#34759);
#6620=VERTEX_POINT('',#34773);
#6621=VERTEX_POINT('',#34775);
#6622=VERTEX_POINT('',#34781);
#6623=VERTEX_POINT('',#34783);
#6624=VERTEX_POINT('',#34787);
#6625=VERTEX_POINT('',#34789);
#6626=VERTEX_POINT('',#34793);
#6627=VERTEX_POINT('',#34795);
#6628=VERTEX_POINT('',#34797);
#6629=VERTEX_POINT('',#34801);
#6630=VERTEX_POINT('',#34803);
#6631=VERTEX_POINT('',#34807);
#6632=VERTEX_POINT('',#34809);
#6633=VERTEX_POINT('',#34816);
#6634=VERTEX_POINT('',#34818);
#6635=VERTEX_POINT('',#34822);
#6636=VERTEX_POINT('',#34824);
#6637=VERTEX_POINT('',#34828);
#6638=VERTEX_POINT('',#34830);
#6639=VERTEX_POINT('',#34837);
#6640=VERTEX_POINT('',#34839);
#6641=VERTEX_POINT('',#34850);
#6642=VERTEX_POINT('',#34851);
#6643=VERTEX_POINT('',#34853);
#6644=VERTEX_POINT('',#34855);
#6645=VERTEX_POINT('',#34857);
#6646=VERTEX_POINT('',#34863);
#6647=VERTEX_POINT('',#34864);
#6648=VERTEX_POINT('',#34866);
#6649=VERTEX_POINT('',#34868);
#6650=VERTEX_POINT('',#34871);
#6651=VERTEX_POINT('',#34876);
#6652=VERTEX_POINT('',#34877);
#6653=VERTEX_POINT('',#34879);
#6654=VERTEX_POINT('',#34881);
#6655=VERTEX_POINT('',#34886);
#6656=VERTEX_POINT('',#34887);
#6657=VERTEX_POINT('',#34891);
#6658=VERTEX_POINT('',#34895);
#6659=VERTEX_POINT('',#34897);
#6660=VERTEX_POINT('',#34899);
#6661=VERTEX_POINT('',#34901);
#6662=VERTEX_POINT('',#34903);
#6663=VERTEX_POINT('',#34906);
#6664=VERTEX_POINT('',#34910);
#6665=VERTEX_POINT('',#34912);
#6666=VERTEX_POINT('',#34916);
#6667=VERTEX_POINT('',#34918);
#6668=VERTEX_POINT('',#34928);
#6669=VERTEX_POINT('',#34930);
#6670=VERTEX_POINT('',#34938);
#6671=VERTEX_POINT('',#34942);
#6672=VERTEX_POINT('',#34944);
#6673=VERTEX_POINT('',#34946);
#6674=VERTEX_POINT('',#34950);
#6675=VERTEX_POINT('',#34952);
#6676=VERTEX_POINT('',#34957);
#6677=VERTEX_POINT('',#34959);
#6678=VERTEX_POINT('',#34963);
#6679=VERTEX_POINT('',#34965);
#6680=VERTEX_POINT('',#34972);
#6681=VERTEX_POINT('',#34976);
#6682=VERTEX_POINT('',#34980);
#6683=VERTEX_POINT('',#34982);
#6684=VERTEX_POINT('',#34986);
#6685=VERTEX_POINT('',#34988);
#6686=VERTEX_POINT('',#34993);
#6687=VERTEX_POINT('',#34997);
#6688=VERTEX_POINT('',#35002);
#6689=VERTEX_POINT('',#35004);
#6690=VERTEX_POINT('',#35006);
#6691=VERTEX_POINT('',#35009);
#6692=VERTEX_POINT('',#35013);
#6693=VERTEX_POINT('',#35017);
#6694=VERTEX_POINT('',#35024);
#6695=VERTEX_POINT('',#35026);
#6696=VERTEX_POINT('',#35030);
#6697=VERTEX_POINT('',#35034);
#6698=VERTEX_POINT('',#35036);
#6699=VERTEX_POINT('',#35038);
#6700=VERTEX_POINT('',#35046);
#6701=VERTEX_POINT('',#35053);
#6702=VERTEX_POINT('',#35059);
#6703=VERTEX_POINT('',#35066);
#6704=VERTEX_POINT('',#35068);
#6705=VERTEX_POINT('',#35072);
#6706=VERTEX_POINT('',#35076);
#6707=VERTEX_POINT('',#35080);
#6708=VERTEX_POINT('',#35084);
#6709=VERTEX_POINT('',#35088);
#6710=VERTEX_POINT('',#35092);
#6711=VERTEX_POINT('',#35106);
#6712=VERTEX_POINT('',#35107);
#6713=VERTEX_POINT('',#35109);
#6714=VERTEX_POINT('',#35111);
#6715=VERTEX_POINT('',#35115);
#6716=VERTEX_POINT('',#35116);
#6717=VERTEX_POINT('',#35118);
#6718=VERTEX_POINT('',#35120);
#6719=VERTEX_POINT('',#35124);
#6720=VERTEX_POINT('',#35125);
#6721=VERTEX_POINT('',#35131);
#6722=VERTEX_POINT('',#35135);
#6723=VERTEX_POINT('',#35142);
#6724=VERTEX_POINT('',#35151);
#6725=VERTEX_POINT('',#35152);
#6726=VERTEX_POINT('',#35155);
#6727=VERTEX_POINT('',#35157);
#6728=VERTEX_POINT('',#35159);
#6729=VERTEX_POINT('',#35161);
#6730=VERTEX_POINT('',#35165);
#6731=VERTEX_POINT('',#35166);
#6732=VERTEX_POINT('',#35168);
#6733=VERTEX_POINT('',#35170);
#6734=VERTEX_POINT('',#35173);
#6735=VERTEX_POINT('',#35175);
#6736=VERTEX_POINT('',#35179);
#6737=VERTEX_POINT('',#35180);
#6738=VERTEX_POINT('',#35197);
#6739=VERTEX_POINT('',#35226);
#6740=VERTEX_POINT('',#35265);
#6741=VERTEX_POINT('',#35308);
#6742=VERTEX_POINT('',#35361);
#6743=VERTEX_POINT('',#35365);
#6744=VERTEX_POINT('',#35367);
#6745=VERTEX_POINT('',#35369);
#6746=VERTEX_POINT('',#35413);
#6747=VERTEX_POINT('',#35451);
#6748=VERTEX_POINT('',#35539);
#6749=VERTEX_POINT('',#35543);
#6750=VERTEX_POINT('',#35547);
#6751=VERTEX_POINT('',#35549);
#6752=VERTEX_POINT('',#35553);
#6753=VERTEX_POINT('',#35554);
#6754=VERTEX_POINT('',#35557);
#6755=VERTEX_POINT('',#35561);
#6756=VERTEX_POINT('',#35562);
#6757=VERTEX_POINT('',#35567);
#6758=VERTEX_POINT('',#35568);
#6759=VERTEX_POINT('',#35570);
#6760=VERTEX_POINT('',#35572);
#6761=VERTEX_POINT('',#35574);
#6762=VERTEX_POINT('',#35576);
#6763=VERTEX_POINT('',#35578);
#6764=VERTEX_POINT('',#35591);
#6765=VERTEX_POINT('',#35593);
#6766=VERTEX_POINT('',#35606);
#6767=VERTEX_POINT('',#35608);
#6768=VERTEX_POINT('',#35610);
#6769=VERTEX_POINT('',#35612);
#6770=VERTEX_POINT('',#35617);
#6771=VERTEX_POINT('',#35619);
#6772=VERTEX_POINT('',#35621);
#6773=VERTEX_POINT('',#35623);
#6774=VERTEX_POINT('',#35625);
#6775=VERTEX_POINT('',#35644);
#6776=VERTEX_POINT('',#35646);
#6777=VERTEX_POINT('',#35648);
#6778=VERTEX_POINT('',#35678);
#6779=VERTEX_POINT('',#35716);
#6780=VERTEX_POINT('',#35718);
#6781=VERTEX_POINT('',#35720);
#6782=VERTEX_POINT('',#35727);
#6783=VERTEX_POINT('',#35763);
#6784=VERTEX_POINT('',#35767);
#6785=VERTEX_POINT('',#35768);
#6786=VERTEX_POINT('',#35770);
#6787=VERTEX_POINT('',#35785);
#6788=VERTEX_POINT('',#35802);
#6789=VERTEX_POINT('',#35803);
#6790=VERTEX_POINT('',#35805);
#6791=VERTEX_POINT('',#35820);
#6792=VERTEX_POINT('',#35837);
#6793=VERTEX_POINT('',#35838);
#6794=VERTEX_POINT('',#35840);
#6795=VERTEX_POINT('',#35842);
#6796=VERTEX_POINT('',#35846);
#6797=VERTEX_POINT('',#35848);
#6798=VERTEX_POINT('',#35931);
#6799=VERTEX_POINT('',#36014);
#6800=VERTEX_POINT('',#36016);
#6801=VERTEX_POINT('',#36057);
#6802=VERTEX_POINT('',#36059);
#6803=VERTEX_POINT('',#36061);
#6804=VERTEX_POINT('',#36072);
#6805=VERTEX_POINT('',#36074);
#6806=VERTEX_POINT('',#36076);
#6807=VERTEX_POINT('',#36078);
#6808=VERTEX_POINT('',#36082);
#6809=VERTEX_POINT('',#36101);
#6810=VERTEX_POINT('',#36103);
#6811=VERTEX_POINT('',#36118);
#6812=VERTEX_POINT('',#36120);
#6813=VERTEX_POINT('',#36135);
#6814=VERTEX_POINT('',#36136);
#6815=VERTEX_POINT('',#36138);
#6816=VERTEX_POINT('',#36140);
#6817=VERTEX_POINT('',#36144);
#6818=VERTEX_POINT('',#36148);
#6819=VERTEX_POINT('',#36150);
#6820=VERTEX_POINT('',#36154);
#6821=VERTEX_POINT('',#36156);
#6822=VERTEX_POINT('',#36158);
#6823=VERTEX_POINT('',#36160);
#6824=VERTEX_POINT('',#36345);
#6825=VERTEX_POINT('',#36348);
#6826=VERTEX_POINT('',#36350);
#6827=VERTEX_POINT('',#36354);
#6828=VERTEX_POINT('',#36356);
#6829=VERTEX_POINT('',#36358);
#6830=VERTEX_POINT('',#36362);
#6831=VERTEX_POINT('',#36364);
#6832=VERTEX_POINT('',#36368);
#6833=VERTEX_POINT('',#36369);
#6834=VERTEX_POINT('',#36371);
#6835=VERTEX_POINT('',#36392);
#6836=VERTEX_POINT('',#36397);
#6837=VERTEX_POINT('',#36414);
#6838=VERTEX_POINT('',#36415);
#6839=VERTEX_POINT('',#36417);
#6840=VERTEX_POINT('',#36512);
#6841=VERTEX_POINT('',#36537);
#6842=VERTEX_POINT('',#36581);
#6843=VERTEX_POINT('',#36583);
#6844=VERTEX_POINT('',#36585);
#6845=VERTEX_POINT('',#36596);
#6846=VERTEX_POINT('',#36598);
#6847=VERTEX_POINT('',#36600);
#6848=VERTEX_POINT('',#36602);
#6849=VERTEX_POINT('',#36604);
#6850=VERTEX_POINT('',#36606);
#6851=VERTEX_POINT('',#36608);
#6852=VERTEX_POINT('',#36610);
#6853=VERTEX_POINT('',#36612);
#6854=VERTEX_POINT('',#36633);
#6855=VERTEX_POINT('',#36635);
#6856=VERTEX_POINT('',#36640);
#6857=VERTEX_POINT('',#36674);
#6858=VERTEX_POINT('',#36676);
#6859=VERTEX_POINT('',#36680);
#6860=VERTEX_POINT('',#36695);
#6861=VERTEX_POINT('',#36699);
#6862=VERTEX_POINT('',#36700);
#6863=VERTEX_POINT('',#36702);
#6864=VERTEX_POINT('',#36717);
#6865=VERTEX_POINT('',#36734);
#6866=VERTEX_POINT('',#36735);
#6867=VERTEX_POINT('',#36737);
#6868=VERTEX_POINT('',#36750);
#6869=VERTEX_POINT('',#38297);
#6870=VERTEX_POINT('',#38299);
#6871=VERTEX_POINT('',#38959);
#6872=VERTEX_POINT('',#38961);
#6873=VERTEX_POINT('',#41335);
#6874=VERTEX_POINT('',#41337);
#6875=VERTEX_POINT('',#41349);
#6876=VERTEX_POINT('',#41350);
#6877=VERTEX_POINT('',#41352);
#6878=VERTEX_POINT('',#41354);
#6879=VERTEX_POINT('',#41358);
#6880=VERTEX_POINT('',#41359);
#6881=VERTEX_POINT('',#41361);
#6882=VERTEX_POINT('',#41363);
#6883=VERTEX_POINT('',#41367);
#6884=VERTEX_POINT('',#41368);
#6885=VERTEX_POINT('',#41370);
#6886=VERTEX_POINT('',#41372);
#6887=VERTEX_POINT('',#41382);
#6888=VERTEX_POINT('',#41399);
#6889=VERTEX_POINT('',#41415);
#6890=VERTEX_POINT('',#41432);
#6891=VERTEX_POINT('',#41453);
#6892=VERTEX_POINT('',#41468);
#6893=VERTEX_POINT('',#41470);
#6894=VERTEX_POINT('',#41487);
#6895=VERTEX_POINT('',#41488);
#6896=VERTEX_POINT('',#41490);
#6897=VERTEX_POINT('',#41492);
#6898=VERTEX_POINT('',#41499);
#6899=VERTEX_POINT('',#41500);
#6900=VERTEX_POINT('',#41502);
#6901=VERTEX_POINT('',#41504);
#6902=VERTEX_POINT('',#41633);
#6903=VERTEX_POINT('',#41634);
#6904=VERTEX_POINT('',#41645);
#6905=VERTEX_POINT('',#41647);
#6906=VERTEX_POINT('',#41651);
#6907=VERTEX_POINT('',#41653);
#6908=VERTEX_POINT('',#41956);
#6909=VERTEX_POINT('',#41960);
#6910=VERTEX_POINT('',#41963);
#6911=VERTEX_POINT('',#41970);
#6912=VERTEX_POINT('',#41985);
#6913=VERTEX_POINT('',#41998);
#6914=VERTEX_POINT('',#42000);
#6915=VERTEX_POINT('',#42009);
#6916=VERTEX_POINT('',#42013);
#6917=VERTEX_POINT('',#42015);
#6918=VERTEX_POINT('',#42032);
#6919=VERTEX_POINT('',#42233);
#6920=VERTEX_POINT('',#42234);
#6921=VERTEX_POINT('',#42398);
#6922=VERTEX_POINT('',#42412);
#6923=VERTEX_POINT('',#42517);
#6924=VERTEX_POINT('',#42642);
#6925=VERTEX_POINT('',#42763);
#6926=VERTEX_POINT('',#42868);
#6927=VERTEX_POINT('',#42972);
#6928=VERTEX_POINT('',#43116);
#6929=VERTEX_POINT('',#43120);
#6930=VERTEX_POINT('',#43122);
#6931=VERTEX_POINT('',#43135);
#6932=VERTEX_POINT('',#43137);
#6933=VERTEX_POINT('',#43139);
#6934=VERTEX_POINT('',#43143);
#6935=VERTEX_POINT('',#43144);
#6936=VERTEX_POINT('',#43146);
#6937=VERTEX_POINT('',#43178);
#6938=VERTEX_POINT('',#43185);
#6939=VERTEX_POINT('',#43186);
#6940=VERTEX_POINT('',#43191);
#6941=VERTEX_POINT('',#43195);
#6942=VERTEX_POINT('',#43201);
#6943=VERTEX_POINT('',#43202);
#6944=VERTEX_POINT('',#43205);
#6945=VERTEX_POINT('',#43209);
#6946=VERTEX_POINT('',#43210);
#6947=VERTEX_POINT('',#43212);
#6948=VERTEX_POINT('',#43214);
#6949=VERTEX_POINT('',#43222);
#6950=VERTEX_POINT('',#43224);
#6951=VERTEX_POINT('',#43228);
#6952=VERTEX_POINT('',#43285);
#6953=VERTEX_POINT('',#43351);
#6954=VERTEX_POINT('',#43364);
#6955=VERTEX_POINT('',#43379);
#6956=VERTEX_POINT('',#43396);
#6957=VERTEX_POINT('',#43400);
#6958=VERTEX_POINT('',#43731);
#6959=VERTEX_POINT('',#43752);
#6960=VERTEX_POINT('',#43754);
#6961=VERTEX_POINT('',#43757);
#6962=VERTEX_POINT('',#43758);
#6963=VERTEX_POINT('',#43760);
#6964=VERTEX_POINT('',#43762);
#6965=VERTEX_POINT('',#43784);
#6966=VERTEX_POINT('',#43786);
#6967=VERTEX_POINT('',#43791);
#6968=VERTEX_POINT('',#43793);
#6969=VERTEX_POINT('',#43797);
#6970=VERTEX_POINT('',#43798);
#6971=VERTEX_POINT('',#43800);
#6972=VERTEX_POINT('',#43802);
#6973=VERTEX_POINT('',#43806);
#6974=VERTEX_POINT('',#43808);
#6975=VERTEX_POINT('',#43813);
#6976=VERTEX_POINT('',#43918);
#6977=VERTEX_POINT('',#43976);
#6978=VERTEX_POINT('',#43978);
#6979=VERTEX_POINT('',#44426);
#6980=VERTEX_POINT('',#44438);
#6981=VERTEX_POINT('',#44440);
#6982=VERTEX_POINT('',#44441);
#6983=VERTEX_POINT('',#44443);
#6984=VERTEX_POINT('',#44445);
#6985=VERTEX_POINT('',#44447);
#6986=VERTEX_POINT('',#44449);
#6987=VERTEX_POINT('',#44451);
#6988=VERTEX_POINT('',#44453);
#6989=VERTEX_POINT('',#44455);
#6990=VERTEX_POINT('',#44457);
#6991=VERTEX_POINT('',#44459);
#6992=VERTEX_POINT('',#44461);
#6993=VERTEX_POINT('',#44465);
#6994=VERTEX_POINT('',#44466);
#6995=VERTEX_POINT('',#44468);
#6996=VERTEX_POINT('',#44473);
#6997=VERTEX_POINT('',#44477);
#6998=VERTEX_POINT('',#44482);
#6999=VERTEX_POINT('',#44484);
#7000=VERTEX_POINT('',#44488);
#7001=VERTEX_POINT('',#44492);
#7002=VERTEX_POINT('',#44496);
#7003=VERTEX_POINT('',#44500);
#7004=VERTEX_POINT('',#44504);
#7005=VERTEX_POINT('',#44508);
#7006=VERTEX_POINT('',#44512);
#7007=VERTEX_POINT('',#44516);
#7008=VERTEX_POINT('',#44520);
#7009=VERTEX_POINT('',#44524);
#7010=VERTEX_POINT('',#44533);
#7011=VERTEX_POINT('',#44534);
#7012=VERTEX_POINT('',#44536);
#7013=VERTEX_POINT('',#44538);
#7014=VERTEX_POINT('',#44549);
#7015=VERTEX_POINT('',#44551);
#7016=VERTEX_POINT('',#44562);
#7017=VERTEX_POINT('',#44564);
#7018=VERTEX_POINT('',#44567);
#7019=VERTEX_POINT('',#44569);
#7020=VERTEX_POINT('',#44573);
#7021=VERTEX_POINT('',#44574);
#7022=VERTEX_POINT('',#44576);
#7023=VERTEX_POINT('',#44578);
#7024=VERTEX_POINT('',#44581);
#7025=VERTEX_POINT('',#44583);
#7026=VERTEX_POINT('',#44587);
#7027=VERTEX_POINT('',#44588);
#7028=VERTEX_POINT('',#44590);
#7029=VERTEX_POINT('',#44592);
#7030=VERTEX_POINT('',#44603);
#7031=VERTEX_POINT('',#44605);
#7032=VERTEX_POINT('',#44616);
#7033=VERTEX_POINT('',#44618);
#7034=VERTEX_POINT('',#44620);
#7035=VERTEX_POINT('',#44622);
#7036=VERTEX_POINT('',#44633);
#7037=VERTEX_POINT('',#44635);
#7038=VERTEX_POINT('',#44647);
#7039=VERTEX_POINT('',#44649);
#7040=VERTEX_POINT('',#44652);
#7041=VERTEX_POINT('',#44654);
#7042=VERTEX_POINT('',#44658);
#7043=VERTEX_POINT('',#44660);
#7044=VERTEX_POINT('',#44662);
#7045=VERTEX_POINT('',#44664);
#7046=VERTEX_POINT('',#44675);
#7047=VERTEX_POINT('',#44677);
#7048=VERTEX_POINT('',#44688);
#7049=VERTEX_POINT('',#44690);
#7050=VERTEX_POINT('',#44692);
#7051=VERTEX_POINT('',#44694);
#7052=VERTEX_POINT('',#44698);
#7053=VERTEX_POINT('',#44699);
#7054=VERTEX_POINT('',#44701);
#7055=VERTEX_POINT('',#44703);
#7056=VERTEX_POINT('',#44714);
#7057=VERTEX_POINT('',#44716);
#7058=VERTEX_POINT('',#44727);
#7059=VERTEX_POINT('',#44729);
#7060=VERTEX_POINT('',#44731);
#7061=VERTEX_POINT('',#44733);
#7062=VERTEX_POINT('',#44744);
#7063=VERTEX_POINT('',#44746);
#7064=VERTEX_POINT('',#44759);
#7065=VERTEX_POINT('',#44760);
#7066=VERTEX_POINT('',#44762);
#7067=VERTEX_POINT('',#44764);
#7068=VERTEX_POINT('',#44775);
#7069=VERTEX_POINT('',#44777);
#7070=VERTEX_POINT('',#44788);
#7071=VERTEX_POINT('',#44790);
#7072=VERTEX_POINT('',#44792);
#7073=VERTEX_POINT('',#44794);
#7074=VERTEX_POINT('',#44805);
#7075=VERTEX_POINT('',#44807);
#7076=VERTEX_POINT('',#44820);
#7077=VERTEX_POINT('',#44822);
#7078=VERTEX_POINT('',#44826);
#7079=VERTEX_POINT('',#44828);
#7080=VERTEX_POINT('',#44832);
#7081=VERTEX_POINT('',#44834);
#7082=VERTEX_POINT('',#44838);
#7083=VERTEX_POINT('',#44839);
#7084=VERTEX_POINT('',#44841);
#7085=VERTEX_POINT('',#44843);
#7086=VERTEX_POINT('',#44847);
#7087=VERTEX_POINT('',#44849);
#7088=VERTEX_POINT('',#44853);
#7089=VERTEX_POINT('',#44855);
#7090=VERTEX_POINT('',#44859);
#7091=VERTEX_POINT('',#44861);
#7092=VERTEX_POINT('',#44863);
#7093=VERTEX_POINT('',#44865);
#7094=VERTEX_POINT('',#44867);
#7095=VERTEX_POINT('',#44869);
#7096=VERTEX_POINT('',#44873);
#7097=VERTEX_POINT('',#44875);
#7098=VERTEX_POINT('',#44879);
#7099=VERTEX_POINT('',#44881);
#7100=VERTEX_POINT('',#44885);
#7101=VERTEX_POINT('',#44887);
#7102=VERTEX_POINT('',#44889);
#7103=VERTEX_POINT('',#44891);
#7104=VERTEX_POINT('',#44893);
#7105=VERTEX_POINT('',#44895);
#7106=VERTEX_POINT('',#44899);
#7107=VERTEX_POINT('',#44901);
#7108=VERTEX_POINT('',#44905);
#7109=VERTEX_POINT('',#44907);
#7110=VERTEX_POINT('',#44913);
#7111=VERTEX_POINT('',#44915);
#7112=VERTEX_POINT('',#44926);
#7113=VERTEX_POINT('',#44927);
#7114=VERTEX_POINT('',#44929);
#7115=VERTEX_POINT('',#44931);
#7116=VERTEX_POINT('',#44939);
#7117=VERTEX_POINT('',#44941);
#7118=VERTEX_POINT('',#44947);
#7119=VERTEX_POINT('',#44949);
#7120=VERTEX_POINT('',#44953);
#7121=VERTEX_POINT('',#44955);
#7122=VERTEX_POINT('',#44963);
#7123=VERTEX_POINT('',#44965);
#7124=VERTEX_POINT('',#44978);
#7125=VERTEX_POINT('',#44980);
#7126=VERTEX_POINT('',#44984);
#7127=VERTEX_POINT('',#44986);
#7128=VERTEX_POINT('',#44991);
#7129=VERTEX_POINT('',#44993);
#7130=VERTEX_POINT('',#44997);
#7131=VERTEX_POINT('',#44999);
#7132=VERTEX_POINT('',#45013);
#7133=VERTEX_POINT('',#45014);
#7134=VERTEX_POINT('',#45016);
#7135=VERTEX_POINT('',#45018);
#7136=VERTEX_POINT('',#45022);
#7137=VERTEX_POINT('',#45024);
#7138=VERTEX_POINT('',#45028);
#7139=VERTEX_POINT('',#45031);
#7140=VERTEX_POINT('',#45033);
#7141=VERTEX_POINT('',#45038);
#7142=VERTEX_POINT('',#45040);
#7143=VERTEX_POINT('',#45046);
#7144=VERTEX_POINT('',#45065);
#7145=VERTEX_POINT('',#45066);
#7146=VERTEX_POINT('',#45068);
#7147=VERTEX_POINT('',#45070);
#7148=VERTEX_POINT('',#45078);
#7149=VERTEX_POINT('',#45080);
#7150=VERTEX_POINT('',#45085);
#7151=VERTEX_POINT('',#45087);
#7152=VERTEX_POINT('',#45104);
#7153=VERTEX_POINT('',#45105);
#7154=VERTEX_POINT('',#45107);
#7155=VERTEX_POINT('',#45109);
#7156=VERTEX_POINT('',#45113);
#7157=VERTEX_POINT('',#45115);
#7158=VERTEX_POINT('',#45119);
#7159=VERTEX_POINT('',#45120);
#7160=VERTEX_POINT('',#45122);
#7161=VERTEX_POINT('',#45124);
#7162=VERTEX_POINT('',#45128);
#7163=VERTEX_POINT('',#45130);
#7164=VERTEX_POINT('',#45134);
#7165=VERTEX_POINT('',#45136);
#7166=VERTEX_POINT('',#45140);
#7167=VERTEX_POINT('',#45142);
#7168=VERTEX_POINT('',#45146);
#7169=VERTEX_POINT('',#45148);
#7170=VERTEX_POINT('',#45152);
#7171=VERTEX_POINT('',#45154);
#7172=VERTEX_POINT('',#45158);
#7173=VERTEX_POINT('',#45162);
#7174=VERTEX_POINT('',#45165);
#7175=VERTEX_POINT('',#45171);
#7176=VERTEX_POINT('',#45180);
#7177=VERTEX_POINT('',#45181);
#7178=VERTEX_POINT('',#45194);
#7179=VERTEX_POINT('',#45197);
#7180=VERTEX_POINT('',#45216);
#7181=VERTEX_POINT('',#45234);
#7182=VERTEX_POINT('',#45235);
#7183=VERTEX_POINT('',#45294);
#7184=VERTEX_POINT('',#45295);
#7185=VERTEX_POINT('',#45297);
#7186=VERTEX_POINT('',#45299);
#7187=VERTEX_POINT('',#45303);
#7188=VERTEX_POINT('',#45304);
#7189=VERTEX_POINT('',#45306);
#7190=VERTEX_POINT('',#45308);
#7191=VERTEX_POINT('',#45312);
#7192=VERTEX_POINT('',#45316);
#7193=VERTEX_POINT('',#45318);
#7194=VERTEX_POINT('',#45322);
#7195=VERTEX_POINT('',#45326);
#7196=VERTEX_POINT('',#45328);
#7197=VERTEX_POINT('',#45332);
#7198=VERTEX_POINT('',#45334);
#7199=VERTEX_POINT('',#45338);
#7200=VERTEX_POINT('',#45340);
#7201=VERTEX_POINT('',#45344);
#7202=VERTEX_POINT('',#45346);
#7203=VERTEX_POINT('',#45350);
#7204=VERTEX_POINT('',#45351);
#7205=VERTEX_POINT('',#45353);
#7206=VERTEX_POINT('',#45355);
#7207=VERTEX_POINT('',#45359);
#7208=VERTEX_POINT('',#45361);
#7209=VERTEX_POINT('',#45365);
#7210=VERTEX_POINT('',#45367);
#7211=VERTEX_POINT('',#45371);
#7212=VERTEX_POINT('',#45375);
#7213=VERTEX_POINT('',#45377);
#7214=VERTEX_POINT('',#45384);
#7215=VERTEX_POINT('',#45386);
#7216=VERTEX_POINT('',#45390);
#7217=VERTEX_POINT('',#45391);
#7218=VERTEX_POINT('',#45393);
#7219=VERTEX_POINT('',#45395);
#7220=VERTEX_POINT('',#45399);
#7221=VERTEX_POINT('',#45401);
#7222=VERTEX_POINT('',#45405);
#7223=VERTEX_POINT('',#45407);
#7224=VERTEX_POINT('',#45409);
#7225=VERTEX_POINT('',#45413);
#7226=VERTEX_POINT('',#45415);
#7227=VERTEX_POINT('',#45419);
#7228=VERTEX_POINT('',#45421);
#7229=VERTEX_POINT('',#45425);
#7230=VERTEX_POINT('',#45427);
#7231=VERTEX_POINT('',#45431);
#7232=VERTEX_POINT('',#45433);
#7233=VERTEX_POINT('',#45437);
#7234=VERTEX_POINT('',#45439);
#7235=VERTEX_POINT('',#45443);
#7236=VERTEX_POINT('',#45445);
#7237=VERTEX_POINT('',#45449);
#7238=VERTEX_POINT('',#45450);
#7239=VERTEX_POINT('',#45455);
#7240=VERTEX_POINT('',#45456);
#7241=VERTEX_POINT('',#45458);
#7242=VERTEX_POINT('',#45460);
#7243=VERTEX_POINT('',#45464);
#7244=VERTEX_POINT('',#45465);
#7245=VERTEX_POINT('',#45467);
#7246=VERTEX_POINT('',#45469);
#7247=VERTEX_POINT('',#45473);
#7248=VERTEX_POINT('',#45475);
#7249=VERTEX_POINT('',#45477);
#7250=VERTEX_POINT('',#45481);
#7251=VERTEX_POINT('',#45489);
#7252=VERTEX_POINT('',#45492);
#7253=VERTEX_POINT('',#45494);
#7254=VERTEX_POINT('',#45498);
#7255=VERTEX_POINT('',#45500);
#7256=VERTEX_POINT('',#45502);
#7257=VERTEX_POINT('',#45508);
#7258=VERTEX_POINT('',#45509);
#7259=VERTEX_POINT('',#45511);
#7260=VERTEX_POINT('',#45513);
#7261=VERTEX_POINT('',#45518);
#7262=VERTEX_POINT('',#45520);
#7263=VERTEX_POINT('',#45524);
#7264=VERTEX_POINT('',#45529);
#7265=VERTEX_POINT('',#45533);
#7266=VERTEX_POINT('',#45536);
#7267=VERTEX_POINT('',#45540);
#7268=VERTEX_POINT('',#45546);
#7269=VERTEX_POINT('',#45558);
#7270=VERTEX_POINT('',#45570);
#7271=VERTEX_POINT('',#45571);
#7272=VERTEX_POINT('',#45584);
#7273=VERTEX_POINT('',#45586);
#7274=VERTEX_POINT('',#45588);
#7275=VERTEX_POINT('',#45590);
#7276=VERTEX_POINT('',#45594);
#7277=VERTEX_POINT('',#45596);
#7278=VERTEX_POINT('',#45600);
#7279=VERTEX_POINT('',#45601);
#7280=VERTEX_POINT('',#45747);
#7281=VERTEX_POINT('',#45752);
#7282=VERTEX_POINT('',#46033);
#7283=VERTEX_POINT('',#46038);
#7284=VERTEX_POINT('',#46085);
#7285=VERTEX_POINT('',#46087);
#7286=VERTEX_POINT('',#46089);
#7287=VERTEX_POINT('',#46098);
#7288=VERTEX_POINT('',#46100);
#7289=VERTEX_POINT('',#46112);
#7290=VERTEX_POINT('',#46154);
#7291=VERTEX_POINT('',#46341);
#7292=VERTEX_POINT('',#46342);
#7293=VERTEX_POINT('',#46365);
#7294=VERTEX_POINT('',#46367);
#7295=VERTEX_POINT('',#46369);
#7296=VERTEX_POINT('',#46371);
#7297=VERTEX_POINT('',#46655);
#7298=VERTEX_POINT('',#46657);
#7299=VERTEX_POINT('',#46680);
#7300=VERTEX_POINT('',#46682);
#7301=VERTEX_POINT('',#47028);
#7302=VERTEX_POINT('',#47032);
#7303=VERTEX_POINT('',#47033);
#7304=VERTEX_POINT('',#47035);
#7305=VERTEX_POINT('',#47037);
#7306=VERTEX_POINT('',#47039);
#7307=VERTEX_POINT('',#47296);
#7308=VERTEX_POINT('',#48195);
#7309=VERTEX_POINT('',#48228);
#7310=VERTEX_POINT('',#48230);
#7311=VERTEX_POINT('',#48342);
#7312=VERTEX_POINT('',#48366);
#7313=VERTEX_POINT('',#48368);
#7314=VERTEX_POINT('',#48370);
#7315=VERTEX_POINT('',#48372);
#7316=VERTEX_POINT('',#48397);
#7317=VERTEX_POINT('',#48399);
#7318=VERTEX_POINT('',#48401);
#7319=VERTEX_POINT('',#48565);
#7320=VERTEX_POINT('',#48567);
#7321=VERTEX_POINT('',#48906);
#7322=VERTEX_POINT('',#48908);
#7323=VERTEX_POINT('',#48910);
#7324=VERTEX_POINT('',#48912);
#7325=VERTEX_POINT('',#49044);
#7326=VERTEX_POINT('',#49045);
#7327=VERTEX_POINT('',#49047);
#7328=VERTEX_POINT('',#49469);
#7329=VERTEX_POINT('',#49862);
#7330=VERTEX_POINT('',#49863);
#7331=VERTEX_POINT('',#50108);
#7332=VERTEX_POINT('',#50112);
#7333=VERTEX_POINT('',#50113);
#7334=VERTEX_POINT('',#50120);
#7335=VERTEX_POINT('',#50239);
#7336=VERTEX_POINT('',#50241);
#7337=VERTEX_POINT('',#50243);
#7338=VERTEX_POINT('',#50245);
#7339=VERTEX_POINT('',#50309);
#7340=VERTEX_POINT('',#50703);
#7341=VERTEX_POINT('',#50704);
#7342=VERTEX_POINT('',#50706);
#7343=VERTEX_POINT('',#50708);
#7344=VERTEX_POINT('',#50712);
#7345=VERTEX_POINT('',#51501);
#7346=VERTEX_POINT('',#51503);
#7347=VERTEX_POINT('',#51505);
#7348=VERTEX_POINT('',#51627);
#7349=VERTEX_POINT('',#51640);
#7350=VERTEX_POINT('',#51644);
#7351=VERTEX_POINT('',#51647);
#7352=VERTEX_POINT('',#51776);
#7353=VERTEX_POINT('',#51777);
#7354=VERTEX_POINT('',#51849);
#7355=VERTEX_POINT('',#51972);
#7356=VERTEX_POINT('',#52118);
#7357=VERTEX_POINT('',#52120);
#7358=VERTEX_POINT('',#52124);
#7359=VERTEX_POINT('',#52125);
#7360=VERTEX_POINT('',#52132);
#7361=VERTEX_POINT('',#52134);
#7362=VERTEX_POINT('',#52138);
#7363=VERTEX_POINT('',#52140);
#7364=VERTEX_POINT('',#52143);
#7365=VERTEX_POINT('',#52144);
#7366=VERTEX_POINT('',#52182);
#7367=VERTEX_POINT('',#52183);
#7368=VERTEX_POINT('',#53019);
#7369=VERTEX_POINT('',#53021);
#7370=VERTEX_POINT('',#53419);
#7371=VERTEX_POINT('',#53423);
#7372=VERTEX_POINT('',#53424);
#7373=VERTEX_POINT('',#53426);
#7374=VERTEX_POINT('',#53428);
#7375=VERTEX_POINT('',#53432);
#7376=VERTEX_POINT('',#53433);
#7377=VERTEX_POINT('',#53435);
#7378=VERTEX_POINT('',#53446);
#7379=VERTEX_POINT('',#53448);
#7380=VERTEX_POINT('',#53459);
#7381=VERTEX_POINT('',#53461);
#7382=VERTEX_POINT('',#53472);
#7383=VERTEX_POINT('',#53485);
#7384=VERTEX_POINT('',#53487);
#7385=VERTEX_POINT('',#53507);
#7386=VERTEX_POINT('',#53568);
#7387=VERTEX_POINT('',#53569);
#7388=VERTEX_POINT('',#53582);
#7389=VERTEX_POINT('',#53605);
#7390=VERTEX_POINT('',#53625);
#7391=VERTEX_POINT('',#53684);
#7392=VERTEX_POINT('',#53686);
#7393=VERTEX_POINT('',#53707);
#7394=VERTEX_POINT('',#53709);
#7395=VERTEX_POINT('',#53711);
#7396=VERTEX_POINT('',#53713);
#7397=VERTEX_POINT('',#53835);
#7398=VERTEX_POINT('',#53836);
#7399=VERTEX_POINT('',#53844);
#7400=VERTEX_POINT('',#54038);
#7401=VERTEX_POINT('',#54040);
#7402=VERTEX_POINT('',#54064);
#7403=VERTEX_POINT('',#54500);
#7404=VERTEX_POINT('',#54501);
#7405=VERTEX_POINT('',#54503);
#7406=VERTEX_POINT('',#54506);
#7407=VERTEX_POINT('',#54510);
#7408=VERTEX_POINT('',#54512);
#7409=VERTEX_POINT('',#54516);
#7410=VERTEX_POINT('',#54518);
#7411=VERTEX_POINT('',#54522);
#7412=VERTEX_POINT('',#54523);
#7413=VERTEX_POINT('',#54525);
#7414=VERTEX_POINT('',#54529);
#7415=VERTEX_POINT('',#54530);
#7416=VERTEX_POINT('',#54532);
#7417=VERTEX_POINT('',#54534);
#7418=VERTEX_POINT('',#54538);
#7419=VERTEX_POINT('',#54540);
#7420=VERTEX_POINT('',#54542);
#7421=VERTEX_POINT('',#54546);
#7422=VERTEX_POINT('',#54550);
#7423=VERTEX_POINT('',#54551);
#7424=VERTEX_POINT('',#54556);
#7425=VERTEX_POINT('',#54560);
#7426=VERTEX_POINT('',#54562);
#7427=VERTEX_POINT('',#54566);
#7428=VERTEX_POINT('',#54567);
#7429=VERTEX_POINT('',#54632);
#7430=VERTEX_POINT('',#54688);
#7431=VERTEX_POINT('',#54690);
#7432=VERTEX_POINT('',#54695);
#7433=VERTEX_POINT('',#54697);
#7434=VERTEX_POINT('',#54834);
#7435=VERTEX_POINT('',#54967);
#7436=VERTEX_POINT('',#54971);
#7437=VERTEX_POINT('',#54975);
#7438=VERTEX_POINT('',#54977);
#7439=VERTEX_POINT('',#54981);
#7440=VERTEX_POINT('',#54983);
#7441=VERTEX_POINT('',#54987);
#7442=VERTEX_POINT('',#54998);
#7443=VERTEX_POINT('',#55002);
#7444=VERTEX_POINT('',#55004);
#7445=VERTEX_POINT('',#55008);
#7446=VERTEX_POINT('',#55012);
#7447=VERTEX_POINT('',#55018);
#7448=VERTEX_POINT('',#55020);
#7449=VERTEX_POINT('',#55024);
#7450=VERTEX_POINT('',#55026);
#7451=VERTEX_POINT('',#55033);
#7452=VERTEX_POINT('',#55101);
#7453=VERTEX_POINT('',#55105);
#7454=VERTEX_POINT('',#55106);
#7455=VERTEX_POINT('',#55120);
#7456=VERTEX_POINT('',#55121);
#7457=VERTEX_POINT('',#55126);
#7458=VERTEX_POINT('',#55127);
#7459=VERTEX_POINT('',#55132);
#7460=VERTEX_POINT('',#55133);
#7461=VERTEX_POINT('',#55136);
#7462=VERTEX_POINT('',#55138);
#7463=VERTEX_POINT('',#55142);
#7464=VERTEX_POINT('',#55146);
#7465=VERTEX_POINT('',#55150);
#7466=VERTEX_POINT('',#55154);
#7467=VERTEX_POINT('',#55631);
#7468=VERTEX_POINT('',#55775);
#7469=VERTEX_POINT('',#56057);
#7470=VERTEX_POINT('',#56059);
#7471=VERTEX_POINT('',#56063);
#7472=VERTEX_POINT('',#56064);
#7473=VERTEX_POINT('',#56066);
#7474=VERTEX_POINT('',#56073);
#7475=VERTEX_POINT('',#56074);
#7476=VERTEX_POINT('',#56079);
#7477=VERTEX_POINT('',#56080);
#7478=VERTEX_POINT('',#56082);
#7479=VERTEX_POINT('',#56086);
#7480=VERTEX_POINT('',#56087);
#7481=VERTEX_POINT('',#56092);
#7482=VERTEX_POINT('',#56093);
#7483=VERTEX_POINT('',#56098);
#7484=VERTEX_POINT('',#56102);
#7485=VERTEX_POINT('',#56103);
#7486=VERTEX_POINT('',#56108);
#7487=VERTEX_POINT('',#56109);
#7488=VERTEX_POINT('',#56114);
#7489=VERTEX_POINT('',#56118);
#7490=VERTEX_POINT('',#56119);
#7491=VERTEX_POINT('',#56124);
#7492=VERTEX_POINT('',#56126);
#7493=VERTEX_POINT('',#56130);
#7494=VERTEX_POINT('',#56131);
#7495=VERTEX_POINT('',#56133);
#7496=VERTEX_POINT('',#56140);
#7497=VERTEX_POINT('',#56141);
#7498=VERTEX_POINT('',#56147);
#7499=VERTEX_POINT('',#56154);
#7500=VERTEX_POINT('',#56156);
#7501=VERTEX_POINT('',#56160);
#7502=VERTEX_POINT('',#56170);
#7503=VERTEX_POINT('',#56172);
#7504=VERTEX_POINT('',#56177);
#7505=VERTEX_POINT('',#56179);
#7506=VERTEX_POINT('',#56183);
#7507=VERTEX_POINT('',#56187);
#7508=VERTEX_POINT('',#56198);
#7509=VERTEX_POINT('',#56200);
#7510=VERTEX_POINT('',#56206);
#7511=VERTEX_POINT('',#56209);
#7512=VERTEX_POINT('',#56211);
#7513=VERTEX_POINT('',#56215);
#7514=VERTEX_POINT('',#56216);
#7515=VERTEX_POINT('',#56221);
#7516=VERTEX_POINT('',#56222);
#7517=VERTEX_POINT('',#56224);
#7518=VERTEX_POINT('',#56226);
#7519=VERTEX_POINT('',#56228);
#7520=VERTEX_POINT('',#56233);
#7521=VERTEX_POINT('',#56235);
#7522=VERTEX_POINT('',#56237);
#7523=VERTEX_POINT('',#56241);
#7524=VERTEX_POINT('',#56248);
#7525=VERTEX_POINT('',#56250);
#7526=VERTEX_POINT('',#56255);
#7527=VERTEX_POINT('',#56263);
#7528=VERTEX_POINT('',#56265);
#7529=VERTEX_POINT('',#56396);
#7530=VERTEX_POINT('',#56446);
#7531=VERTEX_POINT('',#56448);
#7532=VERTEX_POINT('',#56463);
#7533=VERTEX_POINT('',#56465);
#7534=VERTEX_POINT('',#56472);
#7535=VERTEX_POINT('',#57047);
#7536=VERTEX_POINT('',#57049);
#7537=VERTEX_POINT('',#58856);
#7538=VERTEX_POINT('',#58860);
#7539=VERTEX_POINT('',#58965);
#7540=VERTEX_POINT('',#58995);
#7541=VERTEX_POINT('',#58999);
#7542=VERTEX_POINT('',#59003);
#7543=VERTEX_POINT('',#59005);
#7544=VERTEX_POINT('',#59008);
#7545=VERTEX_POINT('',#59010);
#7546=VERTEX_POINT('',#59012);
#7547=VERTEX_POINT('',#59018);
#7548=VERTEX_POINT('',#59021);
#7549=VERTEX_POINT('',#59030);
#7550=VERTEX_POINT('',#59032);
#7551=VERTEX_POINT('',#59038);
#7552=VERTEX_POINT('',#59042);
#7553=VERTEX_POINT('',#59049);
#7554=VERTEX_POINT('',#59203);
#7555=VERTEX_POINT('',#60712);
#7556=VERTEX_POINT('',#62604);
#7557=VERTEX_POINT('',#62615);
#7558=VERTEX_POINT('',#62633);
#7559=VERTEX_POINT('',#62635);
#7560=VERTEX_POINT('',#62643);
#7561=VERTEX_POINT('',#62645);
#7562=VERTEX_POINT('',#62649);
#7563=VERTEX_POINT('',#62651);
#7564=VERTEX_POINT('',#62658);
#7565=VERTEX_POINT('',#62659);
#7566=VERTEX_POINT('',#62661);
#7567=VERTEX_POINT('',#62672);
#7568=VERTEX_POINT('',#62685);
#7569=VERTEX_POINT('',#62686);
#7570=VERTEX_POINT('',#62688);
#7571=VERTEX_POINT('',#62699);
#7572=VERTEX_POINT('',#62712);
#7573=VERTEX_POINT('',#62713);
#7574=VERTEX_POINT('',#62715);
#7575=VERTEX_POINT('',#62726);
#7576=VERTEX_POINT('',#62739);
#7577=VERTEX_POINT('',#62740);
#7578=VERTEX_POINT('',#62742);
#7579=VERTEX_POINT('',#62753);
#7580=VERTEX_POINT('',#62781);
#7581=VERTEX_POINT('',#62782);
#7582=VERTEX_POINT('',#62784);
#7583=VERTEX_POINT('',#62786);
#7584=VERTEX_POINT('',#62788);
#7585=VERTEX_POINT('',#62790);
#7586=VERTEX_POINT('',#62792);
#7587=VERTEX_POINT('',#62796);
#7588=VERTEX_POINT('',#62797);
#7589=VERTEX_POINT('',#62803);
#7590=VERTEX_POINT('',#62805);
#7591=VERTEX_POINT('',#62807);
#7592=VERTEX_POINT('',#62811);
#7593=VERTEX_POINT('',#62815);
#7594=VERTEX_POINT('',#62817);
#7595=VERTEX_POINT('',#62819);
#7596=VERTEX_POINT('',#62823);
#7597=VERTEX_POINT('',#62825);
#7598=VERTEX_POINT('',#62829);
#7599=VERTEX_POINT('',#62831);
#7600=VERTEX_POINT('',#62835);
#7601=VERTEX_POINT('',#62842);
#7602=VERTEX_POINT('',#62843);
#7603=VERTEX_POINT('',#62849);
#7604=VERTEX_POINT('',#62850);
#7605=VERTEX_POINT('',#62856);
#7606=VERTEX_POINT('',#62857);
#7607=VERTEX_POINT('',#62863);
#7608=VERTEX_POINT('',#62867);
#7609=VERTEX_POINT('',#62868);
#7610=VERTEX_POINT('',#62874);
#7611=VERTEX_POINT('',#62875);
#7612=VERTEX_POINT('',#62881);
#7613=VERTEX_POINT('',#62885);
#7614=VERTEX_POINT('',#62890);
#7615=VERTEX_POINT('',#62893);
#7616=VERTEX_POINT('',#62898);
#7617=VERTEX_POINT('',#62903);
#7618=VERTEX_POINT('',#62905);
#7619=VERTEX_POINT('',#62911);
#7620=VERTEX_POINT('',#62913);
#7621=VERTEX_POINT('',#62917);
#7622=VERTEX_POINT('',#62919);
#7623=EDGE_CURVE('',#6221,#6221,#5509,.T.);
#7624=EDGE_CURVE('',#6221,#6222,#5510,.T.);
#7625=EDGE_CURVE('',#6222,#6222,#5511,.T.);
#7626=EDGE_CURVE('',#6221,#6223,#1057,.T.);
#7627=EDGE_CURVE('',#6223,#6223,#5512,.T.);
#7628=EDGE_CURVE('',#6224,#6224,#5513,.T.);
#7629=EDGE_CURVE('',#6224,#6222,#1058,.T.);
#7630=EDGE_CURVE('',#6225,#6225,#5514,.T.);
#7631=EDGE_CURVE('',#6225,#6226,#1059,.T.);
#7632=EDGE_CURVE('',#6226,#6226,#5515,.T.);
#7633=EDGE_CURVE('',#6227,#6227,#5516,.T.);
#7634=EDGE_CURVE('',#6227,#6228,#1060,.T.);
#7635=EDGE_CURVE('',#6228,#6228,#5517,.T.);
#7636=EDGE_CURVE('',#6229,#6229,#5518,.T.);
#7637=EDGE_CURVE('',#6229,#6230,#1061,.T.);
#7638=EDGE_CURVE('',#6231,#6230,#5519,.T.);
#7639=EDGE_CURVE('',#6231,#6232,#795,.T.);
#7640=EDGE_CURVE('',#6230,#6232,#5520,.T.);
#7641=EDGE_CURVE('',#6233,#6234,#5521,.T.);
#7642=EDGE_CURVE('',#6235,#6233,#1062,.T.);
#7643=EDGE_CURVE('',#6235,#6236,#5522,.T.);
#7644=EDGE_CURVE('',#6236,#6234,#1063,.T.);
#7645=EDGE_CURVE('',#6232,#6237,#735,.T.);
#7646=EDGE_CURVE('',#6237,#6238,#5523,.T.);
#7647=EDGE_CURVE('',#6238,#6239,#5524,.T.);
#7648=EDGE_CURVE('',#6239,#6240,#5525,.T.);
#7649=EDGE_CURVE('',#6240,#6231,#736,.T.);
#7650=EDGE_CURVE('',#6241,#6241,#5526,.T.);
#7651=EDGE_CURVE('',#6241,#6242,#1064,.T.);
#7652=EDGE_CURVE('',#6242,#6242,#5527,.T.);
#7653=EDGE_CURVE('',#6243,#6243,#5528,.T.);
#7654=EDGE_CURVE('',#6243,#6244,#1065,.T.);
#7655=EDGE_CURVE('',#6238,#6244,#737,.T.);
#7656=EDGE_CURVE('',#6244,#6239,#738,.T.);
#7657=EDGE_CURVE('',#6245,#6245,#5529,.T.);
#7658=EDGE_CURVE('',#6245,#6246,#1066,.T.);
#7659=EDGE_CURVE('',#6246,#6246,#5530,.T.);
#7660=EDGE_CURVE('',#6245,#6247,#1067,.T.);
#7661=EDGE_CURVE('',#6247,#6247,#5531,.T.);
#7662=EDGE_CURVE('',#6248,#6248,#5532,.T.);
#7663=EDGE_CURVE('',#6248,#6249,#1068,.T.);
#7664=EDGE_CURVE('',#6249,#6249,#5533,.T.);
#7665=EDGE_CURVE('',#6250,#6250,#5534,.T.);
#7666=EDGE_CURVE('',#6250,#6251,#1069,.T.);
#7667=EDGE_CURVE('',#6251,#6251,#5535,.T.);
#7668=EDGE_CURVE('',#6252,#6252,#5536,.T.);
#7669=EDGE_CURVE('',#6252,#6253,#1070,.T.);
#7670=EDGE_CURVE('',#6253,#6253,#5537,.T.);
#7671=EDGE_CURVE('',#6254,#6254,#5538,.T.);
#7672=EDGE_CURVE('',#6254,#6255,#5539,.T.);
#7673=EDGE_CURVE('',#6255,#6255,#5540,.T.);
#7674=EDGE_CURVE('',#6256,#6256,#5541,.T.);
#7675=EDGE_CURVE('',#6256,#6257,#1071,.T.);
#7676=EDGE_CURVE('',#6257,#6257,#5542,.T.);
#7677=EDGE_CURVE('',#6258,#6258,#5543,.T.);
#7678=EDGE_CURVE('',#6258,#6257,#1072,.T.);
#7679=EDGE_CURVE('',#6259,#6259,#5544,.T.);
#7680=EDGE_CURVE('',#6259,#6260,#1073,.T.);
#7681=EDGE_CURVE('',#6260,#6260,#5545,.T.);
#7682=EDGE_CURVE('',#6261,#6262,#1074,.T.);
#7683=EDGE_CURVE('',#6263,#6261,#1075,.T.);
#7684=EDGE_CURVE('',#6264,#6263,#1076,.T.);
#7685=EDGE_CURVE('',#6262,#6264,#1077,.T.);
#7686=EDGE_CURVE('',#6265,#6266,#1078,.T.);
#7687=EDGE_CURVE('',#6263,#6265,#1079,.T.);
#7688=EDGE_CURVE('',#6261,#6266,#1080,.T.);
#7689=EDGE_CURVE('',#6267,#6265,#1081,.T.);
#7690=EDGE_CURVE('',#6264,#6267,#1082,.T.);
#7691=EDGE_CURVE('',#6268,#6267,#1083,.T.);
#7692=EDGE_CURVE('',#6262,#6268,#1084,.T.);
#7693=EDGE_CURVE('',#6269,#6270,#1085,.T.);
#7694=EDGE_CURVE('',#6271,#6269,#1086,.T.);
#7695=EDGE_CURVE('',#6272,#6271,#1087,.T.);
#7696=EDGE_CURVE('',#6270,#6272,#1088,.T.);
#7697=EDGE_CURVE('',#6273,#6274,#1089,.T.);
#7698=EDGE_CURVE('',#6273,#6275,#1090,.T.);
#7699=EDGE_CURVE('',#6272,#6275,#1091,.T.);
#7700=EDGE_CURVE('',#6271,#6274,#1092,.T.);
#7701=EDGE_CURVE('',#6275,#6276,#1093,.T.);
#7702=EDGE_CURVE('',#6270,#6276,#1094,.T.);
#7703=EDGE_CURVE('',#6277,#6278,#1095,.T.);
#7704=EDGE_CURVE('',#6277,#6279,#1096,.T.);
#7705=EDGE_CURVE('',#6279,#6280,#1097,.T.);
#7706=EDGE_CURVE('',#6278,#6280,#1098,.T.);
#7707=EDGE_CURVE('',#6281,#6282,#1099,.T.);
#7708=EDGE_CURVE('',#6281,#6277,#1100,.T.);
#7709=EDGE_CURVE('',#6282,#6278,#1101,.T.);
#7710=EDGE_CURVE('',#6283,#6284,#1102,.T.);
#7711=EDGE_CURVE('',#6283,#6281,#1103,.T.);
#7712=EDGE_CURVE('',#6284,#6282,#1104,.T.);
#7713=EDGE_CURVE('',#6278,#6285,#1105,.T.);
#7714=EDGE_CURVE('',#6285,#6286,#1106,.T.);
#7715=EDGE_CURVE('',#6282,#6286,#1107,.T.);
#7716=EDGE_CURVE('',#6280,#6287,#1108,.T.);
#7717=EDGE_CURVE('',#6287,#6285,#1109,.T.);
#7718=EDGE_CURVE('',#6271,#6283,#1110,.T.);
#7719=EDGE_CURVE('',#6274,#6284,#1111,.T.);
#7720=EDGE_CURVE('',#6288,#6287,#1112,.T.);
#7721=EDGE_CURVE('',#6280,#6289,#1113,.T.);
#7722=EDGE_CURVE('',#6274,#6289,#1114,.T.);
#7723=EDGE_CURVE('',#6284,#6288,#1115,.T.);
#7724=EDGE_CURVE('',#6286,#6288,#1116,.T.);
#7725=EDGE_CURVE('',#6290,#6291,#1117,.T.);
#7726=EDGE_CURVE('',#6286,#6291,#1118,.T.);
#7727=EDGE_CURVE('',#6285,#6290,#1119,.T.);
#7728=EDGE_CURVE('',#6292,#6290,#1120,.T.);
#7729=EDGE_CURVE('',#6287,#6292,#1121,.T.);
#7730=EDGE_CURVE('',#6293,#6292,#1122,.T.);
#7731=EDGE_CURVE('',#6288,#6293,#1123,.T.);
#7732=EDGE_CURVE('',#6291,#6293,#1124,.T.);
#7733=EDGE_CURVE('',#6294,#6295,#1125,.T.);
#7734=EDGE_CURVE('',#6295,#6296,#1126,.T.);
#7735=EDGE_CURVE('',#6296,#6297,#1127,.T.);
#7736=EDGE_CURVE('',#6297,#6294,#1128,.T.);
#7737=EDGE_CURVE('',#6298,#6299,#1129,.T.);
#7738=EDGE_CURVE('',#6299,#6300,#1130,.T.);
#7739=EDGE_CURVE('',#6301,#6300,#1131,.T.);
#7740=EDGE_CURVE('',#6298,#6301,#1132,.T.);
#7741=EDGE_CURVE('',#6300,#6302,#1133,.T.);
#7742=EDGE_CURVE('',#6302,#6303,#1134,.T.);
#7743=EDGE_CURVE('',#6303,#6304,#1135,.T.);
#7744=EDGE_CURVE('',#6305,#6304,#1136,.T.);
#7745=EDGE_CURVE('',#6301,#6305,#1137,.T.);
#7746=EDGE_CURVE('',#6266,#6268,#1138,.T.);
#7747=EDGE_CURVE('',#6306,#6302,#1139,.T.);
#7748=EDGE_CURVE('',#6307,#6306,#1140,.T.);
#7749=EDGE_CURVE('',#6303,#6307,#1141,.T.);
#7750=EDGE_CURVE('',#6304,#6308,#1142,.T.);
#7751=EDGE_CURVE('',#6309,#6308,#1143,.T.);
#7752=EDGE_CURVE('',#6305,#6309,#1144,.T.);
#7753=EDGE_CURVE('',#6310,#6299,#1145,.T.);
#7754=EDGE_CURVE('',#6310,#6295,#1146,.T.);
#7755=EDGE_CURVE('',#6295,#6306,#1147,.T.);
#7756=EDGE_CURVE('',#6307,#6296,#1148,.T.);
#7757=EDGE_CURVE('',#6296,#6311,#1149,.T.);
#7758=EDGE_CURVE('',#6308,#6311,#1150,.T.);
#7759=EDGE_CURVE('',#6289,#6312,#1151,.T.);
#7760=EDGE_CURVE('',#6312,#6273,#1152,.T.);
#7761=EDGE_CURVE('',#6311,#6310,#1153,.T.);
#7762=EDGE_CURVE('',#6309,#6298,#1154,.T.);
#7763=EDGE_CURVE('',#6276,#6312,#1155,.T.);
#7764=EDGE_CURVE('',#6313,#6307,#1156,.T.);
#7765=EDGE_CURVE('',#6306,#6314,#1157,.T.);
#7766=EDGE_CURVE('',#6314,#6313,#1158,.T.);
#7767=EDGE_CURVE('',#6313,#6277,#1159,.T.);
#7768=EDGE_CURVE('',#6279,#6314,#1160,.T.);
#7769=EDGE_CURVE('',#6283,#6294,#1161,.T.);
#7770=EDGE_CURVE('',#6279,#6269,#1162,.T.);
#7771=EDGE_CURVE('',#6297,#6281,#1163,.T.);
#7772=EDGE_CURVE('',#6269,#6289,#1164,.T.);
#7773=EDGE_CURVE('',#6244,#6315,#796,.T.);
#7774=EDGE_CURVE('',#6315,#6239,#5546,.T.);
#7775=EDGE_CURVE('',#6316,#6238,#5547,.T.);
#7776=EDGE_CURVE('',#6315,#6316,#5548,.T.);
#7777=EDGE_CURVE('',#6316,#6244,#797,.T.);
#7778=EDGE_CURVE('',#6317,#6318,#5549,.T.);
#7779=EDGE_CURVE('',#6319,#6317,#1165,.T.);
#7780=EDGE_CURVE('',#6319,#6320,#5550,.T.);
#7781=EDGE_CURVE('',#6320,#6318,#1166,.T.);
#7782=EDGE_CURVE('',#6318,#6321,#1167,.T.);
#7783=EDGE_CURVE('',#6320,#6322,#1168,.T.);
#7784=EDGE_CURVE('',#6322,#6321,#1169,.T.);
#7785=EDGE_CURVE('',#6321,#6323,#5551,.T.);
#7786=EDGE_CURVE('',#6322,#6324,#5552,.T.);
#7787=EDGE_CURVE('',#6324,#6323,#1170,.T.);
#7788=EDGE_CURVE('',#6325,#6326,#1171,.T.);
#7789=EDGE_CURVE('',#6327,#6325,#1172,.T.);
#7790=EDGE_CURVE('',#6327,#6328,#1173,.T.);
#7791=EDGE_CURVE('',#6328,#6326,#1174,.T.);
#7792=EDGE_CURVE('',#6323,#6325,#1175,.T.);
#7793=EDGE_CURVE('',#6324,#6327,#1176,.T.);
#7794=EDGE_CURVE('',#6326,#6233,#1177,.T.);
#7795=EDGE_CURVE('',#6328,#6235,#1178,.T.);
#7796=EDGE_CURVE('',#6234,#6317,#1179,.T.);
#7797=EDGE_CURVE('',#6236,#6319,#1180,.T.);
#7798=EDGE_CURVE('',#6329,#6330,#1181,.T.);
#7799=EDGE_CURVE('',#6331,#6330,#1182,.T.);
#7800=EDGE_CURVE('',#6332,#6331,#1183,.T.);
#7801=EDGE_CURVE('',#6332,#6329,#1184,.T.);
#7802=EDGE_CURVE('',#6333,#6329,#1185,.T.);
#7803=EDGE_CURVE('',#6334,#6332,#1186,.T.);
#7804=EDGE_CURVE('',#6334,#6333,#1187,.T.);
#7805=EDGE_CURVE('',#6335,#6333,#1188,.T.);
#7806=EDGE_CURVE('',#6330,#6335,#1189,.T.);
#7807=EDGE_CURVE('',#6336,#6335,#1190,.T.);
#7808=EDGE_CURVE('',#6331,#6336,#1191,.T.);
#7809=EDGE_CURVE('',#6336,#6334,#1192,.T.);
#7810=EDGE_CURVE('',#6337,#6337,#5553,.T.);
#7811=EDGE_CURVE('',#6337,#6338,#1193,.T.);
#7812=EDGE_CURVE('',#6338,#6338,#5554,.T.);
#7813=EDGE_CURVE('',#6339,#6340,#5555,.T.);
#7814=EDGE_CURVE('',#6340,#6341,#5556,.T.);
#7815=EDGE_CURVE('',#6341,#6342,#5557,.T.);
#7816=EDGE_CURVE('',#6342,#6343,#5558,.T.);
#7817=EDGE_CURVE('',#6343,#6344,#5559,.T.);
#7818=EDGE_CURVE('',#6344,#6345,#5560,.T.);
#7819=EDGE_CURVE('',#6345,#6346,#5561,.T.);
#7820=EDGE_CURVE('',#6346,#6347,#5562,.T.);
#7821=EDGE_CURVE('',#6347,#6348,#5563,.T.);
#7822=EDGE_CURVE('',#6348,#6349,#5564,.T.);
#7823=EDGE_CURVE('',#6349,#6350,#5565,.T.);
#7824=EDGE_CURVE('',#6350,#6351,#5566,.T.);
#7825=EDGE_CURVE('',#6351,#6352,#5567,.T.);
#7826=EDGE_CURVE('',#6352,#6353,#5568,.T.);
#7827=EDGE_CURVE('',#6353,#6354,#5569,.T.);
#7828=EDGE_CURVE('',#6354,#6355,#5570,.T.);
#7829=EDGE_CURVE('',#6355,#6356,#5571,.T.);
#7830=EDGE_CURVE('',#6356,#6357,#5572,.T.);
#7831=EDGE_CURVE('',#6357,#6358,#5573,.T.);
#7832=EDGE_CURVE('',#6358,#6339,#5574,.T.);
#7833=EDGE_CURVE('',#6359,#6359,#5575,.T.);
#7834=EDGE_CURVE('',#6359,#6360,#5576,.T.);
#7835=EDGE_CURVE('',#6360,#6360,#5577,.T.);
#7836=EDGE_CURVE('',#6360,#6361,#1194,.T.);
#7837=EDGE_CURVE('',#6361,#6362,#5578,.T.);
#7838=EDGE_CURVE('',#6362,#6361,#5579,.T.);
#7839=EDGE_CURVE('',#6363,#6364,#5580,.T.);
#7840=EDGE_CURVE('',#6364,#6362,#1195,.T.);
#7841=EDGE_CURVE('',#6364,#6363,#5581,.T.);
#7842=EDGE_CURVE('',#6365,#6365,#5582,.T.);
#7843=EDGE_CURVE('',#6365,#6363,#1196,.T.);
#7844=EDGE_CURVE('',#6343,#6366,#1197,.T.);
#7845=EDGE_CURVE('',#6366,#6367,#1198,.T.);
#7846=EDGE_CURVE('',#6344,#6367,#1199,.T.);
#7847=EDGE_CURVE('',#6368,#6369,#1200,.T.);
#7848=EDGE_CURVE('',#6369,#6341,#1201,.T.);
#7849=EDGE_CURVE('',#6340,#6368,#1202,.T.);
#7850=EDGE_CURVE('',#6339,#6370,#1203,.T.);
#7851=EDGE_CURVE('',#6370,#6368,#1204,.T.);
#7852=EDGE_CURVE('',#6358,#6371,#1205,.T.);
#7853=EDGE_CURVE('',#6371,#6370,#1206,.T.);
#7854=EDGE_CURVE('',#6357,#6372,#1207,.T.);
#7855=EDGE_CURVE('',#6372,#6371,#1208,.T.);
#7856=EDGE_CURVE('',#6373,#6356,#1209,.T.);
#7857=EDGE_CURVE('',#6373,#6372,#1210,.T.);
#7858=EDGE_CURVE('',#6374,#6373,#1211,.T.);
#7859=EDGE_CURVE('',#6355,#6374,#1212,.T.);
#7860=EDGE_CURVE('',#6354,#6375,#1213,.T.);
#7861=EDGE_CURVE('',#6375,#6374,#1214,.T.);
#7862=EDGE_CURVE('',#6353,#6376,#1215,.T.);
#7863=EDGE_CURVE('',#6376,#6375,#1216,.T.);
#7864=EDGE_CURVE('',#6352,#6377,#1217,.T.);
#7865=EDGE_CURVE('',#6377,#6376,#1218,.T.);
#7866=EDGE_CURVE('',#6378,#6351,#1219,.T.);
#7867=EDGE_CURVE('',#6378,#6377,#1220,.T.);
#7868=EDGE_CURVE('',#6379,#6378,#1221,.T.);
#7869=EDGE_CURVE('',#6350,#6379,#1222,.T.);
#7870=EDGE_CURVE('',#6349,#6380,#1223,.T.);
#7871=EDGE_CURVE('',#6380,#6379,#1224,.T.);
#7872=EDGE_CURVE('',#6348,#6381,#1225,.T.);
#7873=EDGE_CURVE('',#6381,#6380,#1226,.T.);
#7874=EDGE_CURVE('',#6347,#6382,#1227,.T.);
#7875=EDGE_CURVE('',#6382,#6381,#1228,.T.);
#7876=EDGE_CURVE('',#6383,#6346,#1229,.T.);
#7877=EDGE_CURVE('',#6383,#6382,#1230,.T.);
#7878=EDGE_CURVE('',#6384,#6383,#1231,.T.);
#7879=EDGE_CURVE('',#6345,#6384,#1232,.T.);
#7880=EDGE_CURVE('',#6367,#6384,#1233,.T.);
#7881=EDGE_CURVE('',#6369,#6385,#1234,.T.);
#7882=EDGE_CURVE('',#6385,#6366,#1235,.T.);
#7883=EDGE_CURVE('',#6342,#6385,#1236,.T.);
#7884=EDGE_CURVE('',#6386,#6387,#739,.T.);
#7885=EDGE_CURVE('',#6386,#6388,#1237,.T.);
#7886=EDGE_CURVE('',#6388,#6389,#740,.T.);
#7887=EDGE_CURVE('',#6389,#6390,#741,.T.);
#7888=EDGE_CURVE('',#6390,#6391,#742,.T.);
#7889=EDGE_CURVE('',#6392,#6391,#1238,.T.);
#7890=EDGE_CURVE('',#6393,#6392,#743,.T.);
#7891=EDGE_CURVE('',#6387,#6393,#744,.T.);
#7892=EDGE_CURVE('',#6394,#6395,#5583,.T.);
#7893=EDGE_CURVE('',#6395,#6396,#5584,.T.);
#7894=EDGE_CURVE('',#6396,#6397,#5585,.T.);
#7895=EDGE_CURVE('',#6397,#6398,#1239,.T.);
#7896=EDGE_CURVE('',#6398,#6398,#5586,.T.);
#7897=EDGE_CURVE('',#6397,#6399,#5587,.T.);
#7898=EDGE_CURVE('',#6399,#6394,#5588,.T.);
#7899=EDGE_CURVE('',#6400,#6401,#5589,.T.);
#7900=EDGE_CURVE('',#6401,#6402,#5590,.T.);
#7901=EDGE_CURVE('',#6402,#6403,#5591,.T.);
#7902=EDGE_CURVE('',#6403,#6404,#5592,.T.);
#7903=EDGE_CURVE('',#6404,#6405,#5593,.T.);
#7904=EDGE_CURVE('',#6405,#6406,#5594,.T.);
#7905=EDGE_CURVE('',#6406,#6407,#5595,.T.);
#7906=EDGE_CURVE('',#6407,#6408,#5596,.T.);
#7907=EDGE_CURVE('',#6408,#6409,#5597,.T.);
#7908=EDGE_CURVE('',#6409,#6410,#5598,.T.);
#7909=EDGE_CURVE('',#6410,#6411,#5599,.T.);
#7910=EDGE_CURVE('',#6411,#6412,#5600,.T.);
#7911=EDGE_CURVE('',#6412,#6413,#5601,.T.);
#7912=EDGE_CURVE('',#6413,#6414,#5602,.T.);
#7913=EDGE_CURVE('',#6414,#6415,#5603,.T.);
#7914=EDGE_CURVE('',#6415,#6416,#5604,.T.);
#7915=EDGE_CURVE('',#6416,#6417,#5605,.T.);
#7916=EDGE_CURVE('',#6417,#6418,#5606,.T.);
#7917=EDGE_CURVE('',#6418,#6419,#5607,.T.);
#7918=EDGE_CURVE('',#6419,#6400,#5608,.T.);
#7919=EDGE_CURVE('',#6420,#6420,#5609,.T.);
#7920=EDGE_CURVE('',#6420,#6421,#1240,.T.);
#7921=EDGE_CURVE('',#6422,#6421,#5610,.T.);
#7922=EDGE_CURVE('',#6422,#6393,#1241,.T.);
#7923=EDGE_CURVE('',#6393,#6423,#1242,.T.);
#7924=EDGE_CURVE('',#6423,#6424,#1243,.T.);
#7925=EDGE_CURVE('',#6424,#6425,#5611,.T.);
#7926=EDGE_CURVE('',#6425,#6426,#1244,.T.);
#7927=EDGE_CURVE('',#6426,#6426,#5612,.T.);
#7928=EDGE_CURVE('',#6425,#6427,#5613,.T.);
#7929=EDGE_CURVE('',#6428,#6427,#1245,.T.);
#7930=EDGE_CURVE('',#6390,#6428,#1246,.T.);
#7931=EDGE_CURVE('',#6429,#6390,#1247,.T.);
#7932=EDGE_CURVE('',#6421,#6429,#5614,.T.);
#7933=EDGE_CURVE('',#6430,#6431,#5615,.T.);
#7934=EDGE_CURVE('',#6432,#6431,#1248,.T.);
#7935=EDGE_CURVE('',#6387,#6432,#1249,.T.);
#7936=EDGE_CURVE('',#6433,#6387,#1250,.T.);
#7937=EDGE_CURVE('',#6434,#6433,#5616,.T.);
#7938=EDGE_CURVE('',#6434,#6389,#1251,.T.);
#7939=EDGE_CURVE('',#6389,#6435,#1252,.T.);
#7940=EDGE_CURVE('',#6435,#6430,#1253,.T.);
#7941=EDGE_CURVE('',#6436,#6437,#5617,.T.);
#7942=EDGE_CURVE('',#6436,#6438,#1254,.T.);
#7943=EDGE_CURVE('',#6438,#6439,#5618,.T.);
#7944=EDGE_CURVE('',#6437,#6439,#1255,.T.);
#7945=EDGE_CURVE('',#6440,#6441,#5619,.T.);
#7946=EDGE_CURVE('',#6440,#6399,#1256,.T.);
#7947=EDGE_CURVE('',#6399,#6396,#1257,.T.);
#7948=EDGE_CURVE('',#6396,#6442,#1258,.T.);
#7949=EDGE_CURVE('',#6442,#6443,#1259,.T.);
#7950=EDGE_CURVE('',#6443,#6444,#1260,.T.);
#7951=EDGE_CURVE('',#6444,#6445,#5620,.T.);
#7952=EDGE_CURVE('',#6446,#6445,#1261,.T.);
#7953=EDGE_CURVE('',#6447,#6446,#1262,.T.);
#7954=EDGE_CURVE('',#6395,#6447,#1263,.T.);
#7955=EDGE_CURVE('',#6394,#6395,#1264,.T.);
#7956=EDGE_CURVE('',#6441,#6394,#1265,.T.);
#7957=EDGE_CURVE('',#6448,#6448,#5621,.T.);
#7958=EDGE_CURVE('',#6449,#6450,#5622,.T.);
#7959=EDGE_CURVE('',#6450,#6451,#5623,.T.);
#7960=EDGE_CURVE('',#6451,#6452,#5624,.T.);
#7961=EDGE_CURVE('',#6452,#6453,#5625,.T.);
#7962=EDGE_CURVE('',#6453,#6454,#5626,.T.);
#7963=EDGE_CURVE('',#6454,#6455,#5627,.T.);
#7964=EDGE_CURVE('',#6455,#6456,#5628,.T.);
#7965=EDGE_CURVE('',#6456,#6457,#5629,.T.);
#7966=EDGE_CURVE('',#6457,#6458,#5630,.T.);
#7967=EDGE_CURVE('',#6458,#6459,#5631,.T.);
#7968=EDGE_CURVE('',#6459,#6460,#5632,.T.);
#7969=EDGE_CURVE('',#6460,#6461,#5633,.T.);
#7970=EDGE_CURVE('',#6461,#6462,#5634,.T.);
#7971=EDGE_CURVE('',#6462,#6463,#5635,.T.);
#7972=EDGE_CURVE('',#6463,#6464,#5636,.T.);
#7973=EDGE_CURVE('',#6464,#6465,#5637,.T.);
#7974=EDGE_CURVE('',#6465,#6466,#5638,.T.);
#7975=EDGE_CURVE('',#6466,#6467,#5639,.T.);
#7976=EDGE_CURVE('',#6467,#6468,#5640,.T.);
#7977=EDGE_CURVE('',#6468,#6449,#5641,.T.);
#7978=EDGE_CURVE('',#6447,#6446,#5642,.T.);
#7979=EDGE_CURVE('',#6446,#6443,#5643,.T.);
#7980=EDGE_CURVE('',#6443,#6469,#5644,.T.);
#7981=EDGE_CURVE('',#6469,#6448,#1266,.T.);
#7982=EDGE_CURVE('',#6469,#6442,#5645,.T.);
#7983=EDGE_CURVE('',#6442,#6447,#5646,.T.);
#7984=EDGE_CURVE('',#6428,#6435,#745,.T.);
#7985=EDGE_CURVE('',#6427,#6430,#1267,.T.);
#7986=EDGE_CURVE('',#6429,#6434,#1268,.T.);
#7987=EDGE_CURVE('',#6423,#6432,#746,.T.);
#7988=EDGE_CURVE('',#6431,#6424,#1269,.T.);
#7989=EDGE_CURVE('',#6470,#6451,#1270,.T.);
#7990=EDGE_CURVE('',#6470,#6471,#1271,.T.);
#7991=EDGE_CURVE('',#6452,#6471,#1272,.T.);
#7992=EDGE_CURVE('',#6471,#6472,#1273,.T.);
#7993=EDGE_CURVE('',#6453,#6472,#1274,.T.);
#7994=EDGE_CURVE('',#6473,#6470,#1275,.T.);
#7995=EDGE_CURVE('',#6474,#6473,#1276,.T.);
#7996=EDGE_CURVE('',#6475,#6474,#1277,.T.);
#7997=EDGE_CURVE('',#6476,#6475,#1278,.T.);
#7998=EDGE_CURVE('',#6477,#6476,#1279,.T.);
#7999=EDGE_CURVE('',#6478,#6477,#1280,.T.);
#8000=EDGE_CURVE('',#6479,#6478,#1281,.T.);
#8001=EDGE_CURVE('',#6480,#6479,#1282,.T.);
#8002=EDGE_CURVE('',#6481,#6480,#1283,.T.);
#8003=EDGE_CURVE('',#6482,#6481,#1284,.T.);
#8004=EDGE_CURVE('',#6483,#6482,#1285,.T.);
#8005=EDGE_CURVE('',#6484,#6483,#1286,.T.);
#8006=EDGE_CURVE('',#6485,#6484,#1287,.T.);
#8007=EDGE_CURVE('',#6486,#6485,#1288,.T.);
#8008=EDGE_CURVE('',#6487,#6486,#1289,.T.);
#8009=EDGE_CURVE('',#6488,#6487,#1290,.T.);
#8010=EDGE_CURVE('',#6489,#6488,#1291,.T.);
#8011=EDGE_CURVE('',#6472,#6489,#1292,.T.);
#8012=EDGE_CURVE('',#6454,#6489,#1293,.T.);
#8013=EDGE_CURVE('',#6455,#6488,#1294,.T.);
#8014=EDGE_CURVE('',#6487,#6456,#1295,.T.);
#8015=EDGE_CURVE('',#6457,#6486,#1296,.T.);
#8016=EDGE_CURVE('',#6458,#6485,#1297,.T.);
#8017=EDGE_CURVE('',#6459,#6484,#1298,.T.);
#8018=EDGE_CURVE('',#6460,#6483,#1299,.T.);
#8019=EDGE_CURVE('',#6482,#6461,#1300,.T.);
#8020=EDGE_CURVE('',#6462,#6481,#1301,.T.);
#8021=EDGE_CURVE('',#6463,#6480,#1302,.T.);
#8022=EDGE_CURVE('',#6464,#6479,#1303,.T.);
#8023=EDGE_CURVE('',#6465,#6478,#1304,.T.);
#8024=EDGE_CURVE('',#6477,#6466,#1305,.T.);
#8025=EDGE_CURVE('',#6467,#6476,#1306,.T.);
#8026=EDGE_CURVE('',#6468,#6475,#1307,.T.);
#8027=EDGE_CURVE('',#6449,#6474,#1308,.T.);
#8028=EDGE_CURVE('',#6450,#6473,#1309,.T.);
#8029=EDGE_CURVE('',#6445,#6444,#1310,.T.);
#8030=EDGE_CURVE('',#6433,#6422,#1311,.T.);
#8031=EDGE_CURVE('',#6441,#6440,#1312,.T.);
#8032=EDGE_CURVE('',#6439,#6438,#1313,.T.);
#8033=EDGE_CURVE('',#6437,#6436,#1314,.T.);
#8034=EDGE_CURVE('',#6490,#6491,#1315,.T.);
#8035=EDGE_CURVE('',#6492,#6490,#1316,.T.);
#8036=EDGE_CURVE('',#6493,#6492,#1317,.T.);
#8037=EDGE_CURVE('',#6494,#6493,#1318,.T.);
#8038=EDGE_CURVE('',#6495,#6494,#1319,.T.);
#8039=EDGE_CURVE('',#6496,#6495,#1320,.T.);
#8040=EDGE_CURVE('',#6497,#6496,#1321,.T.);
#8041=EDGE_CURVE('',#6498,#6497,#1322,.T.);
#8042=EDGE_CURVE('',#6499,#6498,#1323,.T.);
#8043=EDGE_CURVE('',#6500,#6499,#1324,.T.);
#8044=EDGE_CURVE('',#6501,#6500,#1325,.T.);
#8045=EDGE_CURVE('',#6502,#6501,#1326,.T.);
#8046=EDGE_CURVE('',#6503,#6502,#1327,.T.);
#8047=EDGE_CURVE('',#6504,#6503,#1328,.T.);
#8048=EDGE_CURVE('',#6505,#6504,#1329,.T.);
#8049=EDGE_CURVE('',#6506,#6505,#1330,.T.);
#8050=EDGE_CURVE('',#6507,#6506,#1331,.T.);
#8051=EDGE_CURVE('',#6508,#6507,#1332,.T.);
#8052=EDGE_CURVE('',#6509,#6508,#1333,.T.);
#8053=EDGE_CURVE('',#6491,#6509,#1334,.T.);
#8054=EDGE_CURVE('',#6400,#6493,#1335,.T.);
#8055=EDGE_CURVE('',#6401,#6492,#1336,.T.);
#8056=EDGE_CURVE('',#6419,#6494,#1337,.T.);
#8057=EDGE_CURVE('',#6418,#6495,#1338,.T.);
#8058=EDGE_CURVE('',#6496,#6417,#1339,.T.);
#8059=EDGE_CURVE('',#6416,#6497,#1340,.T.);
#8060=EDGE_CURVE('',#6415,#6498,#1341,.T.);
#8061=EDGE_CURVE('',#6414,#6499,#1342,.T.);
#8062=EDGE_CURVE('',#6413,#6500,#1343,.T.);
#8063=EDGE_CURVE('',#6501,#6412,#1344,.T.);
#8064=EDGE_CURVE('',#6411,#6502,#1345,.T.);
#8065=EDGE_CURVE('',#6410,#6503,#1346,.T.);
#8066=EDGE_CURVE('',#6409,#6504,#1347,.T.);
#8067=EDGE_CURVE('',#6408,#6505,#1348,.T.);
#8068=EDGE_CURVE('',#6506,#6407,#1349,.T.);
#8069=EDGE_CURVE('',#6406,#6507,#1350,.T.);
#8070=EDGE_CURVE('',#6405,#6508,#1351,.T.);
#8071=EDGE_CURVE('',#6404,#6509,#1352,.T.);
#8072=EDGE_CURVE('',#6403,#6491,#1353,.T.);
#8073=EDGE_CURVE('',#6490,#6402,#1354,.T.);
#8074=EDGE_CURVE('',#6435,#6388,#747,.T.);
#8075=EDGE_CURVE('',#6432,#6386,#748,.T.);
#8076=EDGE_CURVE('',#6391,#6428,#749,.T.);
#8077=EDGE_CURVE('',#6392,#6423,#750,.T.);
#8078=EDGE_CURVE('',#6510,#6511,#5647,.T.);
#8079=EDGE_CURVE('',#6512,#6510,#5648,.T.);
#8080=EDGE_CURVE('',#6513,#6512,#5649,.T.);
#8081=EDGE_CURVE('',#6514,#6513,#1355,.T.);
#8082=EDGE_CURVE('',#6514,#6515,#5650,.T.);
#8083=EDGE_CURVE('',#6515,#6511,#1356,.T.);
#8084=EDGE_CURVE('',#6516,#6516,#5651,.T.);
#8085=EDGE_CURVE('',#6516,#6517,#1357,.T.);
#8086=EDGE_CURVE('',#6517,#6517,#5652,.T.);
#8087=EDGE_CURVE('',#6518,#6519,#5653,.T.);
#8088=EDGE_CURVE('',#6520,#6518,#1358,.T.);
#8089=EDGE_CURVE('',#6520,#6521,#5654,.T.);
#8090=EDGE_CURVE('',#6521,#6519,#1359,.T.);
#8091=EDGE_CURVE('',#6522,#6523,#5655,.T.);
#8092=EDGE_CURVE('',#6524,#6522,#1360,.T.);
#8093=EDGE_CURVE('',#6524,#6525,#5656,.T.);
#8094=EDGE_CURVE('',#6525,#6523,#1361,.T.);
#8095=EDGE_CURVE('',#6526,#6527,#5657,.T.);
#8096=EDGE_CURVE('',#6528,#6526,#1362,.T.);
#8097=EDGE_CURVE('',#6528,#6529,#5658,.T.);
#8098=EDGE_CURVE('',#6529,#6530,#5659,.T.);
#8099=EDGE_CURVE('',#6530,#6527,#1363,.T.);
#8100=EDGE_CURVE('',#6531,#6532,#1364,.T.);
#8101=EDGE_CURVE('',#6533,#6532,#1365,.T.);
#8102=EDGE_CURVE('',#6534,#6533,#1366,.T.);
#8103=EDGE_CURVE('',#6534,#6531,#1367,.T.);
#8104=EDGE_CURVE('',#6535,#6531,#1368,.T.);
#8105=EDGE_CURVE('',#6536,#6534,#1369,.T.);
#8106=EDGE_CURVE('',#6536,#6535,#1370,.T.);
#8107=EDGE_CURVE('',#6537,#6535,#1371,.T.);
#8108=EDGE_CURVE('',#6538,#6536,#1372,.T.);
#8109=EDGE_CURVE('',#6538,#6537,#1373,.T.);
#8110=EDGE_CURVE('',#6539,#6540,#1374,.T.);
#8111=EDGE_CURVE('',#6541,#6539,#1375,.T.);
#8112=EDGE_CURVE('',#6542,#6541,#1376,.T.);
#8113=EDGE_CURVE('',#6540,#6542,#1377,.T.);
#8114=EDGE_CURVE('',#6543,#6544,#1378,.T.);
#8115=EDGE_CURVE('',#6541,#6543,#1379,.T.);
#8116=EDGE_CURVE('',#6539,#6544,#1380,.T.);
#8117=EDGE_CURVE('',#6545,#6546,#1381,.T.);
#8118=EDGE_CURVE('',#6540,#6545,#1382,.T.);
#8119=EDGE_CURVE('',#6542,#6546,#1383,.T.);
#8120=EDGE_CURVE('',#6547,#6548,#1384,.T.);
#8121=EDGE_CURVE('',#6548,#6549,#1385,.T.);
#8122=EDGE_CURVE('',#6549,#6550,#1386,.T.);
#8123=EDGE_CURVE('',#6550,#6547,#1387,.T.);
#8124=EDGE_CURVE('',#6551,#6552,#1388,.T.);
#8125=EDGE_CURVE('',#6551,#6553,#1389,.T.);
#8126=EDGE_CURVE('',#6553,#6554,#1390,.T.);
#8127=EDGE_CURVE('',#6554,#6552,#1391,.T.);
#8128=EDGE_CURVE('',#6549,#6551,#1392,.T.);
#8129=EDGE_CURVE('',#6552,#6555,#1393,.T.);
#8130=EDGE_CURVE('',#6555,#6556,#1394,.T.);
#8131=EDGE_CURVE('',#6550,#6556,#1395,.T.);
#8132=EDGE_CURVE('',#6553,#6548,#1396,.T.);
#8133=EDGE_CURVE('',#6557,#6547,#1397,.T.);
#8134=EDGE_CURVE('',#6558,#6557,#1398,.T.);
#8135=EDGE_CURVE('',#6559,#6558,#1399,.T.);
#8136=EDGE_CURVE('',#6559,#6560,#1400,.T.);
#8137=EDGE_CURVE('',#6560,#6554,#1401,.T.);
#8138=EDGE_CURVE('',#6561,#6562,#1402,.T.);
#8139=EDGE_CURVE('',#6559,#6561,#1403,.T.);
#8140=EDGE_CURVE('',#6558,#6562,#1404,.T.);
#8141=EDGE_CURVE('',#6563,#6564,#1405,.T.);
#8142=EDGE_CURVE('',#6557,#6563,#1406,.T.);
#8143=EDGE_CURVE('',#6547,#6564,#1407,.T.);
#8144=EDGE_CURVE('',#6565,#6566,#5660,.T.);
#8145=EDGE_CURVE('',#6567,#6566,#1408,.T.);
#8146=EDGE_CURVE('',#6550,#6567,#1409,.T.);
#8147=EDGE_CURVE('',#6568,#6556,#1410,.T.);
#8148=EDGE_CURVE('',#6569,#6568,#1411,.T.);
#8149=EDGE_CURVE('',#6569,#6570,#5661,.T.);
#8150=EDGE_CURVE('',#6570,#6565,#1412,.T.);
#8151=EDGE_CURVE('',#6571,#6572,#1413,.T.);
#8152=EDGE_CURVE('',#6573,#6572,#1414,.T.);
#8153=EDGE_CURVE('',#6574,#6573,#1415,.T.);
#8154=EDGE_CURVE('',#6567,#6574,#751,.T.);
#8155=EDGE_CURVE('',#6566,#6571,#752,.T.);
#8156=EDGE_CURVE('',#6575,#6576,#1416,.T.);
#8157=EDGE_CURVE('',#6576,#6577,#1417,.T.);
#8158=EDGE_CURVE('',#6577,#6578,#1418,.T.);
#8159=EDGE_CURVE('',#6578,#6579,#1419,.T.);
#8160=EDGE_CURVE('',#6579,#6580,#1420,.T.);
#8161=EDGE_CURVE('',#6575,#6580,#1421,.T.);
#8162=EDGE_CURVE('',#6581,#6582,#1422,.T.);
#8163=EDGE_CURVE('',#6581,#6583,#1423,.T.);
#8164=EDGE_CURVE('',#6584,#6583,#1424,.T.);
#8165=EDGE_CURVE('',#6584,#6585,#1425,.T.);
#8166=EDGE_CURVE('',#6585,#6586,#1426,.T.);
#8167=EDGE_CURVE('',#6586,#6582,#1427,.T.);
#8168=EDGE_CURVE('',#6585,#6587,#1428,.T.);
#8169=EDGE_CURVE('',#6587,#6588,#1429,.T.);
#8170=EDGE_CURVE('',#6588,#6586,#1430,.T.);
#8171=EDGE_CURVE('',#6589,#6590,#1431,.T.);
#8172=EDGE_CURVE('',#6589,#6591,#1432,.T.);
#8173=EDGE_CURVE('',#6591,#6592,#1433,.T.);
#8174=EDGE_CURVE('',#6592,#6590,#1434,.T.);
#8175=EDGE_CURVE('',#6593,#6594,#1435,.T.);
#8176=EDGE_CURVE('',#6593,#6595,#1436,.T.);
#8177=EDGE_CURVE('',#6595,#6596,#1437,.T.);
#8178=EDGE_CURVE('',#6596,#6592,#1438,.T.);
#8179=EDGE_CURVE('',#6591,#6594,#1439,.T.);
#8180=EDGE_CURVE('',#6587,#6597,#1440,.T.);
#8181=EDGE_CURVE('',#6597,#6584,#1441,.T.);
#8182=EDGE_CURVE('',#6598,#6581,#1442,.T.);
#8183=EDGE_CURVE('',#6599,#6598,#1443,.T.);
#8184=EDGE_CURVE('',#6583,#6599,#1444,.T.);
#8185=EDGE_CURVE('',#6599,#6597,#1445,.T.);
#8186=EDGE_CURVE('',#6600,#6589,#1446,.T.);
#8187=EDGE_CURVE('',#6594,#6600,#1447,.T.);
#8188=EDGE_CURVE('',#6601,#6602,#1448,.T.);
#8189=EDGE_CURVE('',#6595,#6601,#1449,.T.);
#8190=EDGE_CURVE('',#6602,#6593,#1450,.T.);
#8191=EDGE_CURVE('',#6533,#6538,#1451,.T.);
#8192=EDGE_CURVE('',#6603,#6604,#1452,.T.);
#8193=EDGE_CURVE('',#6605,#6603,#5662,.T.);
#8194=EDGE_CURVE('',#6606,#6605,#1453,.T.);
#8195=EDGE_CURVE('',#6604,#6606,#5663,.T.);
#8196=EDGE_CURVE('',#6607,#6605,#1454,.T.);
#8197=EDGE_CURVE('',#6608,#6607,#1455,.T.);
#8198=EDGE_CURVE('',#6606,#6608,#1456,.T.);
#8199=EDGE_CURVE('',#6609,#6604,#1457,.T.);
#8200=EDGE_CURVE('',#6610,#6609,#1458,.T.);
#8201=EDGE_CURVE('',#6603,#6610,#1459,.T.);
#8202=EDGE_CURVE('',#6611,#6607,#5664,.T.);
#8203=EDGE_CURVE('',#6612,#6611,#1460,.T.);
#8204=EDGE_CURVE('',#6608,#6612,#5665,.T.);
#8205=EDGE_CURVE('',#6613,#6609,#5666,.T.);
#8206=EDGE_CURVE('',#6614,#6613,#1461,.T.);
#8207=EDGE_CURVE('',#6610,#6614,#5667,.T.);
#8208=EDGE_CURVE('',#6615,#6611,#1462,.T.);
#8209=EDGE_CURVE('',#6616,#6615,#1463,.T.);
#8210=EDGE_CURVE('',#6612,#6616,#1464,.T.);
#8211=EDGE_CURVE('',#6617,#6613,#1465,.T.);
#8212=EDGE_CURVE('',#6618,#6617,#1466,.T.);
#8213=EDGE_CURVE('',#6614,#6618,#1467,.T.);
#8214=EDGE_CURVE('',#6601,#6619,#1468,.T.);
#8215=EDGE_CURVE('',#6619,#6596,#1469,.T.);
#8216=EDGE_CURVE('',#6618,#6615,#5668,.T.);
#8217=EDGE_CURVE('',#6616,#6617,#5669,.T.);
#8218=EDGE_CURVE('',#6544,#6545,#1470,.T.);
#8219=EDGE_CURVE('',#6555,#6560,#1471,.T.);
#8220=EDGE_CURVE('',#6556,#6559,#1472,.T.);
#8221=EDGE_CURVE('',#6620,#6526,#1473,.T.);
#8222=EDGE_CURVE('',#6621,#6620,#1474,.T.);
#8223=EDGE_CURVE('',#6621,#6512,#1475,.T.);
#8224=EDGE_CURVE('',#6512,#6510,#1476,.T.);
#8225=EDGE_CURVE('',#6510,#6528,#1477,.T.);
#8226=EDGE_CURVE('',#6527,#6622,#1478,.T.);
#8227=EDGE_CURVE('',#6530,#6623,#1479,.T.);
#8228=EDGE_CURVE('',#6623,#6622,#1480,.T.);
#8229=EDGE_CURVE('',#6622,#6624,#5670,.T.);
#8230=EDGE_CURVE('',#6623,#6625,#5671,.T.);
#8231=EDGE_CURVE('',#6625,#6624,#1481,.T.);
#8232=EDGE_CURVE('',#6624,#6626,#1482,.T.);
#8233=EDGE_CURVE('',#6625,#6627,#1483,.T.);
#8234=EDGE_CURVE('',#6627,#6628,#1484,.T.);
#8235=EDGE_CURVE('',#6628,#6626,#1485,.T.);
#8236=EDGE_CURVE('',#6626,#6629,#5672,.T.);
#8237=EDGE_CURVE('',#6628,#6630,#5673,.T.);
#8238=EDGE_CURVE('',#6630,#6629,#1486,.T.);
#8239=EDGE_CURVE('',#6631,#6620,#5674,.T.);
#8240=EDGE_CURVE('',#6632,#6631,#1487,.T.);
#8241=EDGE_CURVE('',#6632,#6621,#5675,.T.);
#8242=EDGE_CURVE('',#6629,#6631,#1488,.T.);
#8243=EDGE_CURVE('',#6630,#6632,#1489,.T.);
#8244=EDGE_CURVE('',#6633,#6522,#5676,.T.);
#8245=EDGE_CURVE('',#6634,#6633,#1490,.T.);
#8246=EDGE_CURVE('',#6634,#6524,#5677,.T.);
#8247=EDGE_CURVE('',#6523,#6635,#5678,.T.);
#8248=EDGE_CURVE('',#6525,#6636,#5679,.T.);
#8249=EDGE_CURVE('',#6636,#6635,#1491,.T.);
#8250=EDGE_CURVE('',#6635,#6637,#1492,.T.);
#8251=EDGE_CURVE('',#6636,#6638,#1493,.T.);
#8252=EDGE_CURVE('',#6638,#6637,#1494,.T.);
#8253=EDGE_CURVE('',#6637,#6518,#5680,.T.);
#8254=EDGE_CURVE('',#6638,#6520,#5681,.T.);
#8255=EDGE_CURVE('',#6519,#6639,#5682,.T.);
#8256=EDGE_CURVE('',#6521,#6640,#5683,.T.);
#8257=EDGE_CURVE('',#6640,#6639,#1495,.T.);
#8258=EDGE_CURVE('',#6511,#6529,#1496,.T.);
#8259=EDGE_CURVE('',#6639,#6633,#1497,.T.);
#8260=EDGE_CURVE('',#6640,#6634,#1498,.T.);
#8261=EDGE_CURVE('',#6641,#6642,#1499,.T.);
#8262=EDGE_CURVE('',#6641,#6643,#5684,.T.);
#8263=EDGE_CURVE('',#6643,#6644,#1500,.T.);
#8264=EDGE_CURVE('',#6644,#6645,#1501,.T.);
#8265=EDGE_CURVE('',#6645,#6642,#1502,.T.);
#8266=EDGE_CURVE('',#6627,#6513,#1503,.T.);
#8267=EDGE_CURVE('',#6646,#6647,#1504,.T.);
#8268=EDGE_CURVE('',#6648,#6646,#1505,.T.);
#8269=EDGE_CURVE('',#6649,#6648,#1506,.T.);
#8270=EDGE_CURVE('',#6529,#6649,#1507,.T.);
#8271=EDGE_CURVE('',#6515,#6650,#1508,.T.);
#8272=EDGE_CURVE('',#6650,#6647,#1509,.T.);
#8273=EDGE_CURVE('',#6651,#6652,#1510,.T.);
#8274=EDGE_CURVE('',#6652,#6653,#1511,.T.);
#8275=EDGE_CURVE('',#6654,#6653,#1512,.T.);
#8276=EDGE_CURVE('',#6654,#6647,#1513,.T.);
#8277=EDGE_CURVE('',#6650,#6651,#1514,.T.);
#8278=EDGE_CURVE('',#6655,#6656,#1515,.T.);
#8279=EDGE_CURVE('',#6656,#6580,#1516,.T.);
#8280=EDGE_CURVE('',#6579,#6514,#1517,.T.);
#8281=EDGE_CURVE('',#6657,#6627,#1518,.T.);
#8282=EDGE_CURVE('',#6657,#6655,#1519,.T.);
#8283=EDGE_CURVE('',#6658,#6649,#1520,.T.);
#8284=EDGE_CURVE('',#6659,#6658,#1521,.T.);
#8285=EDGE_CURVE('',#6659,#6660,#1522,.T.);
#8286=EDGE_CURVE('',#6661,#6660,#1523,.T.);
#8287=EDGE_CURVE('',#6661,#6662,#1524,.T.);
#8288=EDGE_CURVE('',#6662,#6641,#1525,.T.);
#8289=EDGE_CURVE('',#6642,#6663,#1526,.T.);
#8290=EDGE_CURVE('',#6663,#6657,#1527,.T.);
#8291=EDGE_CURVE('',#6664,#6578,#1528,.T.);
#8292=EDGE_CURVE('',#6665,#6664,#1529,.T.);
#8293=EDGE_CURVE('',#6651,#6665,#1530,.T.);
#8294=EDGE_CURVE('',#6666,#6655,#1531,.T.);
#8295=EDGE_CURVE('',#6666,#6667,#1532,.T.);
#8296=EDGE_CURVE('',#6667,#6656,#1533,.T.);
#8297=EDGE_CURVE('',#6667,#6575,#1534,.T.);
#8298=EDGE_CURVE('',#6663,#6666,#1535,.T.);
#8299=EDGE_CURVE('',#6576,#6645,#1536,.T.);
#8300=EDGE_CURVE('',#6668,#6646,#1537,.T.);
#8301=EDGE_CURVE('',#6669,#6668,#1538,.T.);
#8302=EDGE_CURVE('',#6669,#6648,#1539,.T.);
#8303=EDGE_CURVE('',#6668,#6654,#1540,.T.);
#8304=EDGE_CURVE('',#6658,#6669,#1541,.T.);
#8305=EDGE_CURVE('',#6653,#6670,#1542,.T.);
#8306=EDGE_CURVE('',#6670,#6659,#1543,.T.);
#8307=EDGE_CURVE('',#6671,#6652,#1544,.T.);
#8308=EDGE_CURVE('',#6671,#6672,#1545,.T.);
#8309=EDGE_CURVE('',#6672,#6673,#1546,.T.);
#8310=EDGE_CURVE('',#6653,#6673,#1547,.T.);
#8311=EDGE_CURVE('',#6673,#6674,#1548,.T.);
#8312=EDGE_CURVE('',#6672,#6675,#1549,.T.);
#8313=EDGE_CURVE('',#6675,#6674,#1550,.T.);
#8314=EDGE_CURVE('',#6674,#6670,#1551,.T.);
#8315=EDGE_CURVE('',#6675,#6676,#1552,.T.);
#8316=EDGE_CURVE('',#6676,#6677,#1553,.T.);
#8317=EDGE_CURVE('',#6670,#6677,#1554,.T.);
#8318=EDGE_CURVE('',#6677,#6678,#1555,.T.);
#8319=EDGE_CURVE('',#6676,#6679,#1556,.T.);
#8320=EDGE_CURVE('',#6679,#6678,#1557,.T.);
#8321=EDGE_CURVE('',#6678,#6660,#5685,.T.);
#8322=EDGE_CURVE('',#6679,#6661,#5686,.T.);
#8323=EDGE_CURVE('',#6662,#6680,#5687,.T.);
#8324=EDGE_CURVE('',#6680,#6643,#1558,.T.);
#8325=EDGE_CURVE('',#6680,#6681,#1559,.T.);
#8326=EDGE_CURVE('',#6681,#6644,#1560,.T.);
#8327=EDGE_CURVE('',#6681,#6682,#1561,.T.);
#8328=EDGE_CURVE('',#6682,#6683,#1562,.T.);
#8329=EDGE_CURVE('',#6645,#6683,#1563,.T.);
#8330=EDGE_CURVE('',#6683,#6684,#1564,.T.);
#8331=EDGE_CURVE('',#6682,#6685,#1565,.T.);
#8332=EDGE_CURVE('',#6685,#6684,#1566,.T.);
#8333=EDGE_CURVE('',#6684,#6576,#1567,.T.);
#8334=EDGE_CURVE('',#6685,#6686,#1568,.T.);
#8335=EDGE_CURVE('',#6686,#6577,#1569,.T.);
#8336=EDGE_CURVE('',#6571,#6687,#1570,.T.);
#8337=EDGE_CURVE('',#6578,#6687,#1571,.T.);
#8338=EDGE_CURVE('',#6686,#6572,#1572,.T.);
#8339=EDGE_CURVE('',#6688,#6561,#1573,.T.);
#8340=EDGE_CURVE('',#6562,#6689,#1574,.T.);
#8341=EDGE_CURVE('',#6689,#6690,#5688,.T.);
#8342=EDGE_CURVE('',#6690,#6651,#1575,.T.);
#8343=EDGE_CURVE('',#6665,#6691,#1576,.T.);
#8344=EDGE_CURVE('',#6691,#6688,#5689,.T.);
#8345=EDGE_CURVE('',#6565,#6692,#1577,.T.);
#8346=EDGE_CURVE('',#6687,#6692,#5690,.T.);
#8347=EDGE_CURVE('',#6693,#6569,#753,.T.);
#8348=EDGE_CURVE('',#6693,#6690,#1578,.T.);
#8349=EDGE_CURVE('',#6570,#6689,#1579,.T.);
#8350=EDGE_CURVE('',#6692,#6563,#1580,.T.);
#8351=EDGE_CURVE('',#6564,#6694,#1581,.T.);
#8352=EDGE_CURVE('',#6694,#6695,#5691,.T.);
#8353=EDGE_CURVE('',#6695,#6664,#1582,.T.);
#8354=EDGE_CURVE('',#6696,#6693,#1583,.T.);
#8355=EDGE_CURVE('',#6696,#6671,#1584,.T.);
#8356=EDGE_CURVE('',#6696,#6697,#1585,.T.);
#8357=EDGE_CURVE('',#6698,#6697,#1586,.T.);
#8358=EDGE_CURVE('',#6699,#6698,#1587,.T.);
#8359=EDGE_CURVE('',#6573,#6699,#1588,.T.);
#8360=EDGE_CURVE('',#6688,#6568,#1589,.T.);
#8361=EDGE_CURVE('',#6691,#6700,#1590,.T.);
#8362=EDGE_CURVE('',#6700,#6568,#754,.T.);
#8363=EDGE_CURVE('',#6694,#6567,#1591,.T.);
#8364=EDGE_CURVE('',#6695,#6574,#1592,.T.);
#8365=EDGE_CURVE('',#6701,#6699,#1593,.T.);
#8366=EDGE_CURVE('',#6664,#6701,#1594,.T.);
#8367=EDGE_CURVE('',#6697,#6700,#1595,.T.);
#8368=EDGE_CURVE('',#6702,#6665,#1596,.T.);
#8369=EDGE_CURVE('',#6702,#6698,#1597,.T.);
#8370=EDGE_CURVE('',#6701,#6702,#1598,.T.);
#8371=EDGE_CURVE('',#6703,#6606,#1599,.T.);
#8372=EDGE_CURVE('',#6704,#6608,#1600,.T.);
#8373=EDGE_CURVE('',#6703,#6704,#1601,.T.);
#8374=EDGE_CURVE('',#6705,#6612,#1602,.T.);
#8375=EDGE_CURVE('',#6704,#6705,#5692,.T.);
#8376=EDGE_CURVE('',#6706,#6616,#1603,.T.);
#8377=EDGE_CURVE('',#6705,#6706,#1604,.T.);
#8378=EDGE_CURVE('',#6707,#6617,#1605,.T.);
#8379=EDGE_CURVE('',#6706,#6707,#5693,.T.);
#8380=EDGE_CURVE('',#6708,#6613,#1606,.T.);
#8381=EDGE_CURVE('',#6707,#6708,#1607,.T.);
#8382=EDGE_CURVE('',#6709,#6609,#1608,.T.);
#8383=EDGE_CURVE('',#6708,#6709,#5694,.T.);
#8384=EDGE_CURVE('',#6710,#6604,#1609,.T.);
#8385=EDGE_CURVE('',#6710,#6703,#5695,.T.);
#8386=EDGE_CURVE('',#6546,#6710,#1610,.T.);
#8387=EDGE_CURVE('',#6537,#6543,#1611,.T.);
#8388=EDGE_CURVE('',#6709,#6532,#1612,.T.);
#8389=EDGE_CURVE('',#6600,#6602,#1613,.T.);
#8390=EDGE_CURVE('',#6590,#6619,#1614,.T.);
#8391=EDGE_CURVE('',#6711,#6712,#1615,.T.);
#8392=EDGE_CURVE('',#6711,#6713,#1616,.T.);
#8393=EDGE_CURVE('',#6713,#6714,#1617,.T.);
#8394=EDGE_CURVE('',#6714,#6712,#1618,.T.);
#8395=EDGE_CURVE('',#6715,#6716,#1619,.T.);
#8396=EDGE_CURVE('',#6715,#6717,#1620,.T.);
#8397=EDGE_CURVE('',#6717,#6718,#1621,.T.);
#8398=EDGE_CURVE('',#6718,#6716,#1622,.T.);
#8399=EDGE_CURVE('',#6719,#6720,#1623,.T.);
#8400=EDGE_CURVE('',#6719,#6715,#1624,.T.);
#8401=EDGE_CURVE('',#6716,#6714,#1625,.T.);
#8402=EDGE_CURVE('',#6713,#6720,#1626,.T.);
#8403=EDGE_CURVE('',#6717,#6721,#1627,.T.);
#8404=EDGE_CURVE('',#6721,#6719,#1628,.T.);
#8405=EDGE_CURVE('',#6722,#6721,#1629,.T.);
#8406=EDGE_CURVE('',#6720,#6722,#1630,.T.);
#8407=EDGE_CURVE('',#6722,#6711,#1631,.T.);
#8408=EDGE_CURVE('',#6712,#6718,#1632,.T.);
#8409=EDGE_CURVE('',#6598,#6723,#1633,.T.);
#8410=EDGE_CURVE('',#6582,#6723,#1634,.T.);
#8411=EDGE_CURVE('',#6723,#6588,#1635,.T.);
#8412=EDGE_CURVE('',#6724,#6725,#5696,.T.);
#8413=EDGE_CURVE('',#6725,#6724,#5697,.T.);
#8414=EDGE_CURVE('',#6724,#6726,#5698,.T.);
#8415=EDGE_CURVE('',#6726,#6727,#5699,.T.);
#8416=EDGE_CURVE('',#6727,#6728,#5700,.T.);
#8417=EDGE_CURVE('',#6728,#6729,#5701,.T.);
#8418=EDGE_CURVE('',#6729,#6726,#5702,.T.);
#8419=EDGE_CURVE('',#6730,#6731,#5703,.T.);
#8420=EDGE_CURVE('',#6732,#6730,#5704,.T.);
#8421=EDGE_CURVE('',#6733,#6732,#5705,.T.);
#8422=EDGE_CURVE('',#6731,#6733,#5706,.T.);
#8423=EDGE_CURVE('',#6731,#6734,#5707,.T.);
#8424=EDGE_CURVE('',#6735,#6734,#5708,.T.);
#8425=EDGE_CURVE('',#6734,#6735,#5709,.T.);
#8426=EDGE_CURVE('',#6736,#6737,#798,.T.);
#8427=EDGE_CURVE('',#6736,#6738,#799,.T.);
#8428=EDGE_CURVE('',#6738,#6739,#800,.T.);
#8429=EDGE_CURVE('',#6739,#6740,#801,.T.);
#8430=EDGE_CURVE('',#6740,#6741,#802,.T.);
#8431=EDGE_CURVE('',#6737,#6741,#803,.T.);
#8432=EDGE_CURVE('',#6737,#6742,#5710,.T.);
#8433=EDGE_CURVE('',#6742,#6742,#5711,.T.);
#8434=EDGE_CURVE('',#6743,#6743,#5712,.T.);
#8435=EDGE_CURVE('',#6743,#6744,#5713,.T.);
#8436=EDGE_CURVE('',#6744,#6745,#804,.T.);
#8437=EDGE_CURVE('',#6745,#6746,#805,.T.);
#8438=EDGE_CURVE('',#6746,#6747,#806,.T.);
#8439=EDGE_CURVE('',#6747,#6744,#807,.T.);
#8440=EDGE_CURVE('',#6748,#6748,#5714,.T.);
#8441=EDGE_CURVE('',#6748,#6725,#5715,.T.);
#8442=EDGE_CURVE('',#6735,#6749,#5716,.T.);
#8443=EDGE_CURVE('',#6749,#6749,#5717,.T.);
#8444=EDGE_CURVE('',#6750,#6750,#5718,.T.);
#8445=EDGE_CURVE('',#6750,#6751,#1636,.T.);
#8446=EDGE_CURVE('',#6751,#6751,#5719,.T.);
#8447=EDGE_CURVE('',#6752,#6753,#5720,.T.);
#8448=EDGE_CURVE('',#6753,#6752,#5721,.T.);
#8449=EDGE_CURVE('',#6753,#6754,#1637,.T.);
#8450=EDGE_CURVE('',#6754,#6754,#5722,.T.);
#8451=EDGE_CURVE('',#6755,#6756,#5723,.T.);
#8452=EDGE_CURVE('',#6756,#6755,#5724,.T.);
#8453=EDGE_CURVE('',#6755,#6752,#1638,.T.);
#8454=EDGE_CURVE('',#6757,#6758,#5725,.T.);
#8455=EDGE_CURVE('',#6758,#6759,#1639,.T.);
#8456=EDGE_CURVE('',#6759,#6760,#5726,.T.);
#8457=EDGE_CURVE('',#6761,#6760,#1640,.T.);
#8458=EDGE_CURVE('',#6761,#6762,#5727,.T.);
#8459=EDGE_CURVE('',#6762,#6763,#808,.T.);
#8460=EDGE_CURVE('',#6763,#6764,#1641,.T.);
#8461=EDGE_CURVE('',#6764,#6765,#809,.T.);
#8462=EDGE_CURVE('',#6765,#6766,#5728,.T.);
#8463=EDGE_CURVE('',#6767,#6766,#1642,.T.);
#8464=EDGE_CURVE('',#6767,#6768,#5729,.T.);
#8465=EDGE_CURVE('',#6768,#6769,#1643,.T.);
#8466=EDGE_CURVE('',#6769,#6759,#5730,.T.);
#8467=EDGE_CURVE('',#6758,#6757,#5731,.T.);
#8468=EDGE_CURVE('',#6770,#6770,#5732,.T.);
#8469=EDGE_CURVE('',#6770,#6771,#1644,.T.);
#8470=EDGE_CURVE('',#6771,#6772,#5733,.T.);
#8471=EDGE_CURVE('',#6772,#6773,#1645,.T.);
#8472=EDGE_CURVE('',#6773,#6774,#810,.T.);
#8473=EDGE_CURVE('',#6774,#6775,#1646,.T.);
#8474=EDGE_CURVE('',#6775,#6776,#5734,.T.);
#8475=EDGE_CURVE('',#6776,#6777,#811,.T.);
#8476=EDGE_CURVE('',#6777,#6778,#812,.T.);
#8477=EDGE_CURVE('',#6778,#6779,#1647,.T.);
#8478=EDGE_CURVE('',#6780,#6779,#5735,.T.);
#8479=EDGE_CURVE('',#6780,#6781,#813,.T.);
#8480=EDGE_CURVE('',#6782,#6781,#1648,.T.);
#8481=EDGE_CURVE('',#6782,#6771,#5736,.T.);
#8482=EDGE_CURVE('',#6741,#6736,#814,.T.);
#8483=EDGE_CURVE('',#6783,#6783,#5737,.T.);
#8484=EDGE_CURVE('',#6783,#6756,#5738,.T.);
#8485=EDGE_CURVE('',#6784,#6785,#5739,.T.);
#8486=EDGE_CURVE('',#6784,#6786,#815,.T.);
#8487=EDGE_CURVE('',#6787,#6786,#5740,.T.);
#8488=EDGE_CURVE('',#6787,#6785,#816,.T.);
#8489=EDGE_CURVE('',#6788,#6789,#5741,.T.);
#8490=EDGE_CURVE('',#6790,#6788,#817,.T.);
#8491=EDGE_CURVE('',#6791,#6790,#5742,.T.);
#8492=EDGE_CURVE('',#6789,#6791,#818,.T.);
#8493=EDGE_CURVE('',#6792,#6793,#5743,.T.);
#8494=EDGE_CURVE('',#6793,#6794,#1649,.T.);
#8495=EDGE_CURVE('',#6794,#6795,#5744,.T.);
#8496=EDGE_CURVE('',#6795,#6792,#1650,.T.);
#8497=EDGE_CURVE('',#6778,#6796,#5745,.T.);
#8498=EDGE_CURVE('',#6796,#6797,#819,.T.);
#8499=EDGE_CURVE('',#6797,#6798,#820,.T.);
#8500=EDGE_CURVE('',#6798,#6799,#5746,.T.);
#8501=EDGE_CURVE('',#6799,#6800,#821,.T.);
#8502=EDGE_CURVE('',#6800,#6801,#755,.T.);
#8503=EDGE_CURVE('',#6801,#6802,#1651,.T.);
#8504=EDGE_CURVE('',#6802,#6803,#822,.T.);
#8505=EDGE_CURVE('',#6803,#6804,#5747,.T.);
#8506=EDGE_CURVE('',#6804,#6805,#1652,.T.);
#8507=EDGE_CURVE('',#6806,#6805,#5748,.T.);
#8508=EDGE_CURVE('',#6806,#6807,#1653,.T.);
#8509=EDGE_CURVE('',#6779,#6807,#5749,.T.);
#8510=EDGE_CURVE('',#6808,#6769,#823,.T.);
#8511=EDGE_CURVE('',#6809,#6808,#5750,.T.);
#8512=EDGE_CURVE('',#6810,#6809,#824,.T.);
#8513=EDGE_CURVE('',#6811,#6810,#5751,.T.);
#8514=EDGE_CURVE('',#6812,#6811,#5752,.T.);
#8515=EDGE_CURVE('',#6760,#6812,#825,.F.);
#8516=EDGE_CURVE('',#6813,#6814,#5753,.T.);
#8517=EDGE_CURVE('',#6815,#6813,#5754,.T.);
#8518=EDGE_CURVE('',#6816,#6815,#5755,.T.);
#8519=EDGE_CURVE('',#6816,#6814,#5756,.T.);
#8520=EDGE_CURVE('',#6770,#6817,#5757,.T.);
#8521=EDGE_CURVE('',#6817,#6817,#5758,.T.);
#8522=EDGE_CURVE('',#6818,#6818,#5759,.T.);
#8523=EDGE_CURVE('',#6818,#6819,#1654,.T.);
#8524=EDGE_CURVE('',#6819,#6819,#5760,.T.);
#8525=EDGE_CURVE('',#6820,#6807,#5761,.T.);
#8526=EDGE_CURVE('',#6821,#6806,#5762,.T.);
#8527=EDGE_CURVE('',#6821,#6822,#1655,.T.);
#8528=EDGE_CURVE('',#6822,#6823,#826,.T.);
#8529=EDGE_CURVE('',#6823,#6824,#5763,.T.);
#8530=EDGE_CURVE('',#6824,#6809,#1656,.T.);
#8531=EDGE_CURVE('',#6825,#6808,#1657,.T.);
#8532=EDGE_CURVE('',#6825,#6826,#5764,.T.);
#8533=EDGE_CURVE('',#6820,#6826,#1658,.T.);
#8534=EDGE_CURVE('',#6827,#6773,#1659,.T.);
#8535=EDGE_CURVE('',#6828,#6827,#5765,.T.);
#8536=EDGE_CURVE('',#6829,#6828,#5766,.T.);
#8537=EDGE_CURVE('',#6774,#6829,#1660,.T.);
#8538=EDGE_CURVE('',#6761,#6830,#5767,.T.);
#8539=EDGE_CURVE('',#6831,#6812,#5768,.T.);
#8540=EDGE_CURVE('',#6830,#6831,#1661,.T.);
#8541=EDGE_CURVE('',#6832,#6833,#5769,.T.);
#8542=EDGE_CURVE('',#6832,#6834,#827,.T.);
#8543=EDGE_CURVE('',#6795,#6834,#828,.F.);
#8544=EDGE_CURVE('',#6833,#6794,#5770,.T.);
#8545=EDGE_CURVE('',#6835,#6782,#829,.T.);
#8546=EDGE_CURVE('',#6836,#6835,#5771,.T.);
#8547=EDGE_CURVE('',#6772,#6836,#830,.T.);
#8548=EDGE_CURVE('',#6837,#6838,#5772,.T.);
#8549=EDGE_CURVE('',#6838,#6839,#831,.T.);
#8550=EDGE_CURVE('',#6797,#6839,#832,.T.);
#8551=EDGE_CURVE('',#6840,#6797,#833,.T.);
#8552=EDGE_CURVE('',#6840,#6841,#834,.T.);
#8553=EDGE_CURVE('',#6841,#6842,#5773,.T.);
#8554=EDGE_CURVE('',#6843,#6842,#1662,.T.);
#8555=EDGE_CURVE('',#6843,#6844,#835,.T.);
#8556=EDGE_CURVE('',#6845,#6844,#5774,.T.);
#8557=EDGE_CURVE('',#6846,#6845,#1663,.T.);
#8558=EDGE_CURVE('',#6846,#6847,#5775,.T.);
#8559=EDGE_CURVE('',#6848,#6847,#1664,.T.);
#8560=EDGE_CURVE('',#6849,#6848,#5776,.T.);
#8561=EDGE_CURVE('',#6849,#6850,#1665,.T.);
#8562=EDGE_CURVE('',#6850,#6851,#5777,.T.);
#8563=EDGE_CURVE('',#6851,#6852,#1666,.T.);
#8564=EDGE_CURVE('',#6852,#6853,#836,.T.);
#8565=EDGE_CURVE('',#6837,#6853,#1667,.T.);
#8566=EDGE_CURVE('',#6854,#6852,#1668,.T.);
#8567=EDGE_CURVE('',#6855,#6854,#837,.T.);
#8568=EDGE_CURVE('',#6856,#6855,#838,.T.);
#8569=EDGE_CURVE('',#6856,#6857,#756,.T.);
#8570=EDGE_CURVE('',#6857,#6858,#757,.T.);
#8571=EDGE_CURVE('',#6853,#6858,#1669,.T.);
#8572=EDGE_CURVE('',#6859,#6837,#839,.T.);
#8573=EDGE_CURVE('',#6860,#6859,#5778,.T.);
#8574=EDGE_CURVE('',#6860,#6838,#5779,.T.);
#8575=EDGE_CURVE('',#6861,#6862,#5780,.T.);
#8576=EDGE_CURVE('',#6861,#6863,#840,.T.);
#8577=EDGE_CURVE('',#6864,#6863,#5781,.T.);
#8578=EDGE_CURVE('',#6864,#6862,#841,.T.);
#8579=EDGE_CURVE('',#6865,#6866,#5782,.T.);
#8580=EDGE_CURVE('',#6867,#6865,#842,.T.);
#8581=EDGE_CURVE('',#6868,#6867,#5783,.T.);
#8582=EDGE_CURVE('',#6866,#6868,#843,.T.);
#8583=EDGE_CURVE('',#6729,#6730,#71,.T.);
#8584=EDGE_CURVE('',#6727,#6733,#72,.T.);
#8585=EDGE_CURVE('',#6745,#6869,#5784,.T.);
#8586=EDGE_CURVE('',#6870,#6869,#844,.T.);
#8587=EDGE_CURVE('',#6747,#6870,#5785,.T.);
#8588=EDGE_CURVE('',#6740,#6871,#5786,.T.);
#8589=EDGE_CURVE('',#6872,#6871,#845,.T.);
#8590=EDGE_CURVE('',#6738,#6872,#5787,.T.);
#8591=EDGE_CURVE('',#6748,#6742,#1670,.T.);
#8592=EDGE_CURVE('',#6743,#6749,#1671,.T.);
#8593=EDGE_CURVE('',#6869,#6870,#846,.T.);
#8594=EDGE_CURVE('',#6871,#6872,#847,.T.);
#8595=EDGE_CURVE('',#6791,#6863,#1672,.T.);
#8596=EDGE_CURVE('',#6864,#6790,#1673,.T.);
#8597=EDGE_CURVE('',#6824,#6873,#1674,.T.);
#8598=EDGE_CURVE('',#6873,#6874,#1675,.T.);
#8599=EDGE_CURVE('',#6874,#6809,#1676,.T.);
#8600=EDGE_CURVE('',#6790,#6784,#1677,.T.);
#8601=EDGE_CURVE('',#6866,#6784,#1678,.T.);
#8602=EDGE_CURVE('',#6866,#6864,#1679,.T.);
#8603=EDGE_CURVE('',#6865,#6785,#1680,.T.);
#8604=EDGE_CURVE('',#6785,#6791,#1681,.T.);
#8605=EDGE_CURVE('',#6863,#6865,#1682,.T.);
#8606=EDGE_CURVE('',#6875,#6876,#1683,.T.);
#8607=EDGE_CURVE('',#6876,#6877,#1684,.T.);
#8608=EDGE_CURVE('',#6878,#6877,#1685,.T.);
#8609=EDGE_CURVE('',#6878,#6875,#1686,.T.);
#8610=EDGE_CURVE('',#6879,#6880,#1687,.T.);
#8611=EDGE_CURVE('',#6880,#6881,#1688,.T.);
#8612=EDGE_CURVE('',#6882,#6881,#1689,.T.);
#8613=EDGE_CURVE('',#6882,#6879,#1690,.T.);
#8614=EDGE_CURVE('',#6883,#6884,#1691,.T.);
#8615=EDGE_CURVE('',#6884,#6885,#1692,.T.);
#8616=EDGE_CURVE('',#6885,#6886,#1693,.T.);
#8617=EDGE_CURVE('',#6886,#6883,#1694,.T.);
#8618=EDGE_CURVE('',#6829,#6775,#1695,.T.);
#8619=EDGE_CURVE('',#6862,#6868,#1696,.T.);
#8620=EDGE_CURVE('',#6867,#6861,#1697,.T.);
#8621=EDGE_CURVE('',#6887,#6883,#848,.T.);
#8622=EDGE_CURVE('',#6888,#6887,#5788,.T.);
#8623=EDGE_CURVE('',#6878,#6888,#849,.T.);
#8624=EDGE_CURVE('',#6883,#6878,#5789,.T.);
#8625=EDGE_CURVE('',#6889,#6888,#1698,.T.);
#8626=EDGE_CURVE('',#6875,#6889,#850,.T.);
#8627=EDGE_CURVE('',#6890,#6886,#851,.T.);
#8628=EDGE_CURVE('',#6887,#6890,#1699,.T.);
#8629=EDGE_CURVE('',#6786,#6788,#1700,.T.);
#8630=EDGE_CURVE('',#6789,#6787,#1701,.T.);
#8631=EDGE_CURVE('',#6891,#6880,#852,.T.);
#8632=EDGE_CURVE('',#6892,#6880,#5790,.T.);
#8633=EDGE_CURVE('',#6893,#6892,#853,.T.);
#8634=EDGE_CURVE('',#6891,#6893,#5791,.T.);
#8635=EDGE_CURVE('',#6894,#6895,#5792,.T.);
#8636=EDGE_CURVE('',#6896,#6895,#5793,.T.);
#8637=EDGE_CURVE('',#6897,#6896,#5794,.T.);
#8638=EDGE_CURVE('',#6894,#6897,#5795,.T.);
#8639=EDGE_CURVE('',#6895,#6780,#1702,.T.);
#8640=EDGE_CURVE('',#6781,#6894,#1703,.T.);
#8641=EDGE_CURVE('',#6898,#6899,#5796,.T.);
#8642=EDGE_CURVE('',#6899,#6900,#1704,.T.);
#8643=EDGE_CURVE('',#6900,#6901,#1705,.T.);
#8644=EDGE_CURVE('',#6901,#6898,#1706,.T.);
#8645=EDGE_CURVE('',#6902,#6903,#854,.T.);
#8646=EDGE_CURVE('',#6902,#6904,#758,.T.);
#8647=EDGE_CURVE('',#6905,#6904,#5797,.T.);
#8648=EDGE_CURVE('',#6903,#6905,#759,.T.);
#8649=EDGE_CURVE('',#6906,#6904,#1707,.T.);
#8650=EDGE_CURVE('',#6907,#6906,#5798,.T.);
#8651=EDGE_CURVE('',#6905,#6907,#1708,.T.);
#8652=EDGE_CURVE('',#6907,#6799,#855,.T.);
#8653=EDGE_CURVE('',#6800,#6906,#760,.T.);
#8654=EDGE_CURVE('',#6904,#6908,#1709,.T.);
#8655=EDGE_CURVE('',#6801,#6908,#1710,.T.);
#8656=EDGE_CURVE('',#6909,#6902,#1711,.T.);
#8657=EDGE_CURVE('',#6903,#6757,#1712,.T.);
#8658=EDGE_CURVE('',#6910,#6757,#1713,.T.);
#8659=EDGE_CURVE('',#6910,#6815,#1714,.T.);
#8660=EDGE_CURVE('',#6815,#6909,#1715,.T.);
#8661=EDGE_CURVE('',#6772,#6827,#1716,.T.);
#8662=EDGE_CURVE('',#6851,#6911,#856,.T.);
#8663=EDGE_CURVE('',#6912,#6850,#857,.T.);
#8664=EDGE_CURVE('',#6911,#6912,#5799,.T.);
#8665=EDGE_CURVE('',#6847,#6913,#5800,.T.);
#8666=EDGE_CURVE('',#6913,#6914,#1717,.T.);
#8667=EDGE_CURVE('',#6914,#6846,#5801,.T.);
#8668=EDGE_CURVE('',#6848,#6845,#1718,.T.);
#8669=EDGE_CURVE('',#6858,#6837,#1719,.T.);
#8670=EDGE_CURVE('',#6851,#6854,#1720,.T.);
#8671=EDGE_CURVE('',#6842,#6915,#1721,.T.);
#8672=EDGE_CURVE('',#6915,#6843,#1722,.T.);
#8673=EDGE_CURVE('',#6841,#6916,#5802,.T.);
#8674=EDGE_CURVE('',#6917,#6916,#5803,.T.);
#8675=EDGE_CURVE('',#6842,#6917,#858,.T.);
#8676=EDGE_CURVE('',#6918,#6917,#1723,.T.);
#8677=EDGE_CURVE('',#6915,#6918,#5804,.T.);
#8678=EDGE_CURVE('',#6919,#6920,#859,.T.);
#8679=EDGE_CURVE('',#6921,#6919,#860,.T.);
#8680=EDGE_CURVE('',#6915,#6921,#761,.T.);
#8681=EDGE_CURVE('',#6920,#6918,#762,.T.);
#8682=EDGE_CURVE('',#6844,#6921,#1724,.T.);
#8683=EDGE_CURVE('',#6922,#6858,#5805,.T.);
#8684=EDGE_CURVE('',#6859,#6922,#1725,.T.);
#8685=EDGE_CURVE('',#6855,#6923,#861,.T.);
#8686=EDGE_CURVE('',#6922,#6923,#763,.T.);
#8687=EDGE_CURVE('',#6923,#6911,#1726,.T.);
#8688=EDGE_CURVE('',#6839,#6924,#862,.T.);
#8689=EDGE_CURVE('',#6924,#6860,#863,.T.);
#8690=EDGE_CURVE('',#6913,#6914,#5806,.T.);
#8691=EDGE_CURVE('',#6925,#6840,#864,.T.);
#8692=EDGE_CURVE('',#6916,#6925,#865,.T.);
#8693=EDGE_CURVE('',#6907,#6860,#5807,.T.);
#8694=EDGE_CURVE('',#6798,#6924,#5808,.T.);
#8695=EDGE_CURVE('',#6778,#6926,#866,.T.);
#8696=EDGE_CURVE('',#6916,#6926,#5809,.T.);
#8697=EDGE_CURVE('',#6796,#6925,#5810,.T.);
#8698=EDGE_CURVE('',#6775,#6927,#867,.T.);
#8699=EDGE_CURVE('',#6926,#6927,#5811,.T.);
#8700=EDGE_CURVE('',#6776,#6926,#5812,.T.);
#8701=EDGE_CURVE('',#6928,#6836,#1727,.T.);
#8702=EDGE_CURVE('',#6928,#6827,#764,.T.);
#8703=EDGE_CURVE('',#6929,#6762,#5813,.T.);
#8704=EDGE_CURVE('',#6929,#6930,#868,.T.);
#8705=EDGE_CURVE('',#6930,#6763,#5814,.T.);
#8706=EDGE_CURVE('',#6931,#6897,#1728,.T.);
#8707=EDGE_CURVE('',#6897,#6932,#5815,.T.);
#8708=EDGE_CURVE('',#6932,#6933,#1729,.T.);
#8709=EDGE_CURVE('',#6933,#6931,#5816,.T.);
#8710=EDGE_CURVE('',#6934,#6935,#1730,.T.);
#8711=EDGE_CURVE('',#6935,#6936,#1731,.T.);
#8712=EDGE_CURVE('',#6936,#6822,#869,.T.);
#8713=EDGE_CURVE('',#6821,#6934,#1732,.T.);
#8714=EDGE_CURVE('',#6937,#6896,#5817,.T.);
#8715=EDGE_CURVE('',#6932,#6937,#5818,.T.);
#8716=EDGE_CURVE('',#6932,#6935,#5819,.T.);
#8717=EDGE_CURVE('',#6933,#6934,#5820,.T.);
#8718=EDGE_CURVE('',#6938,#6939,#1733,.T.);
#8719=EDGE_CURVE('',#6938,#6794,#5821,.T.);
#8720=EDGE_CURVE('',#6939,#6793,#5822,.T.);
#8721=EDGE_CURVE('',#6894,#6940,#1734,.T.);
#8722=EDGE_CURVE('',#6940,#6931,#5823,.T.);
#8723=EDGE_CURVE('',#6768,#6941,#1735,.T.);
#8724=EDGE_CURVE('',#6941,#6825,#1736,.T.);
#8725=EDGE_CURVE('',#6941,#6767,#1737,.T.);
#8726=EDGE_CURVE('',#6942,#6943,#1738,.T.);
#8727=EDGE_CURVE('',#6943,#6816,#1739,.T.);
#8728=EDGE_CURVE('',#6816,#6944,#1740,.T.);
#8729=EDGE_CURVE('',#6944,#6942,#1741,.T.);
#8730=EDGE_CURVE('',#6945,#6946,#1742,.T.);
#8731=EDGE_CURVE('',#6946,#6947,#1743,.T.);
#8732=EDGE_CURVE('',#6948,#6947,#870,.T.);
#8733=EDGE_CURVE('',#6930,#6948,#1744,.T.);
#8734=EDGE_CURVE('',#6949,#6929,#1745,.T.);
#8735=EDGE_CURVE('',#6949,#6950,#1746,.T.);
#8736=EDGE_CURVE('',#6950,#6945,#1747,.T.);
#8737=EDGE_CURVE('',#6829,#6951,#765,.T.);
#8738=EDGE_CURVE('',#6927,#6951,#1748,.T.);
#8739=EDGE_CURVE('',#6952,#6928,#871,.T.);
#8740=EDGE_CURVE('',#6828,#6952,#766,.T.);
#8741=EDGE_CURVE('',#6951,#6953,#872,.T.);
#8742=EDGE_CURVE('',#6953,#6828,#767,.T.);
#8743=EDGE_CURVE('',#6824,#6954,#873,.T.);
#8744=EDGE_CURVE('',#6955,#6954,#1749,.T.);
#8745=EDGE_CURVE('',#6955,#6873,#874,.T.);
#8746=EDGE_CURVE('',#6956,#6937,#5824,.T.);
#8747=EDGE_CURVE('',#6956,#6935,#5825,.T.);
#8748=EDGE_CURVE('',#6957,#6823,#5826,.T.);
#8749=EDGE_CURVE('',#6954,#6957,#5827,.T.);
#8750=EDGE_CURVE('',#6957,#6936,#875,.T.);
#8751=EDGE_CURVE('',#6957,#6956,#1750,.T.);
#8752=EDGE_CURVE('',#6831,#6958,#5828,.T.);
#8753=EDGE_CURVE('',#6958,#6938,#876,.T.);
#8754=EDGE_CURVE('',#6939,#6830,#5829,.T.);
#8755=EDGE_CURVE('',#6811,#6958,#5830,.T.);
#8756=EDGE_CURVE('',#6833,#6811,#5831,.T.);
#8757=EDGE_CURVE('',#6792,#6949,#5832,.T.);
#8758=EDGE_CURVE('',#6826,#6941,#1751,.T.);
#8759=EDGE_CURVE('',#6810,#6959,#1752,.T.);
#8760=EDGE_CURVE('',#6959,#6960,#5833,.T.);
#8761=EDGE_CURVE('',#6960,#6832,#1753,.T.);
#8762=EDGE_CURVE('',#6961,#6962,#1754,.T.);
#8763=EDGE_CURVE('',#6963,#6962,#5834,.T.);
#8764=EDGE_CURVE('',#6963,#6964,#1755,.T.);
#8765=EDGE_CURVE('',#6964,#6961,#5835,.T.);
#8766=EDGE_CURVE('',#6890,#6889,#5836,.T.);
#8767=EDGE_CURVE('',#6901,#6942,#5837,.T.);
#8768=EDGE_CURVE('',#6944,#6910,#5838,.T.);
#8769=EDGE_CURVE('',#6757,#6805,#1756,.T.);
#8770=EDGE_CURVE('',#6804,#6898,#877,.T.);
#8771=EDGE_CURVE('',#6877,#6884,#5839,.T.);
#8772=EDGE_CURVE('',#6881,#6965,#5840,.T.);
#8773=EDGE_CURVE('',#6966,#6965,#1757,.T.);
#8774=EDGE_CURVE('',#6966,#6882,#5841,.T.);
#8775=EDGE_CURVE('',#6766,#6820,#1758,.T.);
#8776=EDGE_CURVE('',#6967,#6765,#5842,.T.);
#8777=EDGE_CURVE('',#6967,#6968,#1759,.T.);
#8778=EDGE_CURVE('',#6968,#6955,#5843,.T.);
#8779=EDGE_CURVE('',#6969,#6970,#1760,.T.);
#8780=EDGE_CURVE('',#6970,#6971,#5844,.T.);
#8781=EDGE_CURVE('',#6971,#6972,#1761,.T.);
#8782=EDGE_CURVE('',#6972,#6969,#5845,.T.);
#8783=EDGE_CURVE('',#6893,#6973,#1762,.T.);
#8784=EDGE_CURVE('',#6973,#6974,#5846,.T.);
#8785=EDGE_CURVE('',#6974,#6891,#1763,.T.);
#8786=EDGE_CURVE('',#6965,#6892,#1764,.T.);
#8787=EDGE_CURVE('',#6892,#6975,#1765,.T.);
#8788=EDGE_CURVE('',#6975,#6966,#1766,.T.);
#8789=EDGE_CURVE('',#6873,#6946,#5847,.T.);
#8790=EDGE_CURVE('',#6945,#6874,#5848,.T.);
#8791=EDGE_CURVE('',#6885,#6876,#5849,.T.);
#8792=EDGE_CURVE('',#6875,#6886,#5850,.T.);
#8793=EDGE_CURVE('',#6879,#6963,#878,.T.);
#8794=EDGE_CURVE('',#6962,#6975,#879,.T.);
#8795=EDGE_CURVE('',#6964,#6882,#880,.T.);
#8796=EDGE_CURVE('',#6961,#6966,#881,.T.);
#8797=EDGE_CURVE('',#6874,#6959,#882,.T.);
#8798=EDGE_CURVE('',#6945,#6960,#883,.T.);
#8799=EDGE_CURVE('',#6834,#6950,#884,.T.);
#8800=EDGE_CURVE('',#6953,#6952,#1767,.T.);
#8801=EDGE_CURVE('',#6900,#6976,#885,.T.);
#8802=EDGE_CURVE('',#6976,#6943,#886,.T.);
#8803=EDGE_CURVE('',#6908,#6813,#1768,.T.);
#8804=EDGE_CURVE('',#6908,#6909,#768,.T.);
#8805=EDGE_CURVE('',#6803,#6899,#887,.T.);
#8806=EDGE_CURVE('',#6814,#6977,#1769,.T.);
#8807=EDGE_CURVE('',#6977,#6978,#1770,.T.);
#8808=EDGE_CURVE('',#6978,#6802,#5851,.T.);
#8809=EDGE_CURVE('',#6977,#6976,#769,.T.);
#8810=EDGE_CURVE('',#6978,#6899,#5852,.T.);
#8811=EDGE_CURVE('',#6940,#6835,#1771,.T.);
#8812=EDGE_CURVE('',#6912,#6920,#1772,.T.);
#8813=EDGE_CURVE('',#6884,#6972,#888,.T.);
#8814=EDGE_CURVE('',#6885,#6971,#889,.T.);
#8815=EDGE_CURVE('',#6969,#6877,#890,.T.);
#8816=EDGE_CURVE('',#6970,#6876,#891,.T.);
#8817=EDGE_CURVE('',#6973,#6965,#892,.T.);
#8818=EDGE_CURVE('',#6881,#6974,#893,.T.);
#8819=EDGE_CURVE('',#6968,#6946,#894,.T.);
#8820=EDGE_CURVE('',#6947,#6967,#895,.T.);
#8821=EDGE_CURVE('',#6948,#6764,#5853,.T.);
#8822=EDGE_CURVE('',#6979,#6849,#1773,.T.);
#8823=EDGE_CURVE('',#6919,#6979,#1774,.T.);
#8824=EDGE_CURVE('',#6844,#6979,#1775,.T.);
#8825=EDGE_CURVE('',#6980,#6980,#5854,.T.);
#8826=EDGE_CURVE('',#6981,#6982,#5855,.T.);
#8827=EDGE_CURVE('',#6982,#6983,#5856,.T.);
#8828=EDGE_CURVE('',#6983,#6984,#5857,.T.);
#8829=EDGE_CURVE('',#6984,#6985,#5858,.T.);
#8830=EDGE_CURVE('',#6985,#6986,#5859,.T.);
#8831=EDGE_CURVE('',#6986,#6987,#5860,.T.);
#8832=EDGE_CURVE('',#6987,#6988,#5861,.T.);
#8833=EDGE_CURVE('',#6988,#6989,#5862,.T.);
#8834=EDGE_CURVE('',#6989,#6990,#5863,.T.);
#8835=EDGE_CURVE('',#6990,#6991,#5864,.T.);
#8836=EDGE_CURVE('',#6991,#6992,#5865,.T.);
#8837=EDGE_CURVE('',#6992,#6981,#5866,.T.);
#8838=EDGE_CURVE('',#6993,#6994,#5867,.T.);
#8839=EDGE_CURVE('',#6994,#6995,#1776,.T.);
#8840=EDGE_CURVE('',#6995,#6995,#5868,.T.);
#8841=EDGE_CURVE('',#6994,#6993,#5869,.T.);
#8842=EDGE_CURVE('',#6980,#6996,#1777,.T.);
#8843=EDGE_CURVE('',#6996,#6996,#5870,.T.);
#8844=EDGE_CURVE('',#6997,#6997,#5871,.T.);
#8845=EDGE_CURVE('',#6997,#6993,#1778,.T.);
#8846=EDGE_CURVE('',#6998,#6991,#1779,.T.);
#8847=EDGE_CURVE('',#6998,#6999,#1780,.T.);
#8848=EDGE_CURVE('',#6999,#6992,#1781,.T.);
#8849=EDGE_CURVE('',#6999,#7000,#1782,.T.);
#8850=EDGE_CURVE('',#7000,#6981,#1783,.T.);
#8851=EDGE_CURVE('',#7000,#7001,#1784,.T.);
#8852=EDGE_CURVE('',#7001,#6982,#1785,.T.);
#8853=EDGE_CURVE('',#7001,#7002,#1786,.T.);
#8854=EDGE_CURVE('',#7002,#6983,#1787,.T.);
#8855=EDGE_CURVE('',#7002,#7003,#1788,.T.);
#8856=EDGE_CURVE('',#7003,#6984,#1789,.T.);
#8857=EDGE_CURVE('',#7003,#7004,#1790,.T.);
#8858=EDGE_CURVE('',#7004,#6985,#1791,.T.);
#8859=EDGE_CURVE('',#7005,#6990,#1792,.T.);
#8860=EDGE_CURVE('',#7005,#6998,#1793,.T.);
#8861=EDGE_CURVE('',#7006,#6989,#1794,.T.);
#8862=EDGE_CURVE('',#7006,#7005,#1795,.T.);
#8863=EDGE_CURVE('',#7004,#7007,#1796,.T.);
#8864=EDGE_CURVE('',#7007,#6986,#1797,.T.);
#8865=EDGE_CURVE('',#7007,#7008,#1798,.T.);
#8866=EDGE_CURVE('',#7008,#6987,#1799,.T.);
#8867=EDGE_CURVE('',#7009,#6988,#1800,.T.);
#8868=EDGE_CURVE('',#7009,#7006,#1801,.T.);
#8869=EDGE_CURVE('',#7008,#7009,#1802,.T.);
#8870=EDGE_CURVE('',#7010,#7011,#1803,.T.);
#8871=EDGE_CURVE('',#7010,#7012,#5872,.T.);
#8872=EDGE_CURVE('',#7012,#7013,#896,.T.);
#8873=EDGE_CURVE('',#7014,#7013,#1804,.T.);
#8874=EDGE_CURVE('',#7014,#7015,#897,.T.);
#8875=EDGE_CURVE('',#7016,#7015,#5873,.T.);
#8876=EDGE_CURVE('',#7016,#7017,#1805,.T.);
#8877=EDGE_CURVE('',#7017,#7017,#5874,.T.);
#8878=EDGE_CURVE('',#7018,#7016,#5875,.T.);
#8879=EDGE_CURVE('',#7018,#7019,#1806,.T.);
#8880=EDGE_CURVE('',#7011,#7019,#5876,.T.);
#8881=EDGE_CURVE('',#7020,#7021,#1807,.T.);
#8882=EDGE_CURVE('',#7022,#7021,#5877,.T.);
#8883=EDGE_CURVE('',#7023,#7022,#1808,.T.);
#8884=EDGE_CURVE('',#7023,#7010,#5878,.T.);
#8885=EDGE_CURVE('',#7024,#7011,#5879,.T.);
#8886=EDGE_CURVE('',#7025,#7024,#1809,.T.);
#8887=EDGE_CURVE('',#7025,#7020,#5880,.T.);
#8888=EDGE_CURVE('',#7026,#7027,#1810,.T.);
#8889=EDGE_CURVE('',#7026,#7028,#5881,.T.);
#8890=EDGE_CURVE('',#7028,#7029,#898,.T.);
#8891=EDGE_CURVE('',#7030,#7029,#1811,.T.);
#8892=EDGE_CURVE('',#7030,#7031,#899,.T.);
#8893=EDGE_CURVE('',#7032,#7031,#5882,.T.);
#8894=EDGE_CURVE('',#7032,#7033,#1812,.T.);
#8895=EDGE_CURVE('',#7033,#7034,#5883,.T.);
#8896=EDGE_CURVE('',#7034,#7035,#900,.T.);
#8897=EDGE_CURVE('',#7035,#7036,#1813,.T.);
#8898=EDGE_CURVE('',#7036,#7037,#901,.T.);
#8899=EDGE_CURVE('',#7021,#7037,#5884,.T.);
#8900=EDGE_CURVE('',#7020,#7038,#5885,.T.);
#8901=EDGE_CURVE('',#7038,#7039,#1814,.T.);
#8902=EDGE_CURVE('',#7039,#7033,#5886,.T.);
#8903=EDGE_CURVE('',#7040,#7032,#5887,.T.);
#8904=EDGE_CURVE('',#7040,#7041,#1815,.T.);
#8905=EDGE_CURVE('',#7027,#7041,#5888,.T.);
#8906=EDGE_CURVE('',#7042,#7042,#5889,.T.);
#8907=EDGE_CURVE('',#7042,#7043,#1816,.T.);
#8908=EDGE_CURVE('',#7043,#7044,#5890,.T.);
#8909=EDGE_CURVE('',#7044,#7045,#902,.T.);
#8910=EDGE_CURVE('',#7045,#7046,#1817,.T.);
#8911=EDGE_CURVE('',#7046,#7047,#903,.T.);
#8912=EDGE_CURVE('',#7048,#7047,#5891,.T.);
#8913=EDGE_CURVE('',#7049,#7048,#1818,.T.);
#8914=EDGE_CURVE('',#7049,#7050,#5892,.T.);
#8915=EDGE_CURVE('',#7050,#7051,#1819,.T.);
#8916=EDGE_CURVE('',#7051,#7043,#5893,.T.);
#8917=EDGE_CURVE('',#7052,#7053,#1820,.T.);
#8918=EDGE_CURVE('',#7052,#7054,#5894,.T.);
#8919=EDGE_CURVE('',#7054,#7055,#904,.T.);
#8920=EDGE_CURVE('',#7056,#7055,#1821,.T.);
#8921=EDGE_CURVE('',#7056,#7057,#905,.T.);
#8922=EDGE_CURVE('',#7058,#7057,#5895,.T.);
#8923=EDGE_CURVE('',#7059,#7058,#1822,.T.);
#8924=EDGE_CURVE('',#7059,#7060,#5896,.T.);
#8925=EDGE_CURVE('',#7060,#7061,#906,.T.);
#8926=EDGE_CURVE('',#7061,#7062,#1823,.T.);
#8927=EDGE_CURVE('',#7062,#7063,#907,.T.);
#8928=EDGE_CURVE('',#7053,#7063,#5897,.T.);
#8929=EDGE_CURVE('',#7064,#7065,#1824,.T.);
#8930=EDGE_CURVE('',#7064,#7066,#5898,.T.);
#8931=EDGE_CURVE('',#7066,#7067,#908,.T.);
#8932=EDGE_CURVE('',#7068,#7067,#1825,.T.);
#8933=EDGE_CURVE('',#7068,#7069,#909,.T.);
#8934=EDGE_CURVE('',#7070,#7069,#5899,.T.);
#8935=EDGE_CURVE('',#7071,#7070,#1826,.T.);
#8936=EDGE_CURVE('',#7071,#7072,#5900,.T.);
#8937=EDGE_CURVE('',#7072,#7073,#910,.T.);
#8938=EDGE_CURVE('',#7073,#7074,#1827,.T.);
#8939=EDGE_CURVE('',#7074,#7075,#911,.T.);
#8940=EDGE_CURVE('',#7065,#7075,#5901,.T.);
#8941=EDGE_CURVE('',#7076,#7076,#5902,.T.);
#8942=EDGE_CURVE('',#7076,#7077,#1828,.T.);
#8943=EDGE_CURVE('',#7077,#7077,#5903,.T.);
#8944=EDGE_CURVE('',#7078,#7078,#5904,.T.);
#8945=EDGE_CURVE('',#7078,#7079,#1829,.T.);
#8946=EDGE_CURVE('',#7079,#7079,#5905,.T.);
#8947=EDGE_CURVE('',#7080,#7080,#5906,.T.);
#8948=EDGE_CURVE('',#7080,#7081,#1830,.T.);
#8949=EDGE_CURVE('',#7081,#7081,#5907,.T.);
#8950=EDGE_CURVE('',#7082,#7083,#5908,.T.);
#8951=EDGE_CURVE('',#7083,#7084,#1831,.T.);
#8952=EDGE_CURVE('',#7085,#7084,#5909,.T.);
#8953=EDGE_CURVE('',#7082,#7085,#1832,.T.);
#8954=EDGE_CURVE('',#7050,#7086,#5910,.T.);
#8955=EDGE_CURVE('',#7086,#7087,#1833,.T.);
#8956=EDGE_CURVE('',#7087,#7051,#5911,.T.);
#8957=EDGE_CURVE('',#7088,#7040,#5912,.T.);
#8958=EDGE_CURVE('',#7088,#7089,#1834,.T.);
#8959=EDGE_CURVE('',#7041,#7089,#5913,.T.);
#8960=EDGE_CURVE('',#7090,#7065,#5914,.T.);
#8961=EDGE_CURVE('',#7090,#7091,#1835,.T.);
#8962=EDGE_CURVE('',#7092,#7091,#5915,.T.);
#8963=EDGE_CURVE('',#7093,#7092,#1836,.T.);
#8964=EDGE_CURVE('',#7093,#7094,#5916,.T.);
#8965=EDGE_CURVE('',#7094,#7095,#1837,.T.);
#8966=EDGE_CURVE('',#7095,#7064,#5917,.T.);
#8967=EDGE_CURVE('',#7038,#7096,#5918,.T.);
#8968=EDGE_CURVE('',#7096,#7097,#1838,.T.);
#8969=EDGE_CURVE('',#7097,#7039,#5919,.T.);
#8970=EDGE_CURVE('',#7098,#7018,#5920,.T.);
#8971=EDGE_CURVE('',#7098,#7099,#1839,.T.);
#8972=EDGE_CURVE('',#7019,#7099,#5921,.T.);
#8973=EDGE_CURVE('',#7100,#7053,#5922,.T.);
#8974=EDGE_CURVE('',#7100,#7101,#1840,.T.);
#8975=EDGE_CURVE('',#7102,#7101,#5923,.T.);
#8976=EDGE_CURVE('',#7103,#7102,#1841,.T.);
#8977=EDGE_CURVE('',#7103,#7104,#5924,.T.);
#8978=EDGE_CURVE('',#7104,#7105,#1842,.T.);
#8979=EDGE_CURVE('',#7105,#7052,#5925,.T.);
#8980=EDGE_CURVE('',#7106,#7023,#5926,.T.);
#8981=EDGE_CURVE('',#7107,#7022,#5927,.T.);
#8982=EDGE_CURVE('',#7106,#7107,#1843,.T.);
#8983=EDGE_CURVE('',#7108,#7108,#5928,.T.);
#8984=EDGE_CURVE('',#7108,#7109,#1844,.T.);
#8985=EDGE_CURVE('',#7109,#7109,#5929,.T.);
#8986=EDGE_CURVE('',#7084,#7048,#5930,.T.);
#8987=EDGE_CURVE('',#7083,#7026,#5931,.T.);
#8988=EDGE_CURVE('',#7110,#7027,#5932,.T.);
#8989=EDGE_CURVE('',#7111,#7110,#1845,.T.);
#8990=EDGE_CURVE('',#7111,#7049,#5933,.T.);
#8991=EDGE_CURVE('',#7061,#7036,#1846,.T.);
#8992=EDGE_CURVE('',#7035,#7062,#1847,.T.);
#8993=EDGE_CURVE('',#7055,#7014,#1848,.T.);
#8994=EDGE_CURVE('',#7013,#7056,#1849,.T.);
#8995=EDGE_CURVE('',#7112,#7113,#5934,.T.);
#8996=EDGE_CURVE('',#7114,#7112,#1850,.T.);
#8997=EDGE_CURVE('',#7115,#7114,#5935,.T.);
#8998=EDGE_CURVE('',#7113,#7115,#1851,.T.);
#8999=EDGE_CURVE('',#7037,#7060,#1852,.T.);
#9000=EDGE_CURVE('',#7114,#7059,#1853,.T.);
#9001=EDGE_CURVE('',#7112,#7107,#1854,.T.);
#9002=EDGE_CURVE('',#7116,#7113,#1855,.T.);
#9003=EDGE_CURVE('',#7116,#7117,#5936,.T.);
#9004=EDGE_CURVE('',#7117,#7106,#1856,.T.);
#9005=EDGE_CURVE('',#7015,#7054,#1857,.T.);
#9006=EDGE_CURVE('',#7118,#7105,#1858,.T.);
#9007=EDGE_CURVE('',#7118,#7119,#1859,.T.);
#9008=EDGE_CURVE('',#7119,#7098,#1860,.T.);
#9009=EDGE_CURVE('',#7120,#7116,#1861,.T.);
#9010=EDGE_CURVE('',#7121,#7120,#5937,.T.);
#9011=EDGE_CURVE('',#7117,#7121,#1862,.T.);
#9012=EDGE_CURVE('',#7057,#7012,#1863,.T.);
#9013=EDGE_CURVE('',#7063,#7034,#1864,.T.);
#9014=EDGE_CURVE('',#7122,#7097,#1865,.T.);
#9015=EDGE_CURVE('',#7122,#7123,#1866,.T.);
#9016=EDGE_CURVE('',#7123,#7100,#1867,.T.);
#9017=EDGE_CURVE('',#7121,#7058,#1868,.T.);
#9018=EDGE_CURVE('',#7115,#7120,#1869,.T.);
#9019=EDGE_CURVE('',#7102,#7025,#1870,.T.);
#9020=EDGE_CURVE('',#7024,#7103,#1871,.T.);
#9021=EDGE_CURVE('',#7124,#7122,#5938,.T.);
#9022=EDGE_CURVE('',#7125,#7124,#1872,.T.);
#9023=EDGE_CURVE('',#7123,#7125,#5939,.T.);
#9024=EDGE_CURVE('',#7126,#7124,#1873,.T.);
#9025=EDGE_CURVE('',#7126,#7127,#1874,.T.);
#9026=EDGE_CURVE('',#7125,#7127,#1875,.T.);
#9027=EDGE_CURVE('',#7127,#7118,#5940,.T.);
#9028=EDGE_CURVE('',#7104,#7128,#1876,.T.);
#9029=EDGE_CURVE('',#7128,#7129,#1877,.T.);
#9030=EDGE_CURVE('',#7101,#7129,#1878,.T.);
#9031=EDGE_CURVE('',#7130,#7128,#1879,.T.);
#9032=EDGE_CURVE('',#7131,#7130,#1880,.T.);
#9033=EDGE_CURVE('',#7129,#7131,#1881,.T.);
#9034=EDGE_CURVE('',#7099,#7130,#1882,.T.);
#9035=EDGE_CURVE('',#7119,#7126,#5941,.T.);
#9036=EDGE_CURVE('',#7096,#7131,#1883,.T.);
#9037=EDGE_CURVE('',#7092,#7111,#1884,.T.);
#9038=EDGE_CURVE('',#7110,#7093,#1885,.T.);
#9039=EDGE_CURVE('',#7132,#7133,#5942,.T.);
#9040=EDGE_CURVE('',#7134,#7132,#1886,.T.);
#9041=EDGE_CURVE('',#7135,#7134,#5943,.T.);
#9042=EDGE_CURVE('',#7133,#7135,#1887,.T.);
#9043=EDGE_CURVE('',#7136,#7132,#1888,.T.);
#9044=EDGE_CURVE('',#7136,#7137,#1889,.T.);
#9045=EDGE_CURVE('',#7134,#7137,#1890,.T.);
#9046=EDGE_CURVE('',#7137,#7138,#5944,.T.);
#9047=EDGE_CURVE('',#7138,#7095,#1891,.T.);
#9048=EDGE_CURVE('',#7094,#7139,#1892,.T.);
#9049=EDGE_CURVE('',#7139,#7140,#1893,.T.);
#9050=EDGE_CURVE('',#7091,#7140,#1894,.T.);
#9051=EDGE_CURVE('',#7135,#7090,#1895,.T.);
#9052=EDGE_CURVE('',#7141,#7139,#1896,.T.);
#9053=EDGE_CURVE('',#7142,#7141,#1897,.T.);
#9054=EDGE_CURVE('',#7140,#7142,#1898,.T.);
#9055=EDGE_CURVE('',#7089,#7141,#1899,.T.);
#9056=EDGE_CURVE('',#7143,#7088,#1900,.T.);
#9057=EDGE_CURVE('',#7143,#7136,#5945,.T.);
#9058=EDGE_CURVE('',#7133,#7087,#1901,.T.);
#9059=EDGE_CURVE('',#7086,#7142,#1902,.T.);
#9060=EDGE_CURVE('',#7138,#7143,#1903,.T.);
#9061=EDGE_CURVE('',#7031,#7066,#1904,.T.);
#9062=EDGE_CURVE('',#7075,#7044,#1905,.T.);
#9063=EDGE_CURVE('',#7073,#7046,#1906,.T.);
#9064=EDGE_CURVE('',#7045,#7074,#1907,.T.);
#9065=EDGE_CURVE('',#7067,#7030,#1908,.T.);
#9066=EDGE_CURVE('',#7029,#7068,#1909,.T.);
#9067=EDGE_CURVE('',#7144,#7145,#5946,.T.);
#9068=EDGE_CURVE('',#7146,#7144,#1910,.T.);
#9069=EDGE_CURVE('',#7147,#7146,#5947,.T.);
#9070=EDGE_CURVE('',#7145,#7147,#1911,.T.);
#9071=EDGE_CURVE('',#7047,#7072,#1912,.T.);
#9072=EDGE_CURVE('',#7146,#7071,#1913,.T.);
#9073=EDGE_CURVE('',#7144,#7085,#1914,.T.);
#9074=EDGE_CURVE('',#7148,#7145,#1915,.T.);
#9075=EDGE_CURVE('',#7148,#7149,#5948,.T.);
#9076=EDGE_CURVE('',#7149,#7082,#1916,.T.);
#9077=EDGE_CURVE('',#7150,#7148,#1917,.T.);
#9078=EDGE_CURVE('',#7151,#7150,#5949,.T.);
#9079=EDGE_CURVE('',#7149,#7151,#1918,.T.);
#9080=EDGE_CURVE('',#7069,#7028,#1919,.T.);
#9081=EDGE_CURVE('',#7151,#7070,#1920,.T.);
#9082=EDGE_CURVE('',#7147,#7150,#1921,.T.);
#9083=EDGE_CURVE('',#7152,#7153,#1922,.T.);
#9084=EDGE_CURVE('',#7154,#7153,#1923,.T.);
#9085=EDGE_CURVE('',#7155,#7154,#1924,.T.);
#9086=EDGE_CURVE('',#7155,#7152,#1925,.T.);
#9087=EDGE_CURVE('',#7153,#7156,#1926,.T.);
#9088=EDGE_CURVE('',#7157,#7156,#1927,.T.);
#9089=EDGE_CURVE('',#7154,#7157,#1928,.T.);
#9090=EDGE_CURVE('',#7158,#7159,#1929,.T.);
#9091=EDGE_CURVE('',#7159,#7160,#1930,.T.);
#9092=EDGE_CURVE('',#7161,#7160,#1931,.T.);
#9093=EDGE_CURVE('',#7161,#7158,#1932,.T.);
#9094=EDGE_CURVE('',#7162,#7161,#5950,.T.);
#9095=EDGE_CURVE('',#7163,#7162,#1933,.T.);
#9096=EDGE_CURVE('',#7158,#7163,#5951,.T.);
#9097=EDGE_CURVE('',#7164,#7162,#1934,.T.);
#9098=EDGE_CURVE('',#7164,#7165,#1935,.T.);
#9099=EDGE_CURVE('',#7165,#7163,#1936,.T.);
#9100=EDGE_CURVE('',#7166,#7164,#5952,.T.);
#9101=EDGE_CURVE('',#7167,#7166,#1937,.T.);
#9102=EDGE_CURVE('',#7165,#7167,#5953,.T.);
#9103=EDGE_CURVE('',#7168,#7167,#1938,.T.);
#9104=EDGE_CURVE('',#7169,#7166,#1939,.T.);
#9105=EDGE_CURVE('',#7169,#7168,#1940,.T.);
#9106=EDGE_CURVE('',#7160,#7170,#5954,.T.);
#9107=EDGE_CURVE('',#7170,#7171,#1941,.T.);
#9108=EDGE_CURVE('',#7171,#7169,#5955,.T.);
#9109=EDGE_CURVE('',#7172,#7171,#1942,.T.);
#9110=EDGE_CURVE('',#7168,#7172,#5956,.T.);
#9111=EDGE_CURVE('',#7173,#7172,#1943,.T.);
#9112=EDGE_CURVE('',#7173,#7159,#5957,.T.);
#9113=EDGE_CURVE('',#7156,#7174,#1944,.T.);
#9114=EDGE_CURVE('',#7174,#7152,#1945,.T.);
#9115=EDGE_CURVE('',#7170,#7173,#1946,.T.);
#9116=EDGE_CURVE('',#7175,#7174,#1947,.T.);
#9117=EDGE_CURVE('',#7157,#7175,#1948,.T.);
#9118=EDGE_CURVE('',#7175,#7155,#1949,.T.);
#9119=EDGE_CURVE('',#7176,#7177,#912,.F.);
#9120=EDGE_CURVE('',#7176,#7178,#1950,.T.);
#9121=EDGE_CURVE('',#7178,#7178,#5958,.T.);
#9122=EDGE_CURVE('',#7179,#7176,#913,.F.);
#9123=EDGE_CURVE('',#7180,#7179,#1951,.T.);
#9124=EDGE_CURVE('',#7180,#7180,#5959,.T.);
#9125=EDGE_CURVE('',#7177,#7179,#914,.F.);
#9126=EDGE_CURVE('',#7181,#7182,#915,.T.);
#9127=EDGE_CURVE('',#7182,#7181,#916,.T.);
#9128=EDGE_CURVE('',#7183,#7184,#5960,.T.);
#9129=EDGE_CURVE('',#7185,#7183,#1952,.T.);
#9130=EDGE_CURVE('',#7186,#7185,#5961,.T.);
#9131=EDGE_CURVE('',#7184,#7186,#1953,.T.);
#9132=EDGE_CURVE('',#7187,#7188,#5962,.T.);
#9133=EDGE_CURVE('',#7189,#7187,#1954,.T.);
#9134=EDGE_CURVE('',#7189,#7190,#5963,.T.);
#9135=EDGE_CURVE('',#7190,#7188,#1955,.T.);
#9136=EDGE_CURVE('',#7191,#7177,#1956,.T.);
#9137=EDGE_CURVE('',#7191,#7191,#5964,.T.);
#9138=EDGE_CURVE('',#7192,#7192,#5965,.T.);
#9139=EDGE_CURVE('',#7192,#7193,#1957,.T.);
#9140=EDGE_CURVE('',#7193,#7193,#5966,.T.);
#9141=EDGE_CURVE('',#7194,#7194,#5967,.T.);
#9142=EDGE_CURVE('',#7194,#7182,#1958,.T.);
#9143=EDGE_CURVE('',#7195,#7195,#5968,.T.);
#9144=EDGE_CURVE('',#7195,#7196,#1959,.T.);
#9145=EDGE_CURVE('',#7196,#7196,#5969,.T.);
#9146=EDGE_CURVE('',#7197,#7197,#5970,.T.);
#9147=EDGE_CURVE('',#7197,#7198,#1960,.T.);
#9148=EDGE_CURVE('',#7198,#7198,#5971,.T.);
#9149=EDGE_CURVE('',#7199,#7199,#5972,.T.);
#9150=EDGE_CURVE('',#7199,#7200,#1961,.T.);
#9151=EDGE_CURVE('',#7200,#7200,#5973,.T.);
#9152=EDGE_CURVE('',#7201,#7201,#5974,.T.);
#9153=EDGE_CURVE('',#7201,#7202,#1962,.T.);
#9154=EDGE_CURVE('',#7202,#7202,#5975,.T.);
#9155=EDGE_CURVE('',#7203,#7204,#5976,.T.);
#9156=EDGE_CURVE('',#7205,#7204,#1963,.T.);
#9157=EDGE_CURVE('',#7206,#7205,#5977,.T.);
#9158=EDGE_CURVE('',#7206,#7203,#1964,.T.);
#9159=EDGE_CURVE('',#7207,#7207,#5978,.T.);
#9160=EDGE_CURVE('',#7207,#7208,#1965,.T.);
#9161=EDGE_CURVE('',#7208,#7208,#5979,.T.);
#9162=EDGE_CURVE('',#7209,#7209,#5980,.T.);
#9163=EDGE_CURVE('',#7209,#7210,#1966,.T.);
#9164=EDGE_CURVE('',#7210,#7210,#5981,.T.);
#9165=EDGE_CURVE('',#7207,#7211,#1967,.T.);
#9166=EDGE_CURVE('',#7211,#7211,#5982,.T.);
#9167=EDGE_CURVE('',#7212,#7212,#5983,.T.);
#9168=EDGE_CURVE('',#7212,#7213,#1968,.T.);
#9169=EDGE_CURVE('',#7213,#7213,#5984,.T.);
#9170=EDGE_CURVE('',#7214,#7203,#1969,.T.);
#9171=EDGE_CURVE('',#7215,#7206,#1970,.T.);
#9172=EDGE_CURVE('',#7215,#7214,#1971,.T.);
#9173=EDGE_CURVE('',#7216,#7217,#1972,.T.);
#9174=EDGE_CURVE('',#7218,#7216,#1973,.T.);
#9175=EDGE_CURVE('',#7218,#7219,#1974,.T.);
#9176=EDGE_CURVE('',#7219,#7217,#1975,.T.);
#9177=EDGE_CURVE('',#7217,#7220,#1976,.T.);
#9178=EDGE_CURVE('',#7219,#7221,#1977,.T.);
#9179=EDGE_CURVE('',#7221,#7220,#1978,.T.);
#9180=EDGE_CURVE('',#7220,#7222,#1979,.T.);
#9181=EDGE_CURVE('',#7221,#7223,#1980,.T.);
#9182=EDGE_CURVE('',#7223,#7224,#1981,.T.);
#9183=EDGE_CURVE('',#7224,#7222,#1982,.T.);
#9184=EDGE_CURVE('',#7204,#7225,#1983,.T.);
#9185=EDGE_CURVE('',#7226,#7225,#1984,.T.);
#9186=EDGE_CURVE('',#7205,#7226,#1985,.T.);
#9187=EDGE_CURVE('',#7188,#7227,#1986,.T.);
#9188=EDGE_CURVE('',#7190,#7228,#1987,.T.);
#9189=EDGE_CURVE('',#7228,#7227,#1988,.T.);
#9190=EDGE_CURVE('',#7227,#7229,#5985,.T.);
#9191=EDGE_CURVE('',#7228,#7230,#5986,.T.);
#9192=EDGE_CURVE('',#7230,#7229,#1989,.T.);
#9193=EDGE_CURVE('',#7229,#7231,#1990,.T.);
#9194=EDGE_CURVE('',#7230,#7232,#1991,.T.);
#9195=EDGE_CURVE('',#7232,#7231,#1992,.T.);
#9196=EDGE_CURVE('',#7231,#7233,#5987,.T.);
#9197=EDGE_CURVE('',#7232,#7234,#5988,.T.);
#9198=EDGE_CURVE('',#7234,#7233,#1993,.T.);
#9199=EDGE_CURVE('',#7233,#7235,#1994,.T.);
#9200=EDGE_CURVE('',#7234,#7236,#1995,.T.);
#9201=EDGE_CURVE('',#7236,#7235,#1996,.T.);
#9202=EDGE_CURVE('',#7237,#7238,#1997,.T.);
#9203=EDGE_CURVE('',#7235,#7237,#5989,.T.);
#9204=EDGE_CURVE('',#7236,#7238,#5990,.T.);
#9205=EDGE_CURVE('',#7239,#7240,#5991,.T.);
#9206=EDGE_CURVE('',#7241,#7239,#1998,.T.);
#9207=EDGE_CURVE('',#7242,#7241,#5992,.T.);
#9208=EDGE_CURVE('',#7240,#7242,#1999,.T.);
#9209=EDGE_CURVE('',#7243,#7244,#2000,.T.);
#9210=EDGE_CURVE('',#7245,#7243,#2001,.T.);
#9211=EDGE_CURVE('',#7245,#7246,#2002,.T.);
#9212=EDGE_CURVE('',#7246,#7244,#2003,.T.);
#9213=EDGE_CURVE('',#7238,#7247,#2004,.T.);
#9214=EDGE_CURVE('',#7248,#7189,#2005,.T.);
#9215=EDGE_CURVE('',#7248,#7249,#2006,.T.);
#9216=EDGE_CURVE('',#7247,#7249,#2007,.T.);
#9217=EDGE_CURVE('',#7250,#7187,#2008,.T.);
#9218=EDGE_CURVE('',#7250,#7248,#2009,.T.);
#9219=EDGE_CURVE('',#7249,#7186,#2010,.T.);
#9220=EDGE_CURVE('',#7239,#7185,#2011,.T.);
#9221=EDGE_CURVE('',#7247,#7240,#2012,.T.);
#9222=EDGE_CURVE('',#7184,#7251,#2013,.T.);
#9223=EDGE_CURVE('',#7244,#7250,#2014,.T.);
#9224=EDGE_CURVE('',#7252,#7246,#2015,.T.);
#9225=EDGE_CURVE('',#7253,#7252,#2016,.T.);
#9226=EDGE_CURVE('',#7251,#7253,#2017,.T.);
#9227=EDGE_CURVE('',#7254,#7253,#2018,.T.);
#9228=EDGE_CURVE('',#7255,#7254,#2019,.T.);
#9229=EDGE_CURVE('',#7256,#7255,#2020,.T.);
#9230=EDGE_CURVE('',#7256,#7251,#2021,.T.);
#9231=EDGE_CURVE('',#7254,#7252,#5993,.T.);
#9232=EDGE_CURVE('',#7257,#7258,#2022,.T.);
#9233=EDGE_CURVE('',#7259,#7258,#2023,.T.);
#9234=EDGE_CURVE('',#7260,#7259,#2024,.T.);
#9235=EDGE_CURVE('',#7260,#7257,#2025,.T.);
#9236=EDGE_CURVE('',#7226,#7260,#5994,.T.);
#9237=EDGE_CURVE('',#7259,#7261,#5995,.T.);
#9238=EDGE_CURVE('',#7261,#7262,#2026,.T.);
#9239=EDGE_CURVE('',#7262,#7215,#5996,.T.);
#9240=EDGE_CURVE('',#7263,#7223,#5997,.T.);
#9241=EDGE_CURVE('',#7223,#7214,#5998,.T.);
#9242=EDGE_CURVE('',#7262,#7263,#2027,.T.);
#9243=EDGE_CURVE('',#7264,#7263,#2028,.T.);
#9244=EDGE_CURVE('',#7224,#7264,#2029,.T.);
#9245=EDGE_CURVE('',#7265,#7237,#2030,.T.);
#9246=EDGE_CURVE('',#7265,#7216,#2031,.T.);
#9247=EDGE_CURVE('',#7222,#7266,#2032,.T.);
#9248=EDGE_CURVE('',#7266,#7243,#2033,.T.);
#9249=EDGE_CURVE('',#7267,#7266,#2034,.T.);
#9250=EDGE_CURVE('',#7267,#7245,#2035,.T.);
#9251=EDGE_CURVE('',#7264,#7267,#2036,.T.);
#9252=EDGE_CURVE('',#7268,#7264,#2037,.T.);
#9253=EDGE_CURVE('',#7258,#7268,#5999,.T.);
#9254=EDGE_CURVE('',#7252,#7257,#6000,.T.);
#9255=EDGE_CURVE('',#7261,#7268,#2038,.T.);
#9256=EDGE_CURVE('',#7241,#7183,#2039,.T.);
#9257=EDGE_CURVE('',#7242,#7256,#2040,.T.);
#9258=EDGE_CURVE('',#7269,#7218,#2041,.T.);
#9259=EDGE_CURVE('',#7225,#7269,#6001,.T.);
#9260=EDGE_CURVE('',#7269,#7265,#2042,.T.);
#9261=EDGE_CURVE('',#7255,#7269,#2043,.T.);
#9262=EDGE_CURVE('',#7269,#7254,#6002,.T.);
#9263=EDGE_CURVE('',#7270,#7271,#917,.F.);
#9264=EDGE_CURVE('',#7272,#7270,#770,.T.);
#9265=EDGE_CURVE('',#7273,#7272,#6003,.T.);
#9266=EDGE_CURVE('',#7274,#7273,#6004,.T.);
#9267=EDGE_CURVE('',#7275,#7274,#6005,.T.);
#9268=EDGE_CURVE('',#7271,#7275,#6006,.T.);
#9269=EDGE_CURVE('',#7276,#7276,#6007,.T.);
#9270=EDGE_CURVE('',#7276,#7277,#2044,.T.);
#9271=EDGE_CURVE('',#7277,#7277,#6008,.T.);
#9272=EDGE_CURVE('',#7278,#7279,#918,.T.);
#9273=EDGE_CURVE('',#7279,#7280,#919,.T.);
#9274=EDGE_CURVE('',#7280,#7281,#920,.T.);
#9275=EDGE_CURVE('',#7281,#7282,#921,.T.);
#9276=EDGE_CURVE('',#7282,#7283,#922,.T.);
#9277=EDGE_CURVE('',#7283,#7284,#2045,.T.);
#9278=EDGE_CURVE('',#7284,#7285,#6009,.T.);
#9279=EDGE_CURVE('',#7285,#7286,#923,.T.);
#9280=EDGE_CURVE('',#7286,#7287,#6010,.T.);
#9281=EDGE_CURVE('',#7287,#7288,#924,.T.);
#9282=EDGE_CURVE('',#7288,#7284,#6011,.T.);
#9283=EDGE_CURVE('',#7283,#7289,#925,.T.);
#9284=EDGE_CURVE('',#7289,#7290,#926,.T.);
#9285=EDGE_CURVE('',#7290,#7278,#927,.T.);
#9286=EDGE_CURVE('',#7291,#7292,#6012,.T.);
#9287=EDGE_CURVE('',#7285,#7291,#928,.T.);
#9288=EDGE_CURVE('',#7292,#7288,#929,.T.);
#9289=EDGE_CURVE('',#7293,#7293,#6013,.T.);
#9290=EDGE_CURVE('',#7293,#7294,#2046,.T.);
#9291=EDGE_CURVE('',#7294,#7295,#6014,.T.);
#9292=EDGE_CURVE('',#7295,#7296,#930,.T.);
#9293=EDGE_CURVE('',#7296,#7297,#6015,.T.);
#9294=EDGE_CURVE('',#7297,#7298,#931,.T.);
#9295=EDGE_CURVE('',#7298,#7299,#6016,.T.);
#9296=EDGE_CURVE('',#7299,#7300,#932,.T.);
#9297=EDGE_CURVE('',#7300,#7294,#6017,.T.);
#9298=EDGE_CURVE('',#7301,#7301,#6018,.T.);
#9299=EDGE_CURVE('',#7301,#7293,#6019,.T.);
#9300=EDGE_CURVE('',#7302,#7303,#6020,.T.);
#9301=EDGE_CURVE('',#7303,#7304,#2047,.T.);
#9302=EDGE_CURVE('',#7304,#7305,#6021,.T.);
#9303=EDGE_CURVE('',#7305,#7306,#933,.T.);
#9304=EDGE_CURVE('',#7306,#7307,#934,.T.);
#9305=EDGE_CURVE('',#7307,#7308,#935,.T.);
#9306=EDGE_CURVE('',#7308,#7309,#6022,.T.);
#9307=EDGE_CURVE('',#7309,#7310,#936,.T.);
#9308=EDGE_CURVE('',#7310,#7311,#937,.T.);
#9309=EDGE_CURVE('',#7311,#7312,#6023,.T.);
#9310=EDGE_CURVE('',#7313,#7312,#2048,.T.);
#9311=EDGE_CURVE('',#7314,#7313,#6024,.T.);
#9312=EDGE_CURVE('',#7314,#7315,#938,.T.);
#9313=EDGE_CURVE('',#7315,#7316,#6025,.T.);
#9314=EDGE_CURVE('',#7316,#7317,#6026,.T.);
#9315=EDGE_CURVE('',#7317,#7318,#939,.T.);
#9316=EDGE_CURVE('',#7318,#7319,#6027,.T.);
#9317=EDGE_CURVE('',#7319,#7320,#940,.T.);
#9318=EDGE_CURVE('',#7320,#7304,#6028,.T.);
#9319=EDGE_CURVE('',#7303,#7321,#6029,.T.);
#9320=EDGE_CURVE('',#7321,#7322,#2049,.T.);
#9321=EDGE_CURVE('',#7322,#7323,#6030,.T.);
#9322=EDGE_CURVE('',#7323,#7324,#941,.T.);
#9323=EDGE_CURVE('',#7324,#7302,#2050,.T.);
#9324=EDGE_CURVE('',#7325,#7326,#771,.T.);
#9325=EDGE_CURVE('',#7326,#7327,#942,.T.);
#9326=EDGE_CURVE('',#7327,#7328,#6031,.T.);
#9327=EDGE_CURVE('',#7328,#7325,#943,.T.);
#9328=EDGE_CURVE('',#7329,#7330,#944,.T.);
#9329=EDGE_CURVE('',#7330,#7329,#945,.T.);
#9330=EDGE_CURVE('',#7331,#7331,#6032,.T.);
#9331=EDGE_CURVE('',#7331,#7277,#6033,.T.);
#9332=EDGE_CURVE('',#7332,#7333,#946,.T.);
#9333=EDGE_CURVE('',#7333,#7334,#947,.T.);
#9334=EDGE_CURVE('',#7334,#7335,#2051,.T.);
#9335=EDGE_CURVE('',#7335,#7336,#6034,.T.);
#9336=EDGE_CURVE('',#7336,#7337,#2052,.T.);
#9337=EDGE_CURVE('',#7337,#7338,#948,.T.);
#9338=EDGE_CURVE('',#7338,#7339,#949,.T.);
#9339=EDGE_CURVE('',#7339,#7332,#950,.T.);
#9340=EDGE_CURVE('',#7340,#7341,#6035,.T.);
#9341=EDGE_CURVE('',#7342,#7340,#6036,.T.);
#9342=EDGE_CURVE('',#7343,#7342,#6037,.T.);
#9343=EDGE_CURVE('',#7341,#7343,#6038,.T.);
#9344=EDGE_CURVE('',#7276,#7344,#6039,.T.);
#9345=EDGE_CURVE('',#7344,#7344,#6040,.T.);
#9346=EDGE_CURVE('',#7330,#7345,#6041,.T.);
#9347=EDGE_CURVE('',#7346,#7345,#6042,.T.);
#9348=EDGE_CURVE('',#7347,#7346,#951,.T.);
#9349=EDGE_CURVE('',#7329,#7347,#6043,.T.);
#9350=EDGE_CURVE('',#7348,#7302,#952,.T.);
#9351=EDGE_CURVE('',#7349,#7348,#6044,.T.);
#9352=EDGE_CURVE('',#7349,#7321,#6045,.T.);
#9353=EDGE_CURVE('',#7350,#7350,#6046,.T.);
#9354=EDGE_CURVE('',#7350,#7346,#2053,.T.);
#9355=EDGE_CURVE('',#7345,#7351,#953,.T.);
#9356=EDGE_CURVE('',#7351,#7347,#6047,.T.);
#9357=EDGE_CURVE('',#7352,#7353,#954,.T.);
#9358=EDGE_CURVE('',#7353,#7354,#955,.T.);
#9359=EDGE_CURVE('',#7354,#7355,#956,.T.);
#9360=EDGE_CURVE('',#7355,#7356,#2054,.T.);
#9361=EDGE_CURVE('',#7356,#7357,#6048,.T.);
#9362=EDGE_CURVE('',#7357,#7352,#2055,.T.);
#9363=EDGE_CURVE('',#7358,#7359,#957,.F.);
#9364=EDGE_CURVE('',#7360,#7358,#6049,.T.);
#9365=EDGE_CURVE('',#7360,#7361,#6050,.T.);
#9366=EDGE_CURVE('',#7359,#7361,#6051,.T.);
#9367=EDGE_CURVE('',#7362,#7362,#6052,.T.);
#9368=EDGE_CURVE('',#7362,#7363,#2056,.T.);
#9369=EDGE_CURVE('',#7363,#7363,#6053,.T.);
#9370=EDGE_CURVE('',#7364,#7365,#958,.T.);
#9371=EDGE_CURVE('',#7365,#7364,#959,.T.);
#9372=EDGE_CURVE('',#7366,#7367,#960,.T.);
#9373=EDGE_CURVE('',#7367,#7366,#961,.T.);
#9374=EDGE_CURVE('',#7326,#7368,#6054,.T.);
#9375=EDGE_CURVE('',#7369,#7368,#962,.T.);
#9376=EDGE_CURVE('',#7370,#7369,#6055,.T.);
#9377=EDGE_CURVE('',#7327,#7370,#6056,.T.);
#9378=EDGE_CURVE('',#7371,#7372,#6057,.T.);
#9379=EDGE_CURVE('',#7371,#7373,#6058,.T.);
#9380=EDGE_CURVE('',#7374,#7373,#6059,.T.);
#9381=EDGE_CURVE('',#7372,#7374,#6060,.T.);
#9382=EDGE_CURVE('',#7375,#7376,#6061,.T.);
#9383=EDGE_CURVE('',#7375,#7377,#963,.T.);
#9384=EDGE_CURVE('',#7378,#7377,#2057,.T.);
#9385=EDGE_CURVE('',#7378,#7379,#964,.T.);
#9386=EDGE_CURVE('',#7379,#7380,#6062,.T.);
#9387=EDGE_CURVE('',#7380,#7381,#965,.T.);
#9388=EDGE_CURVE('',#7381,#7382,#2058,.T.);
#9389=EDGE_CURVE('',#7382,#7376,#966,.T.);
#9390=EDGE_CURVE('',#7383,#7382,#2059,.T.);
#9391=EDGE_CURVE('',#7384,#7383,#772,.T.);
#9392=EDGE_CURVE('',#7376,#7384,#2060,.T.);
#9393=EDGE_CURVE('',#7301,#7344,#2061,.T.);
#9394=EDGE_CURVE('',#7320,#7295,#967,.T.);
#9395=EDGE_CURVE('',#7300,#7385,#968,.T.);
#9396=EDGE_CURVE('',#7385,#7305,#969,.T.);
#9397=EDGE_CURVE('',#7386,#7387,#970,.T.);
#9398=EDGE_CURVE('',#7387,#7388,#971,.T.);
#9399=EDGE_CURVE('',#7389,#7388,#972,.T.);
#9400=EDGE_CURVE('',#7390,#7389,#973,.T.);
#9401=EDGE_CURVE('',#7390,#7391,#6063,.T.);
#9402=EDGE_CURVE('',#7392,#7391,#974,.T.);
#9403=EDGE_CURVE('',#7393,#7392,#2062,.T.);
#9404=EDGE_CURVE('',#7393,#7394,#6064,.T.);
#9405=EDGE_CURVE('',#7394,#7395,#2063,.T.);
#9406=EDGE_CURVE('',#7395,#7396,#975,.T.);
#9407=EDGE_CURVE('',#7371,#7396,#976,.T.);
#9408=EDGE_CURVE('',#7386,#7372,#977,.T.);
#9409=EDGE_CURVE('',#7397,#7398,#6065,.T.);
#9410=EDGE_CURVE('',#7397,#7386,#978,.T.);
#9411=EDGE_CURVE('',#7372,#7399,#979,.T.);
#9412=EDGE_CURVE('',#7399,#7390,#980,.T.);
#9413=EDGE_CURVE('',#7389,#7398,#773,.T.);
#9414=EDGE_CURVE('',#7368,#7400,#6066,.T.);
#9415=EDGE_CURVE('',#7400,#7401,#2064,.T.);
#9416=EDGE_CURVE('',#7396,#7401,#981,.F.);
#9417=EDGE_CURVE('',#7402,#7395,#774,.T.);
#9418=EDGE_CURVE('',#7401,#7402,#982,.F.);
#9419=EDGE_CURVE('',#7400,#7370,#983,.T.);
#9420=EDGE_CURVE('',#7403,#7404,#6067,.T.);
#9421=EDGE_CURVE('',#7403,#7405,#775,.T.);
#9422=EDGE_CURVE('',#7404,#7405,#6068,.T.);
#9423=EDGE_CURVE('',#7404,#7406,#2065,.T.);
#9424=EDGE_CURVE('',#7406,#7406,#6069,.T.);
#9425=EDGE_CURVE('',#7407,#7407,#6070,.T.);
#9426=EDGE_CURVE('',#7407,#7408,#2066,.T.);
#9427=EDGE_CURVE('',#7408,#7408,#6071,.T.);
#9428=EDGE_CURVE('',#7409,#7409,#6072,.T.);
#9429=EDGE_CURVE('',#7409,#7410,#2067,.T.);
#9430=EDGE_CURVE('',#7410,#7410,#6073,.T.);
#9431=EDGE_CURVE('',#7411,#7412,#6074,.T.);
#9432=EDGE_CURVE('',#7413,#7412,#6075,.T.);
#9433=EDGE_CURVE('',#7413,#7411,#6076,.T.);
#9434=EDGE_CURVE('',#7414,#7415,#6077,.T.);
#9435=EDGE_CURVE('',#7416,#7415,#2068,.T.);
#9436=EDGE_CURVE('',#7417,#7416,#6078,.T.);
#9437=EDGE_CURVE('',#7414,#7417,#2069,.T.);
#9438=EDGE_CURVE('',#7417,#7418,#6079,.T.);
#9439=EDGE_CURVE('',#7419,#7418,#2070,.T.);
#9440=EDGE_CURVE('',#7420,#7419,#6080,.T.);
#9441=EDGE_CURVE('',#7417,#7420,#2071,.T.);
#9442=EDGE_CURVE('',#7419,#7421,#6081,.T.);
#9443=EDGE_CURVE('',#7420,#7421,#6082,.T.);
#9444=EDGE_CURVE('',#7422,#7423,#776,.T.);
#9445=EDGE_CURVE('',#7379,#7422,#2072,.T.);
#9446=EDGE_CURVE('',#7423,#7378,#2073,.T.);
#9447=EDGE_CURVE('',#7414,#7424,#6083,.T.);
#9448=EDGE_CURVE('',#7424,#7415,#6084,.T.);
#9449=EDGE_CURVE('',#7425,#7425,#6085,.T.);
#9450=EDGE_CURVE('',#7425,#7426,#2074,.T.);
#9451=EDGE_CURVE('',#7426,#7426,#6086,.T.);
#9452=EDGE_CURVE('',#7427,#7428,#984,.T.);
#9453=EDGE_CURVE('',#7428,#7429,#985,.T.);
#9454=EDGE_CURVE('',#7429,#7273,#986,.T.);
#9455=EDGE_CURVE('',#7430,#7273,#2075,.T.);
#9456=EDGE_CURVE('',#7430,#7431,#6087,.T.);
#9457=EDGE_CURVE('',#7427,#7431,#2076,.T.);
#9458=EDGE_CURVE('',#7430,#7431,#6088,.T.);
#9459=EDGE_CURVE('',#7432,#7430,#2077,.T.);
#9460=EDGE_CURVE('',#7432,#7433,#987,.T.);
#9461=EDGE_CURVE('',#7433,#7434,#988,.T.);
#9462=EDGE_CURVE('',#7431,#7434,#2078,.T.);
#9463=EDGE_CURVE('',#7435,#7435,#6089,.T.);
#9464=EDGE_CURVE('',#7435,#7367,#2079,.T.);
#9465=EDGE_CURVE('',#7365,#7436,#2080,.T.);
#9466=EDGE_CURVE('',#7436,#7436,#6090,.T.);
#9467=EDGE_CURVE('',#7437,#7341,#2081,.T.);
#9468=EDGE_CURVE('',#7437,#7438,#6091,.T.);
#9469=EDGE_CURVE('',#7438,#7340,#2082,.T.);
#9470=EDGE_CURVE('',#7439,#7439,#6092,.T.);
#9471=EDGE_CURVE('',#7439,#7440,#2083,.T.);
#9472=EDGE_CURVE('',#7440,#7440,#6093,.T.);
#9473=EDGE_CURVE('',#7334,#7441,#989,.T.);
#9474=EDGE_CURVE('',#7442,#7441,#2084,.T.);
#9475=EDGE_CURVE('',#7335,#7442,#6094,.T.);
#9476=EDGE_CURVE('',#7443,#7443,#6095,.T.);
#9477=EDGE_CURVE('',#7443,#7444,#2085,.T.);
#9478=EDGE_CURVE('',#7444,#7444,#6096,.T.);
#9479=EDGE_CURVE('',#7362,#7445,#6097,.T.);
#9480=EDGE_CURVE('',#7445,#7445,#6098,.T.);
#9481=EDGE_CURVE('',#7445,#7446,#2086,.T.);
#9482=EDGE_CURVE('',#7446,#7446,#6099,.T.);
#9483=EDGE_CURVE('',#7446,#7410,#6100,.T.);
#9484=EDGE_CURVE('',#7447,#7447,#6101,.T.);
#9485=EDGE_CURVE('',#7447,#7448,#2087,.T.);
#9486=EDGE_CURVE('',#7448,#7448,#6102,.T.);
#9487=EDGE_CURVE('',#7449,#7449,#6103,.T.);
#9488=EDGE_CURVE('',#7449,#7450,#2088,.T.);
#9489=EDGE_CURVE('',#7450,#7450,#6104,.T.);
#9490=EDGE_CURVE('',#7355,#7451,#990,.T.);
#9491=EDGE_CURVE('',#7452,#7451,#2089,.T.);
#9492=EDGE_CURVE('',#7356,#7452,#6105,.T.);
#9493=EDGE_CURVE('',#7453,#7454,#2090,.T.);
#9494=EDGE_CURVE('',#7453,#7352,#991,.T.);
#9495=EDGE_CURVE('',#7454,#7357,#6106,.T.);
#9496=EDGE_CURVE('',#7455,#7456,#2091,.T.);
#9497=EDGE_CURVE('',#7456,#7340,#2092,.T.);
#9498=EDGE_CURVE('',#7438,#7455,#2093,.T.);
#9499=EDGE_CURVE('',#7457,#7458,#2094,.T.);
#9500=EDGE_CURVE('',#7458,#7456,#6107,.T.);
#9501=EDGE_CURVE('',#7455,#7457,#6108,.T.);
#9502=EDGE_CURVE('',#7459,#7460,#6109,.T.);
#9503=EDGE_CURVE('',#7457,#7459,#2095,.T.);
#9504=EDGE_CURVE('',#7461,#7437,#2096,.T.);
#9505=EDGE_CURVE('',#7462,#7461,#6110,.T.);
#9506=EDGE_CURVE('',#7460,#7462,#2097,.T.);
#9507=EDGE_CURVE('',#7459,#7463,#2098,.T.);
#9508=EDGE_CURVE('',#7463,#7458,#2099,.T.);
#9509=EDGE_CURVE('',#7460,#7464,#2100,.T.);
#9510=EDGE_CURVE('',#7464,#7463,#6111,.T.);
#9511=EDGE_CURVE('',#7462,#7465,#2101,.T.);
#9512=EDGE_CURVE('',#7465,#7464,#2102,.T.);
#9513=EDGE_CURVE('',#7461,#7466,#2103,.T.);
#9514=EDGE_CURVE('',#7466,#7465,#6112,.T.);
#9515=EDGE_CURVE('',#7292,#7291,#2104,.T.);
#9516=EDGE_CURVE('',#7317,#7429,#6113,.T.);
#9517=EDGE_CURVE('',#7275,#7317,#992,.T.);
#9518=EDGE_CURVE('',#7272,#7432,#993,.T.);
#9519=EDGE_CURVE('',#7282,#7270,#994,.T.);
#9520=EDGE_CURVE('',#7432,#7281,#6114,.T.);
#9521=EDGE_CURVE('',#7280,#7434,#6115,.T.);
#9522=EDGE_CURVE('',#7279,#7467,#6116,.T.);
#9523=EDGE_CURVE('',#7434,#7467,#995,.T.);
#9524=EDGE_CURVE('',#7319,#7468,#6117,.T.);
#9525=EDGE_CURVE('',#7467,#7468,#996,.T.);
#9526=EDGE_CURVE('',#7319,#7279,#997,.T.);
#9527=EDGE_CURVE('',#7318,#7427,#6118,.T.);
#9528=EDGE_CURVE('',#7468,#7427,#6119,.T.);
#9529=EDGE_CURVE('',#7465,#7469,#6120,.T.);
#9530=EDGE_CURVE('',#7470,#7466,#6121,.T.);
#9531=EDGE_CURVE('',#7469,#7470,#6122,.T.);
#9532=EDGE_CURVE('',#7471,#7472,#6123,.T.);
#9533=EDGE_CURVE('',#7472,#7473,#6124,.T.);
#9534=EDGE_CURVE('',#7471,#7473,#6125,.T.);
#9535=EDGE_CURVE('',#7472,#7361,#2105,.T.);
#9536=EDGE_CURVE('',#7359,#7471,#2106,.T.);
#9537=EDGE_CURVE('',#7474,#7475,#6126,.T.);
#9538=EDGE_CURVE('',#7473,#7475,#2107,.T.);
#9539=EDGE_CURVE('',#7474,#7472,#2108,.T.);
#9540=EDGE_CURVE('',#7476,#7477,#6127,.T.);
#9541=EDGE_CURVE('',#7477,#7478,#6128,.T.);
#9542=EDGE_CURVE('',#7476,#7478,#6129,.T.);
#9543=EDGE_CURVE('',#7479,#7480,#6130,.T.);
#9544=EDGE_CURVE('',#7477,#7480,#2109,.T.);
#9545=EDGE_CURVE('',#7479,#7476,#2110,.T.);
#9546=EDGE_CURVE('',#7481,#7482,#777,.T.);
#9547=EDGE_CURVE('',#7478,#7481,#2111,.T.);
#9548=EDGE_CURVE('',#7482,#7477,#2112,.T.);
#9549=EDGE_CURVE('',#7479,#7483,#6131,.T.);
#9550=EDGE_CURVE('',#7483,#7480,#6132,.T.);
#9551=EDGE_CURVE('',#7484,#7485,#6133,.T.);
#9552=EDGE_CURVE('',#7483,#7485,#2113,.T.);
#9553=EDGE_CURVE('',#7484,#7479,#2114,.T.);
#9554=EDGE_CURVE('',#7486,#7487,#778,.T.);
#9555=EDGE_CURVE('',#7480,#7486,#2115,.T.);
#9556=EDGE_CURVE('',#7487,#7483,#2116,.T.);
#9557=EDGE_CURVE('',#7484,#7488,#6134,.T.);
#9558=EDGE_CURVE('',#7488,#7485,#6135,.T.);
#9559=EDGE_CURVE('',#7489,#7490,#779,.T.);
#9560=EDGE_CURVE('',#7488,#7489,#2117,.T.);
#9561=EDGE_CURVE('',#7490,#7484,#2118,.T.);
#9562=EDGE_CURVE('',#7491,#7414,#2119,.T.);
#9563=EDGE_CURVE('',#7491,#7492,#780,.T.);
#9564=EDGE_CURVE('',#7424,#7492,#2120,.T.);
#9565=EDGE_CURVE('',#7493,#7494,#6136,.T.);
#9566=EDGE_CURVE('',#7493,#7495,#6137,.T.);
#9567=EDGE_CURVE('',#7494,#7495,#6138,.T.);
#9568=EDGE_CURVE('',#7415,#7494,#2121,.T.);
#9569=EDGE_CURVE('',#7493,#7424,#2122,.T.);
#9570=EDGE_CURVE('',#7496,#7497,#6139,.T.);
#9571=EDGE_CURVE('',#7418,#7497,#2123,.T.);
#9572=EDGE_CURVE('',#7416,#7418,#6140,.T.);
#9573=EDGE_CURVE('',#7496,#7416,#2124,.T.);
#9574=EDGE_CURVE('',#7496,#7498,#6141,.T.);
#9575=EDGE_CURVE('',#7497,#7498,#6142,.T.);
#9576=EDGE_CURVE('',#7498,#7495,#2125,.T.);
#9577=EDGE_CURVE('',#7494,#7496,#2126,.T.);
#9578=EDGE_CURVE('',#7499,#7498,#2127,.T.);
#9579=EDGE_CURVE('',#7500,#7499,#6143,.T.);
#9580=EDGE_CURVE('',#7497,#7500,#2128,.T.);
#9581=EDGE_CURVE('',#7500,#7501,#6144,.T.);
#9582=EDGE_CURVE('',#7421,#7501,#2129,.T.);
#9583=EDGE_CURVE('',#7500,#7419,#2130,.T.);
#9584=EDGE_CURVE('',#7499,#7501,#6145,.T.);
#9585=EDGE_CURVE('',#7501,#7423,#2131,.T.);
#9586=EDGE_CURVE('',#7422,#7499,#2132,.T.);
#9587=EDGE_CURVE('',#7502,#7493,#2133,.T.);
#9588=EDGE_CURVE('',#7502,#7503,#781,.T.);
#9589=EDGE_CURVE('',#7495,#7503,#2134,.T.);
#9590=EDGE_CURVE('',#7504,#7383,#2135,.T.);
#9591=EDGE_CURVE('',#7505,#7504,#6146,.T.);
#9592=EDGE_CURVE('',#7384,#7505,#2136,.T.);
#9593=EDGE_CURVE('',#7506,#7505,#6147,.T.);
#9594=EDGE_CURVE('',#7506,#7504,#6148,.T.);
#9595=EDGE_CURVE('',#7475,#7507,#6149,.T.);
#9596=EDGE_CURVE('',#7505,#7507,#2137,.T.);
#9597=EDGE_CURVE('',#7475,#7506,#2138,.T.);
#9598=EDGE_CURVE('',#7411,#7473,#2139,.T.);
#9599=EDGE_CURVE('',#7471,#7413,#2140,.T.);
#9600=EDGE_CURVE('',#7412,#7504,#2141,.T.);
#9601=EDGE_CURVE('',#7506,#7411,#2142,.T.);
#9602=EDGE_CURVE('',#7508,#7412,#2143,.T.);
#9603=EDGE_CURVE('',#7509,#7508,#782,.T.);
#9604=EDGE_CURVE('',#7413,#7509,#2144,.T.);
#9605=EDGE_CURVE('',#7482,#7486,#2145,.T.);
#9606=EDGE_CURVE('',#7510,#7360,#2146,.T.);
#9607=EDGE_CURVE('',#7490,#7358,#2147,.T.);
#9608=EDGE_CURVE('',#7476,#7511,#2148,.T.);
#9609=EDGE_CURVE('',#7511,#7512,#2149,.T.);
#9610=EDGE_CURVE('',#7510,#7512,#6150,.T.);
#9611=EDGE_CURVE('',#7513,#7514,#2150,.T.);
#9612=EDGE_CURVE('',#7514,#7488,#2151,.T.);
#9613=EDGE_CURVE('',#7489,#7513,#2152,.T.);
#9614=EDGE_CURVE('',#7515,#7516,#2153,.T.);
#9615=EDGE_CURVE('',#7516,#7517,#6151,.T.);
#9616=EDGE_CURVE('',#7518,#7517,#2154,.T.);
#9617=EDGE_CURVE('',#7518,#7519,#783,.T.);
#9618=EDGE_CURVE('',#7487,#7519,#2155,.T.);
#9619=EDGE_CURVE('',#7485,#7515,#2156,.T.);
#9620=EDGE_CURVE('',#7451,#7520,#6152,.T.);
#9621=EDGE_CURVE('',#7520,#7521,#784,.T.);
#9622=EDGE_CURVE('',#7521,#7522,#2157,.T.);
#9623=EDGE_CURVE('',#7522,#7452,#2158,.T.);
#9624=EDGE_CURVE('',#7388,#7523,#998,.T.);
#9625=EDGE_CURVE('',#7387,#7523,#6153,.T.);
#9626=EDGE_CURVE('',#7393,#7524,#2159,.T.);
#9627=EDGE_CURVE('',#7524,#7525,#2160,.T.);
#9628=EDGE_CURVE('',#7394,#7525,#2161,.T.);
#9629=EDGE_CURVE('',#7403,#7398,#2162,.T.);
#9630=EDGE_CURVE('',#7526,#7405,#2163,.T.);
#9631=EDGE_CURVE('',#7397,#7526,#785,.T.);
#9632=EDGE_CURVE('',#7523,#7389,#786,.T.);
#9633=EDGE_CURVE('',#7526,#7387,#6154,.T.);
#9634=EDGE_CURVE('',#7390,#7527,#6155,.T.);
#9635=EDGE_CURVE('',#7528,#7527,#6156,.T.);
#9636=EDGE_CURVE('',#7391,#7528,#6157,.T.);
#9637=EDGE_CURVE('',#7399,#7374,#999,.T.);
#9638=EDGE_CURVE('',#7441,#7529,#787,.T.);
#9639=EDGE_CURVE('',#7529,#7453,#1000,.T.);
#9640=EDGE_CURVE('',#7454,#7442,#2164,.T.);
#9641=EDGE_CURVE('',#7296,#7271,#1001,.T.);
#9642=EDGE_CURVE('',#7316,#7297,#1002,.T.);
#9643=EDGE_CURVE('',#7522,#7336,#6158,.T.);
#9644=EDGE_CURVE('',#7512,#7530,#6159,.T.);
#9645=EDGE_CURVE('',#7531,#7530,#6160,.T.);
#9646=EDGE_CURVE('',#7510,#7531,#6161,.T.);
#9647=EDGE_CURVE('',#7507,#7530,#2165,.T.);
#9648=EDGE_CURVE('',#7474,#7507,#6162,.T.);
#9649=EDGE_CURVE('',#7531,#7474,#2166,.T.);
#9650=EDGE_CURVE('',#7361,#7531,#2167,.T.);
#9651=EDGE_CURVE('',#7381,#7508,#2168,.T.);
#9652=EDGE_CURVE('',#7508,#7383,#2169,.T.);
#9653=EDGE_CURVE('',#7532,#7421,#2170,.T.);
#9654=EDGE_CURVE('',#7533,#7532,#788,.T.);
#9655=EDGE_CURVE('',#7420,#7533,#2171,.T.);
#9656=EDGE_CURVE('',#7377,#7532,#2172,.T.);
#9657=EDGE_CURVE('',#7533,#7375,#2173,.T.);
#9658=EDGE_CURVE('',#7373,#7534,#1003,.T.);
#9659=EDGE_CURVE('',#7534,#7528,#1004,.T.);
#9660=EDGE_CURVE('',#7527,#7399,#1005,.T.);
#9661=EDGE_CURVE('',#7391,#7534,#1006,.T.);
#9662=EDGE_CURVE('',#7534,#7371,#1007,.T.);
#9663=EDGE_CURVE('',#7402,#7535,#2174,.T.);
#9664=EDGE_CURVE('',#7535,#7536,#1008,.T.);
#9665=EDGE_CURVE('',#7392,#7536,#2175,.T.);
#9666=EDGE_CURVE('',#7521,#7337,#1009,.T.);
#9667=EDGE_CURVE('',#7311,#7535,#789,.T.);
#9668=EDGE_CURVE('',#7298,#7309,#1010,.T.);
#9669=EDGE_CURVE('',#7536,#7314,#790,.T.);
#9670=EDGE_CURVE('',#7524,#7313,#2176,.T.);
#9671=EDGE_CURVE('',#7525,#7312,#2177,.T.);
#9672=EDGE_CURVE('',#7537,#7478,#2178,.T.);
#9673=EDGE_CURVE('',#7511,#7537,#791,.T.);
#9674=EDGE_CURVE('',#7511,#7538,#6163,.T.);
#9675=EDGE_CURVE('',#7530,#7538,#2179,.T.);
#9676=EDGE_CURVE('',#7539,#7537,#1011,.T.);
#9677=EDGE_CURVE('',#7538,#7539,#792,.T.);
#9678=EDGE_CURVE('',#7509,#7380,#2180,.T.);
#9679=EDGE_CURVE('',#7540,#7503,#2181,.T.);
#9680=EDGE_CURVE('',#7513,#7540,#2182,.T.);
#9681=EDGE_CURVE('',#7541,#7469,#2183,.T.);
#9682=EDGE_CURVE('',#7470,#7518,#2184,.T.);
#9683=EDGE_CURVE('',#7517,#7349,#2185,.T.);
#9684=EDGE_CURVE('',#7348,#7542,#6164,.T.);
#9685=EDGE_CURVE('',#7542,#7543,#2186,.T.);
#9686=EDGE_CURVE('',#7543,#7343,#2187,.T.);
#9687=EDGE_CURVE('',#7342,#7544,#2188,.T.);
#9688=EDGE_CURVE('',#7544,#7545,#6165,.T.);
#9689=EDGE_CURVE('',#7545,#7546,#2189,.T.);
#9690=EDGE_CURVE('',#7546,#7541,#6166,.T.);
#9691=EDGE_CURVE('',#7542,#7547,#2190,.T.);
#9692=EDGE_CURVE('',#7547,#7502,#2191,.T.);
#9693=EDGE_CURVE('',#7492,#7548,#2192,.T.);
#9694=EDGE_CURVE('',#7548,#7543,#6167,.T.);
#9695=EDGE_CURVE('',#7423,#7532,#2193,.T.);
#9696=EDGE_CURVE('',#7503,#7549,#2194,.T.);
#9697=EDGE_CURVE('',#7549,#7550,#6168,.T.);
#9698=EDGE_CURVE('',#7540,#7550,#2195,.T.);
#9699=EDGE_CURVE('',#7519,#7466,#2196,.T.);
#9700=EDGE_CURVE('',#7341,#7551,#2197,.T.);
#9701=EDGE_CURVE('',#7551,#7481,#2198,.T.);
#9702=EDGE_CURVE('',#7550,#7552,#1012,.T.);
#9703=EDGE_CURVE('',#7552,#7553,#2199,.T.);
#9704=EDGE_CURVE('',#7553,#7516,#2200,.T.);
#9705=EDGE_CURVE('',#7515,#7514,#6169,.T.);
#9706=EDGE_CURVE('',#7332,#7554,#1013,.T.);
#9707=EDGE_CURVE('',#7308,#7554,#1014,.T.);
#9708=EDGE_CURVE('',#7307,#7529,#1015,.T.);
#9709=EDGE_CURVE('',#7385,#7339,#1016,.T.);
#9710=EDGE_CURVE('',#7520,#7306,#1017,.T.);
#9711=EDGE_CURVE('',#7349,#7553,#6170,.T.);
#9712=EDGE_CURVE('',#7321,#7553,#6171,.T.);
#9713=EDGE_CURVE('',#7322,#7552,#1018,.T.);
#9714=EDGE_CURVE('',#7323,#7549,#6172,.T.);
#9715=EDGE_CURVE('',#7547,#7549,#1019,.T.);
#9716=EDGE_CURVE('',#7547,#7324,#6173,.T.);
#9717=EDGE_CURVE('',#7555,#7491,#2201,.T.);
#9718=EDGE_CURVE('',#7555,#7548,#1020,.T.);
#9719=EDGE_CURVE('',#7551,#7555,#793,.T.);
#9720=EDGE_CURVE('',#7464,#7541,#6174,.T.);
#9721=EDGE_CURVE('',#7463,#7546,#6175,.T.);
#9722=EDGE_CURVE('',#7458,#7545,#6176,.T.);
#9723=EDGE_CURVE('',#7456,#7544,#6177,.T.);
#9724=EDGE_CURVE('',#7554,#7299,#1021,.T.);
#9725=EDGE_CURVE('',#7290,#7320,#6178,.T.);
#9726=EDGE_CURVE('',#7289,#7295,#6179,.T.);
#9727=EDGE_CURVE('',#7287,#7556,#1022,.T.);
#9728=EDGE_CURVE('',#7557,#7286,#1023,.T.);
#9729=EDGE_CURVE('',#7556,#7557,#6180,.T.);
#9730=EDGE_CURVE('',#7556,#7557,#2202,.T.);
#9731=EDGE_CURVE('',#7558,#7539,#2203,.T.);
#9732=EDGE_CURVE('',#7558,#7559,#794,.T.);
#9733=EDGE_CURVE('',#7491,#7559,#2204,.T.);
#9734=EDGE_CURVE('',#7558,#7559,#6181,.T.);
#9735=EDGE_CURVE('',#7560,#7560,#6182,.T.);
#9736=EDGE_CURVE('',#7560,#7561,#2205,.T.);
#9737=EDGE_CURVE('',#7561,#7561,#6183,.T.);
#9738=EDGE_CURVE('',#7562,#7562,#6184,.T.);
#9739=EDGE_CURVE('',#7562,#7563,#2206,.T.);
#9740=EDGE_CURVE('',#7563,#7563,#6185,.T.);
#9741=EDGE_CURVE('',#7564,#7565,#6186,.T.);
#9742=EDGE_CURVE('',#7566,#7564,#1024,.T.);
#9743=EDGE_CURVE('',#7567,#7566,#6187,.T.);
#9744=EDGE_CURVE('',#7565,#7567,#1025,.T.);
#9745=EDGE_CURVE('',#7568,#7569,#6188,.T.);
#9746=EDGE_CURVE('',#7570,#7568,#1026,.T.);
#9747=EDGE_CURVE('',#7571,#7570,#6189,.T.);
#9748=EDGE_CURVE('',#7569,#7571,#1027,.T.);
#9749=EDGE_CURVE('',#7572,#7573,#6190,.T.);
#9750=EDGE_CURVE('',#7574,#7572,#1028,.T.);
#9751=EDGE_CURVE('',#7575,#7574,#6191,.T.);
#9752=EDGE_CURVE('',#7573,#7575,#1029,.T.);
#9753=EDGE_CURVE('',#7576,#7577,#6192,.T.);
#9754=EDGE_CURVE('',#7578,#7576,#1030,.T.);
#9755=EDGE_CURVE('',#7579,#7578,#6193,.T.);
#9756=EDGE_CURVE('',#7577,#7579,#1031,.T.);
#9757=EDGE_CURVE('',#7567,#7569,#2207,.T.);
#9758=EDGE_CURVE('',#7568,#7566,#2208,.T.);
#9759=EDGE_CURVE('',#7577,#7575,#2209,.T.);
#9760=EDGE_CURVE('',#7574,#7576,#2210,.T.);
#9761=EDGE_CURVE('',#7578,#7564,#2211,.T.);
#9762=EDGE_CURVE('',#7579,#7565,#2212,.T.);
#9763=EDGE_CURVE('',#7572,#7570,#2213,.T.);
#9764=EDGE_CURVE('',#7573,#7571,#2214,.T.);
#9765=EDGE_CURVE('',#7580,#7581,#2215,.T.);
#9766=EDGE_CURVE('',#7582,#7581,#6194,.T.);
#9767=EDGE_CURVE('',#7583,#7582,#6195,.T.);
#9768=EDGE_CURVE('',#7584,#7583,#6196,.T.);
#9769=EDGE_CURVE('',#7585,#7584,#6197,.T.);
#9770=EDGE_CURVE('',#7586,#7585,#6198,.T.);
#9771=EDGE_CURVE('',#7581,#7586,#6199,.T.);
#9772=EDGE_CURVE('',#7587,#7588,#73,.F.);
#9773=EDGE_CURVE('',#7587,#7588,#6200,.T.);
#9774=EDGE_CURVE('',#7589,#7589,#6201,.T.);
#9775=EDGE_CURVE('',#7589,#7590,#6202,.T.);
#9776=EDGE_CURVE('',#7590,#7591,#6203,.T.);
#9777=EDGE_CURVE('',#7591,#7590,#6204,.T.);
#9778=EDGE_CURVE('',#7591,#7592,#2216,.T.);
#9779=EDGE_CURVE('',#7592,#7592,#6205,.T.);
#9780=EDGE_CURVE('',#7593,#7593,#6206,.T.);
#9781=EDGE_CURVE('',#7593,#7594,#6207,.T.);
#9782=EDGE_CURVE('',#7594,#7595,#6208,.T.);
#9783=EDGE_CURVE('',#7595,#7594,#6209,.T.);
#9784=EDGE_CURVE('',#7595,#7596,#2217,.T.);
#9785=EDGE_CURVE('',#7597,#7596,#6210,.T.);
#9786=EDGE_CURVE('',#7596,#7597,#6211,.T.);
#9787=EDGE_CURVE('',#7598,#7598,#6212,.T.);
#9788=EDGE_CURVE('',#7598,#7599,#6213,.T.);
#9789=EDGE_CURVE('',#7599,#7599,#6214,.T.);
#9790=EDGE_CURVE('',#7597,#7600,#2218,.T.);
#9791=EDGE_CURVE('',#7600,#7600,#6215,.T.);
#9792=EDGE_CURVE('',#7599,#7593,#2219,.T.);
#9793=EDGE_CURVE('',#7601,#7602,#74,.T.);
#9794=EDGE_CURVE('',#7601,#7602,#6216,.T.);
#9795=EDGE_CURVE('',#7603,#7604,#75,.T.);
#9796=EDGE_CURVE('',#7603,#7604,#6217,.T.);
#9797=EDGE_CURVE('',#7605,#7606,#76,.T.);
#9798=EDGE_CURVE('',#7605,#7606,#6218,.T.);
#9799=EDGE_CURVE('',#7585,#7607,#2220,.T.);
#9800=EDGE_CURVE('',#7607,#7584,#2221,.T.);
#9801=EDGE_CURVE('',#7608,#7609,#77,.T.);
#9802=EDGE_CURVE('',#7608,#7609,#6219,.T.);
#9803=EDGE_CURVE('',#7610,#7611,#78,.T.);
#9804=EDGE_CURVE('',#7610,#7611,#6220,.T.);
#9805=EDGE_CURVE('',#7584,#7612,#2222,.T.);
#9806=EDGE_CURVE('',#7612,#7583,#2223,.T.);
#9807=EDGE_CURVE('',#7583,#7613,#2224,.T.);
#9808=EDGE_CURVE('',#7613,#7582,#2225,.T.);
#9809=EDGE_CURVE('',#7614,#7588,#2226,.T.);
#9810=EDGE_CURVE('',#7607,#7614,#2227,.T.);
#9811=EDGE_CURVE('',#7612,#7615,#2228,.T.);
#9812=EDGE_CURVE('',#7615,#7587,#2229,.T.);
#9813=EDGE_CURVE('',#7615,#7611,#2230,.T.);
#9814=EDGE_CURVE('',#7613,#7616,#2231,.T.);
#9815=EDGE_CURVE('',#7616,#7610,#2232,.T.);
#9816=EDGE_CURVE('',#7616,#7606,#2233,.T.);
#9817=EDGE_CURVE('',#7582,#7617,#2234,.T.);
#9818=EDGE_CURVE('',#7617,#7618,#2235,.T.);
#9819=EDGE_CURVE('',#7618,#7605,#2236,.T.);
#9820=EDGE_CURVE('',#7618,#7602,#2237,.T.);
#9821=EDGE_CURVE('',#7617,#7581,#2238,.T.);
#9822=EDGE_CURVE('',#7581,#7619,#2239,.T.);
#9823=EDGE_CURVE('',#7619,#7620,#2240,.T.);
#9824=EDGE_CURVE('',#7620,#7601,#2241,.T.);
#9825=EDGE_CURVE('',#7621,#7609,#2242,.T.);
#9826=EDGE_CURVE('',#7622,#7621,#2243,.T.);
#9827=EDGE_CURVE('',#7622,#7585,#2244,.T.);
#9828=EDGE_CURVE('',#7614,#7608,#2245,.T.);
#9829=EDGE_CURVE('',#7620,#7604,#2246,.T.);
#9830=EDGE_CURVE('',#7619,#7586,#2247,.T.);
#9831=EDGE_CURVE('',#7586,#7622,#2248,.T.);
#9832=EDGE_CURVE('',#7621,#7603,#2249,.T.);
#9833=ORIENTED_EDGE('',*,*,#7623,.T.);
#9834=ORIENTED_EDGE('',*,*,#7624,.T.);
#9835=ORIENTED_EDGE('',*,*,#7625,.T.);
#9836=ORIENTED_EDGE('',*,*,#7624,.F.);
#9837=ORIENTED_EDGE('',*,*,#7623,.F.);
#9838=ORIENTED_EDGE('',*,*,#7626,.T.);
#9839=ORIENTED_EDGE('',*,*,#7627,.T.);
#9840=ORIENTED_EDGE('',*,*,#7626,.F.);
#9841=ORIENTED_EDGE('',*,*,#7628,.T.);
#9842=ORIENTED_EDGE('',*,*,#7629,.T.);
#9843=ORIENTED_EDGE('',*,*,#7625,.F.);
#9844=ORIENTED_EDGE('',*,*,#7629,.F.);
#9845=ORIENTED_EDGE('',*,*,#7630,.F.);
#9846=ORIENTED_EDGE('',*,*,#7631,.T.);
#9847=ORIENTED_EDGE('',*,*,#7632,.F.);
#9848=ORIENTED_EDGE('',*,*,#7631,.F.);
#9849=ORIENTED_EDGE('',*,*,#7633,.F.);
#9850=ORIENTED_EDGE('',*,*,#7634,.T.);
#9851=ORIENTED_EDGE('',*,*,#7635,.T.);
#9852=ORIENTED_EDGE('',*,*,#7634,.F.);
#9853=ORIENTED_EDGE('',*,*,#7636,.T.);
#9854=ORIENTED_EDGE('',*,*,#7637,.T.);
#9855=ORIENTED_EDGE('',*,*,#7638,.F.);
#9856=ORIENTED_EDGE('',*,*,#7639,.T.);
#9857=ORIENTED_EDGE('',*,*,#7640,.F.);
#9858=ORIENTED_EDGE('',*,*,#7637,.F.);
#9859=ORIENTED_EDGE('',*,*,#7641,.F.);
#9860=ORIENTED_EDGE('',*,*,#7642,.F.);
#9861=ORIENTED_EDGE('',*,*,#7643,.T.);
#9862=ORIENTED_EDGE('',*,*,#7644,.T.);
#9863=ORIENTED_EDGE('',*,*,#7638,.T.);
#9864=ORIENTED_EDGE('',*,*,#7640,.T.);
#9865=ORIENTED_EDGE('',*,*,#7645,.T.);
#9866=ORIENTED_EDGE('',*,*,#7646,.T.);
#9867=ORIENTED_EDGE('',*,*,#7647,.T.);
#9868=ORIENTED_EDGE('',*,*,#7648,.T.);
#9869=ORIENTED_EDGE('',*,*,#7649,.T.);
#9870=ORIENTED_EDGE('',*,*,#7650,.T.);
#9871=ORIENTED_EDGE('',*,*,#7651,.T.);
#9872=ORIENTED_EDGE('',*,*,#7652,.T.);
#9873=ORIENTED_EDGE('',*,*,#7651,.F.);
#9874=ORIENTED_EDGE('',*,*,#7653,.F.);
#9875=ORIENTED_EDGE('',*,*,#7654,.T.);
#9876=ORIENTED_EDGE('',*,*,#7655,.F.);
#9877=ORIENTED_EDGE('',*,*,#7646,.F.);
#9878=ORIENTED_EDGE('',*,*,#7645,.F.);
#9879=ORIENTED_EDGE('',*,*,#7639,.F.);
#9880=ORIENTED_EDGE('',*,*,#7649,.F.);
#9881=ORIENTED_EDGE('',*,*,#7648,.F.);
#9882=ORIENTED_EDGE('',*,*,#7656,.F.);
#9883=ORIENTED_EDGE('',*,*,#7654,.F.);
#9884=ORIENTED_EDGE('',*,*,#7657,.T.);
#9885=ORIENTED_EDGE('',*,*,#7658,.T.);
#9886=ORIENTED_EDGE('',*,*,#7659,.F.);
#9887=ORIENTED_EDGE('',*,*,#7658,.F.);
#9888=ORIENTED_EDGE('',*,*,#7657,.F.);
#9889=ORIENTED_EDGE('',*,*,#7660,.T.);
#9890=ORIENTED_EDGE('',*,*,#7661,.T.);
#9891=ORIENTED_EDGE('',*,*,#7660,.F.);
#9892=ORIENTED_EDGE('',*,*,#7662,.F.);
#9893=ORIENTED_EDGE('',*,*,#7663,.T.);
#9894=ORIENTED_EDGE('',*,*,#7664,.T.);
#9895=ORIENTED_EDGE('',*,*,#7663,.F.);
#9896=ORIENTED_EDGE('',*,*,#7665,.T.);
#9897=ORIENTED_EDGE('',*,*,#7666,.T.);
#9898=ORIENTED_EDGE('',*,*,#7667,.F.);
#9899=ORIENTED_EDGE('',*,*,#7666,.F.);
#9900=ORIENTED_EDGE('',*,*,#7668,.T.);
#9901=ORIENTED_EDGE('',*,*,#7669,.T.);
#9902=ORIENTED_EDGE('',*,*,#7670,.F.);
#9903=ORIENTED_EDGE('',*,*,#7669,.F.);
#9904=ORIENTED_EDGE('',*,*,#7671,.F.);
#9905=ORIENTED_EDGE('',*,*,#7672,.T.);
#9906=ORIENTED_EDGE('',*,*,#7673,.T.);
#9907=ORIENTED_EDGE('',*,*,#7672,.F.);
#9908=ORIENTED_EDGE('',*,*,#7674,.T.);
#9909=ORIENTED_EDGE('',*,*,#7675,.T.);
#9910=ORIENTED_EDGE('',*,*,#7676,.F.);
#9911=ORIENTED_EDGE('',*,*,#7675,.F.);
#9912=ORIENTED_EDGE('',*,*,#7677,.F.);
#9913=ORIENTED_EDGE('',*,*,#7678,.T.);
#9914=ORIENTED_EDGE('',*,*,#7676,.T.);
#9915=ORIENTED_EDGE('',*,*,#7678,.F.);
#9916=ORIENTED_EDGE('',*,*,#7679,.T.);
#9917=ORIENTED_EDGE('',*,*,#7680,.T.);
#9918=ORIENTED_EDGE('',*,*,#7681,.F.);
#9919=ORIENTED_EDGE('',*,*,#7680,.F.);
#9920=ORIENTED_EDGE('',*,*,#7679,.F.);
#9921=ORIENTED_EDGE('',*,*,#7677,.T.);
#9922=ORIENTED_EDGE('',*,*,#7671,.T.);
#9923=ORIENTED_EDGE('',*,*,#7674,.F.);
#9924=ORIENTED_EDGE('',*,*,#7673,.F.);
#9925=ORIENTED_EDGE('',*,*,#7670,.T.);
#9926=ORIENTED_EDGE('',*,*,#7667,.T.);
#9927=ORIENTED_EDGE('',*,*,#7664,.F.);
#9928=ORIENTED_EDGE('',*,*,#7682,.F.);
#9929=ORIENTED_EDGE('',*,*,#7683,.F.);
#9930=ORIENTED_EDGE('',*,*,#7684,.F.);
#9931=ORIENTED_EDGE('',*,*,#7685,.F.);
#9932=ORIENTED_EDGE('',*,*,#7686,.F.);
#9933=ORIENTED_EDGE('',*,*,#7687,.F.);
#9934=ORIENTED_EDGE('',*,*,#7683,.T.);
#9935=ORIENTED_EDGE('',*,*,#7688,.T.);
#9936=ORIENTED_EDGE('',*,*,#7689,.F.);
#9937=ORIENTED_EDGE('',*,*,#7690,.F.);
#9938=ORIENTED_EDGE('',*,*,#7684,.T.);
#9939=ORIENTED_EDGE('',*,*,#7687,.T.);
#9940=ORIENTED_EDGE('',*,*,#7691,.F.);
#9941=ORIENTED_EDGE('',*,*,#7692,.F.);
#9942=ORIENTED_EDGE('',*,*,#7685,.T.);
#9943=ORIENTED_EDGE('',*,*,#7690,.T.);
#9944=ORIENTED_EDGE('',*,*,#7693,.F.);
#9945=ORIENTED_EDGE('',*,*,#7694,.F.);
#9946=ORIENTED_EDGE('',*,*,#7695,.F.);
#9947=ORIENTED_EDGE('',*,*,#7696,.F.);
#9948=ORIENTED_EDGE('',*,*,#7697,.F.);
#9949=ORIENTED_EDGE('',*,*,#7698,.T.);
#9950=ORIENTED_EDGE('',*,*,#7699,.F.);
#9951=ORIENTED_EDGE('',*,*,#7695,.T.);
#9952=ORIENTED_EDGE('',*,*,#7700,.T.);
#9953=ORIENTED_EDGE('',*,*,#7699,.T.);
#9954=ORIENTED_EDGE('',*,*,#7701,.T.);
#9955=ORIENTED_EDGE('',*,*,#7702,.F.);
#9956=ORIENTED_EDGE('',*,*,#7696,.T.);
#9957=ORIENTED_EDGE('',*,*,#7703,.F.);
#9958=ORIENTED_EDGE('',*,*,#7704,.T.);
#9959=ORIENTED_EDGE('',*,*,#7705,.T.);
#9960=ORIENTED_EDGE('',*,*,#7706,.F.);
#9961=ORIENTED_EDGE('',*,*,#7707,.F.);
#9962=ORIENTED_EDGE('',*,*,#7708,.T.);
#9963=ORIENTED_EDGE('',*,*,#7703,.T.);
#9964=ORIENTED_EDGE('',*,*,#7709,.F.);
#9965=ORIENTED_EDGE('',*,*,#7710,.F.);
#9966=ORIENTED_EDGE('',*,*,#7711,.T.);
#9967=ORIENTED_EDGE('',*,*,#7707,.T.);
#9968=ORIENTED_EDGE('',*,*,#7712,.F.);
#9969=ORIENTED_EDGE('',*,*,#7713,.T.);
#9970=ORIENTED_EDGE('',*,*,#7714,.T.);
#9971=ORIENTED_EDGE('',*,*,#7715,.F.);
#9972=ORIENTED_EDGE('',*,*,#7709,.T.);
#9973=ORIENTED_EDGE('',*,*,#7716,.T.);
#9974=ORIENTED_EDGE('',*,*,#7717,.T.);
#9975=ORIENTED_EDGE('',*,*,#7713,.F.);
#9976=ORIENTED_EDGE('',*,*,#7706,.T.);
#9977=ORIENTED_EDGE('',*,*,#7700,.F.);
#9978=ORIENTED_EDGE('',*,*,#7718,.T.);
#9979=ORIENTED_EDGE('',*,*,#7710,.T.);
#9980=ORIENTED_EDGE('',*,*,#7719,.F.);
#9981=ORIENTED_EDGE('',*,*,#7720,.T.);
#9982=ORIENTED_EDGE('',*,*,#7716,.F.);
#9983=ORIENTED_EDGE('',*,*,#7721,.T.);
#9984=ORIENTED_EDGE('',*,*,#7722,.F.);
#9985=ORIENTED_EDGE('',*,*,#7719,.T.);
#9986=ORIENTED_EDGE('',*,*,#7723,.T.);
#9987=ORIENTED_EDGE('',*,*,#7715,.T.);
#9988=ORIENTED_EDGE('',*,*,#7724,.T.);
#9989=ORIENTED_EDGE('',*,*,#7723,.F.);
#9990=ORIENTED_EDGE('',*,*,#7712,.T.);
#9991=ORIENTED_EDGE('',*,*,#7725,.T.);
#9992=ORIENTED_EDGE('',*,*,#7726,.F.);
#9993=ORIENTED_EDGE('',*,*,#7714,.F.);
#9994=ORIENTED_EDGE('',*,*,#7727,.T.);
#9995=ORIENTED_EDGE('',*,*,#7728,.T.);
#9996=ORIENTED_EDGE('',*,*,#7727,.F.);
#9997=ORIENTED_EDGE('',*,*,#7717,.F.);
#9998=ORIENTED_EDGE('',*,*,#7729,.T.);
#9999=ORIENTED_EDGE('',*,*,#7730,.T.);
#10000=ORIENTED_EDGE('',*,*,#7729,.F.);
#10001=ORIENTED_EDGE('',*,*,#7720,.F.);
#10002=ORIENTED_EDGE('',*,*,#7731,.T.);
#10003=ORIENTED_EDGE('',*,*,#7732,.T.);
#10004=ORIENTED_EDGE('',*,*,#7731,.F.);
#10005=ORIENTED_EDGE('',*,*,#7724,.F.);
#10006=ORIENTED_EDGE('',*,*,#7726,.T.);
#10007=ORIENTED_EDGE('',*,*,#7659,.T.);
#10008=ORIENTED_EDGE('',*,*,#7650,.F.);
#10009=ORIENTED_EDGE('',*,*,#7733,.T.);
#10010=ORIENTED_EDGE('',*,*,#7734,.T.);
#10011=ORIENTED_EDGE('',*,*,#7735,.T.);
#10012=ORIENTED_EDGE('',*,*,#7736,.T.);
#10013=ORIENTED_EDGE('',*,*,#7737,.T.);
#10014=ORIENTED_EDGE('',*,*,#7738,.T.);
#10015=ORIENTED_EDGE('',*,*,#7739,.F.);
#10016=ORIENTED_EDGE('',*,*,#7740,.F.);
#10017=ORIENTED_EDGE('',*,*,#7741,.T.);
#10018=ORIENTED_EDGE('',*,*,#7742,.T.);
#10019=ORIENTED_EDGE('',*,*,#7743,.T.);
#10020=ORIENTED_EDGE('',*,*,#7744,.F.);
#10021=ORIENTED_EDGE('',*,*,#7745,.F.);
#10022=ORIENTED_EDGE('',*,*,#7739,.T.);
#10023=ORIENTED_EDGE('',*,*,#7746,.F.);
#10024=ORIENTED_EDGE('',*,*,#7688,.F.);
#10025=ORIENTED_EDGE('',*,*,#7682,.T.);
#10026=ORIENTED_EDGE('',*,*,#7692,.T.);
#10027=ORIENTED_EDGE('',*,*,#7747,.F.);
#10028=ORIENTED_EDGE('',*,*,#7748,.F.);
#10029=ORIENTED_EDGE('',*,*,#7749,.F.);
#10030=ORIENTED_EDGE('',*,*,#7742,.F.);
#10031=ORIENTED_EDGE('',*,*,#7744,.T.);
#10032=ORIENTED_EDGE('',*,*,#7750,.T.);
#10033=ORIENTED_EDGE('',*,*,#7751,.F.);
#10034=ORIENTED_EDGE('',*,*,#7752,.F.);
#10035=ORIENTED_EDGE('',*,*,#7753,.F.);
#10036=ORIENTED_EDGE('',*,*,#7754,.T.);
#10037=ORIENTED_EDGE('',*,*,#7755,.T.);
#10038=ORIENTED_EDGE('',*,*,#7747,.T.);
#10039=ORIENTED_EDGE('',*,*,#7741,.F.);
#10040=ORIENTED_EDGE('',*,*,#7738,.F.);
#10041=ORIENTED_EDGE('',*,*,#7743,.F.);
#10042=ORIENTED_EDGE('',*,*,#7749,.T.);
#10043=ORIENTED_EDGE('',*,*,#7756,.T.);
#10044=ORIENTED_EDGE('',*,*,#7757,.T.);
#10045=ORIENTED_EDGE('',*,*,#7758,.F.);
#10046=ORIENTED_EDGE('',*,*,#7750,.F.);
#10047=ORIENTED_EDGE('',*,*,#7759,.T.);
#10048=ORIENTED_EDGE('',*,*,#7760,.T.);
#10049=ORIENTED_EDGE('',*,*,#7697,.T.);
#10050=ORIENTED_EDGE('',*,*,#7722,.T.);
#10051=ORIENTED_EDGE('',*,*,#7758,.T.);
#10052=ORIENTED_EDGE('',*,*,#7761,.T.);
#10053=ORIENTED_EDGE('',*,*,#7753,.T.);
#10054=ORIENTED_EDGE('',*,*,#7737,.F.);
#10055=ORIENTED_EDGE('',*,*,#7762,.F.);
#10056=ORIENTED_EDGE('',*,*,#7751,.T.);
#10057=ORIENTED_EDGE('',*,*,#7763,.F.);
#10058=ORIENTED_EDGE('',*,*,#7701,.F.);
#10059=ORIENTED_EDGE('',*,*,#7698,.F.);
#10060=ORIENTED_EDGE('',*,*,#7760,.F.);
#10061=ORIENTED_EDGE('',*,*,#7764,.T.);
#10062=ORIENTED_EDGE('',*,*,#7748,.T.);
#10063=ORIENTED_EDGE('',*,*,#7765,.T.);
#10064=ORIENTED_EDGE('',*,*,#7766,.T.);
#10065=ORIENTED_EDGE('',*,*,#7767,.F.);
#10066=ORIENTED_EDGE('',*,*,#7766,.F.);
#10067=ORIENTED_EDGE('',*,*,#7768,.F.);
#10068=ORIENTED_EDGE('',*,*,#7704,.F.);
#10069=ORIENTED_EDGE('',*,*,#7768,.T.);
#10070=ORIENTED_EDGE('',*,*,#7765,.F.);
#10071=ORIENTED_EDGE('',*,*,#7755,.F.);
#10072=ORIENTED_EDGE('',*,*,#7733,.F.);
#10073=ORIENTED_EDGE('',*,*,#7769,.F.);
#10074=ORIENTED_EDGE('',*,*,#7718,.F.);
#10075=ORIENTED_EDGE('',*,*,#7694,.T.);
#10076=ORIENTED_EDGE('',*,*,#7770,.F.);
#10077=ORIENTED_EDGE('',*,*,#7767,.T.);
#10078=ORIENTED_EDGE('',*,*,#7708,.F.);
#10079=ORIENTED_EDGE('',*,*,#7771,.F.);
#10080=ORIENTED_EDGE('',*,*,#7735,.F.);
#10081=ORIENTED_EDGE('',*,*,#7756,.F.);
#10082=ORIENTED_EDGE('',*,*,#7764,.F.);
#10083=ORIENTED_EDGE('',*,*,#7702,.T.);
#10084=ORIENTED_EDGE('',*,*,#7763,.T.);
#10085=ORIENTED_EDGE('',*,*,#7759,.F.);
#10086=ORIENTED_EDGE('',*,*,#7772,.F.);
#10087=ORIENTED_EDGE('',*,*,#7693,.T.);
#10088=ORIENTED_EDGE('',*,*,#7769,.T.);
#10089=ORIENTED_EDGE('',*,*,#7736,.F.);
#10090=ORIENTED_EDGE('',*,*,#7771,.T.);
#10091=ORIENTED_EDGE('',*,*,#7711,.F.);
#10092=ORIENTED_EDGE('',*,*,#7653,.T.);
#10093=ORIENTED_EDGE('',*,*,#7652,.F.);
#10094=ORIENTED_EDGE('',*,*,#7773,.F.);
#10095=ORIENTED_EDGE('',*,*,#7656,.T.);
#10096=ORIENTED_EDGE('',*,*,#7774,.F.);
#10097=ORIENTED_EDGE('',*,*,#7774,.T.);
#10098=ORIENTED_EDGE('',*,*,#7647,.F.);
#10099=ORIENTED_EDGE('',*,*,#7775,.F.);
#10100=ORIENTED_EDGE('',*,*,#7776,.F.);
#10101=ORIENTED_EDGE('',*,*,#7655,.T.);
#10102=ORIENTED_EDGE('',*,*,#7777,.F.);
#10103=ORIENTED_EDGE('',*,*,#7775,.T.);
#10104=ORIENTED_EDGE('',*,*,#7778,.F.);
#10105=ORIENTED_EDGE('',*,*,#7779,.F.);
#10106=ORIENTED_EDGE('',*,*,#7780,.T.);
#10107=ORIENTED_EDGE('',*,*,#7781,.T.);
#10108=ORIENTED_EDGE('',*,*,#7782,.F.);
#10109=ORIENTED_EDGE('',*,*,#7781,.F.);
#10110=ORIENTED_EDGE('',*,*,#7783,.T.);
#10111=ORIENTED_EDGE('',*,*,#7784,.T.);
#10112=ORIENTED_EDGE('',*,*,#7785,.F.);
#10113=ORIENTED_EDGE('',*,*,#7784,.F.);
#10114=ORIENTED_EDGE('',*,*,#7786,.T.);
#10115=ORIENTED_EDGE('',*,*,#7787,.T.);
#10116=ORIENTED_EDGE('',*,*,#7770,.T.);
#10117=ORIENTED_EDGE('',*,*,#7772,.T.);
#10118=ORIENTED_EDGE('',*,*,#7721,.F.);
#10119=ORIENTED_EDGE('',*,*,#7705,.F.);
#10120=ORIENTED_EDGE('',*,*,#7788,.F.);
#10121=ORIENTED_EDGE('',*,*,#7789,.F.);
#10122=ORIENTED_EDGE('',*,*,#7790,.T.);
#10123=ORIENTED_EDGE('',*,*,#7791,.T.);
#10124=ORIENTED_EDGE('',*,*,#7730,.F.);
#10125=ORIENTED_EDGE('',*,*,#7732,.F.);
#10126=ORIENTED_EDGE('',*,*,#7725,.F.);
#10127=ORIENTED_EDGE('',*,*,#7728,.F.);
#10128=ORIENTED_EDGE('',*,*,#7792,.F.);
#10129=ORIENTED_EDGE('',*,*,#7787,.F.);
#10130=ORIENTED_EDGE('',*,*,#7793,.T.);
#10131=ORIENTED_EDGE('',*,*,#7789,.T.);
#10132=ORIENTED_EDGE('',*,*,#7794,.F.);
#10133=ORIENTED_EDGE('',*,*,#7791,.F.);
#10134=ORIENTED_EDGE('',*,*,#7795,.T.);
#10135=ORIENTED_EDGE('',*,*,#7642,.T.);
#10136=ORIENTED_EDGE('',*,*,#7777,.T.);
#10137=ORIENTED_EDGE('',*,*,#7773,.T.);
#10138=ORIENTED_EDGE('',*,*,#7776,.T.);
#10139=ORIENTED_EDGE('',*,*,#7796,.F.);
#10140=ORIENTED_EDGE('',*,*,#7644,.F.);
#10141=ORIENTED_EDGE('',*,*,#7797,.T.);
#10142=ORIENTED_EDGE('',*,*,#7779,.T.);
#10143=ORIENTED_EDGE('',*,*,#7778,.T.);
#10144=ORIENTED_EDGE('',*,*,#7782,.T.);
#10145=ORIENTED_EDGE('',*,*,#7785,.T.);
#10146=ORIENTED_EDGE('',*,*,#7792,.T.);
#10147=ORIENTED_EDGE('',*,*,#7788,.T.);
#10148=ORIENTED_EDGE('',*,*,#7794,.T.);
#10149=ORIENTED_EDGE('',*,*,#7641,.T.);
#10150=ORIENTED_EDGE('',*,*,#7796,.T.);
#10151=ORIENTED_EDGE('',*,*,#7632,.T.);
#10152=ORIENTED_EDGE('',*,*,#7627,.F.);
#10153=ORIENTED_EDGE('',*,*,#7635,.F.);
#10154=ORIENTED_EDGE('',*,*,#7668,.F.);
#10155=ORIENTED_EDGE('',*,*,#7662,.T.);
#10156=ORIENTED_EDGE('',*,*,#7665,.F.);
#10157=ORIENTED_EDGE('',*,*,#7780,.F.);
#10158=ORIENTED_EDGE('',*,*,#7797,.F.);
#10159=ORIENTED_EDGE('',*,*,#7643,.F.);
#10160=ORIENTED_EDGE('',*,*,#7795,.F.);
#10161=ORIENTED_EDGE('',*,*,#7790,.F.);
#10162=ORIENTED_EDGE('',*,*,#7793,.F.);
#10163=ORIENTED_EDGE('',*,*,#7786,.F.);
#10164=ORIENTED_EDGE('',*,*,#7783,.F.);
#10165=ORIENTED_EDGE('',*,*,#7630,.T.);
#10166=ORIENTED_EDGE('',*,*,#7636,.F.);
#10167=ORIENTED_EDGE('',*,*,#7661,.F.);
#10168=ORIENTED_EDGE('',*,*,#7633,.T.);
#10169=ORIENTED_EDGE('',*,*,#7798,.T.);
#10170=ORIENTED_EDGE('',*,*,#7799,.F.);
#10171=ORIENTED_EDGE('',*,*,#7800,.F.);
#10172=ORIENTED_EDGE('',*,*,#7801,.T.);
#10173=ORIENTED_EDGE('',*,*,#7802,.T.);
#10174=ORIENTED_EDGE('',*,*,#7801,.F.);
#10175=ORIENTED_EDGE('',*,*,#7803,.F.);
#10176=ORIENTED_EDGE('',*,*,#7804,.T.);
#10177=ORIENTED_EDGE('',*,*,#7762,.T.);
#10178=ORIENTED_EDGE('',*,*,#7740,.T.);
#10179=ORIENTED_EDGE('',*,*,#7745,.T.);
#10180=ORIENTED_EDGE('',*,*,#7752,.T.);
#10181=ORIENTED_EDGE('',*,*,#7805,.F.);
#10182=ORIENTED_EDGE('',*,*,#7806,.F.);
#10183=ORIENTED_EDGE('',*,*,#7798,.F.);
#10184=ORIENTED_EDGE('',*,*,#7802,.F.);
#10185=ORIENTED_EDGE('',*,*,#7746,.T.);
#10186=ORIENTED_EDGE('',*,*,#7691,.T.);
#10187=ORIENTED_EDGE('',*,*,#7689,.T.);
#10188=ORIENTED_EDGE('',*,*,#7686,.T.);
#10189=ORIENTED_EDGE('',*,*,#7628,.F.);
#10190=ORIENTED_EDGE('',*,*,#7681,.T.);
#10191=ORIENTED_EDGE('',*,*,#7806,.T.);
#10192=ORIENTED_EDGE('',*,*,#7807,.F.);
#10193=ORIENTED_EDGE('',*,*,#7808,.F.);
#10194=ORIENTED_EDGE('',*,*,#7799,.T.);
#10195=ORIENTED_EDGE('',*,*,#7808,.T.);
#10196=ORIENTED_EDGE('',*,*,#7809,.T.);
#10197=ORIENTED_EDGE('',*,*,#7803,.T.);
#10198=ORIENTED_EDGE('',*,*,#7800,.T.);
#10199=ORIENTED_EDGE('',*,*,#7805,.T.);
#10200=ORIENTED_EDGE('',*,*,#7804,.F.);
#10201=ORIENTED_EDGE('',*,*,#7809,.F.);
#10202=ORIENTED_EDGE('',*,*,#7807,.T.);
#10203=ORIENTED_EDGE('',*,*,#7757,.F.);
#10204=ORIENTED_EDGE('',*,*,#7734,.F.);
#10205=ORIENTED_EDGE('',*,*,#7754,.F.);
#10206=ORIENTED_EDGE('',*,*,#7761,.F.);
#10207=ORIENTED_EDGE('',*,*,#7810,.T.);
#10208=ORIENTED_EDGE('',*,*,#7811,.T.);
#10209=ORIENTED_EDGE('',*,*,#7812,.F.);
#10210=ORIENTED_EDGE('',*,*,#7811,.F.);
#10211=ORIENTED_EDGE('',*,*,#7812,.T.);
#10212=ORIENTED_EDGE('',*,*,#7813,.T.);
#10213=ORIENTED_EDGE('',*,*,#7814,.T.);
#10214=ORIENTED_EDGE('',*,*,#7815,.T.);
#10215=ORIENTED_EDGE('',*,*,#7816,.T.);
#10216=ORIENTED_EDGE('',*,*,#7817,.T.);
#10217=ORIENTED_EDGE('',*,*,#7818,.T.);
#10218=ORIENTED_EDGE('',*,*,#7819,.T.);
#10219=ORIENTED_EDGE('',*,*,#7820,.T.);
#10220=ORIENTED_EDGE('',*,*,#7821,.T.);
#10221=ORIENTED_EDGE('',*,*,#7822,.T.);
#10222=ORIENTED_EDGE('',*,*,#7823,.T.);
#10223=ORIENTED_EDGE('',*,*,#7824,.T.);
#10224=ORIENTED_EDGE('',*,*,#7825,.T.);
#10225=ORIENTED_EDGE('',*,*,#7826,.T.);
#10226=ORIENTED_EDGE('',*,*,#7827,.T.);
#10227=ORIENTED_EDGE('',*,*,#7828,.T.);
#10228=ORIENTED_EDGE('',*,*,#7829,.T.);
#10229=ORIENTED_EDGE('',*,*,#7830,.T.);
#10230=ORIENTED_EDGE('',*,*,#7831,.T.);
#10231=ORIENTED_EDGE('',*,*,#7832,.T.);
#10232=ORIENTED_EDGE('',*,*,#7833,.T.);
#10233=ORIENTED_EDGE('',*,*,#7834,.T.);
#10234=ORIENTED_EDGE('',*,*,#7835,.T.);
#10235=ORIENTED_EDGE('',*,*,#7834,.F.);
#10236=ORIENTED_EDGE('',*,*,#7835,.F.);
#10237=ORIENTED_EDGE('',*,*,#7836,.T.);
#10238=ORIENTED_EDGE('',*,*,#7837,.T.);
#10239=ORIENTED_EDGE('',*,*,#7838,.T.);
#10240=ORIENTED_EDGE('',*,*,#7836,.F.);
#10241=ORIENTED_EDGE('',*,*,#7839,.T.);
#10242=ORIENTED_EDGE('',*,*,#7840,.T.);
#10243=ORIENTED_EDGE('',*,*,#7837,.F.);
#10244=ORIENTED_EDGE('',*,*,#7838,.F.);
#10245=ORIENTED_EDGE('',*,*,#7840,.F.);
#10246=ORIENTED_EDGE('',*,*,#7841,.T.);
#10247=ORIENTED_EDGE('',*,*,#7842,.T.);
#10248=ORIENTED_EDGE('',*,*,#7843,.T.);
#10249=ORIENTED_EDGE('',*,*,#7841,.F.);
#10250=ORIENTED_EDGE('',*,*,#7839,.F.);
#10251=ORIENTED_EDGE('',*,*,#7843,.F.);
#10252=ORIENTED_EDGE('',*,*,#7842,.F.);
#10253=ORIENTED_EDGE('',*,*,#7810,.F.);
#10254=ORIENTED_EDGE('',*,*,#7833,.F.);
#10255=ORIENTED_EDGE('',*,*,#7817,.F.);
#10256=ORIENTED_EDGE('',*,*,#7844,.T.);
#10257=ORIENTED_EDGE('',*,*,#7845,.T.);
#10258=ORIENTED_EDGE('',*,*,#7846,.F.);
#10259=ORIENTED_EDGE('',*,*,#7847,.T.);
#10260=ORIENTED_EDGE('',*,*,#7848,.T.);
#10261=ORIENTED_EDGE('',*,*,#7814,.F.);
#10262=ORIENTED_EDGE('',*,*,#7849,.T.);
#10263=ORIENTED_EDGE('',*,*,#7850,.T.);
#10264=ORIENTED_EDGE('',*,*,#7851,.T.);
#10265=ORIENTED_EDGE('',*,*,#7849,.F.);
#10266=ORIENTED_EDGE('',*,*,#7813,.F.);
#10267=ORIENTED_EDGE('',*,*,#7832,.F.);
#10268=ORIENTED_EDGE('',*,*,#7852,.T.);
#10269=ORIENTED_EDGE('',*,*,#7853,.T.);
#10270=ORIENTED_EDGE('',*,*,#7850,.F.);
#10271=ORIENTED_EDGE('',*,*,#7854,.T.);
#10272=ORIENTED_EDGE('',*,*,#7855,.T.);
#10273=ORIENTED_EDGE('',*,*,#7852,.F.);
#10274=ORIENTED_EDGE('',*,*,#7831,.F.);
#10275=ORIENTED_EDGE('',*,*,#7856,.F.);
#10276=ORIENTED_EDGE('',*,*,#7857,.T.);
#10277=ORIENTED_EDGE('',*,*,#7854,.F.);
#10278=ORIENTED_EDGE('',*,*,#7830,.F.);
#10279=ORIENTED_EDGE('',*,*,#7858,.T.);
#10280=ORIENTED_EDGE('',*,*,#7856,.T.);
#10281=ORIENTED_EDGE('',*,*,#7829,.F.);
#10282=ORIENTED_EDGE('',*,*,#7859,.T.);
#10283=ORIENTED_EDGE('',*,*,#7860,.T.);
#10284=ORIENTED_EDGE('',*,*,#7861,.T.);
#10285=ORIENTED_EDGE('',*,*,#7859,.F.);
#10286=ORIENTED_EDGE('',*,*,#7828,.F.);
#10287=ORIENTED_EDGE('',*,*,#7827,.F.);
#10288=ORIENTED_EDGE('',*,*,#7862,.T.);
#10289=ORIENTED_EDGE('',*,*,#7863,.T.);
#10290=ORIENTED_EDGE('',*,*,#7860,.F.);
#10291=ORIENTED_EDGE('',*,*,#7864,.T.);
#10292=ORIENTED_EDGE('',*,*,#7865,.T.);
#10293=ORIENTED_EDGE('',*,*,#7862,.F.);
#10294=ORIENTED_EDGE('',*,*,#7826,.F.);
#10295=ORIENTED_EDGE('',*,*,#7866,.F.);
#10296=ORIENTED_EDGE('',*,*,#7867,.T.);
#10297=ORIENTED_EDGE('',*,*,#7864,.F.);
#10298=ORIENTED_EDGE('',*,*,#7825,.F.);
#10299=ORIENTED_EDGE('',*,*,#7868,.T.);
#10300=ORIENTED_EDGE('',*,*,#7866,.T.);
#10301=ORIENTED_EDGE('',*,*,#7824,.F.);
#10302=ORIENTED_EDGE('',*,*,#7869,.T.);
#10303=ORIENTED_EDGE('',*,*,#7870,.T.);
#10304=ORIENTED_EDGE('',*,*,#7871,.T.);
#10305=ORIENTED_EDGE('',*,*,#7869,.F.);
#10306=ORIENTED_EDGE('',*,*,#7823,.F.);
#10307=ORIENTED_EDGE('',*,*,#7822,.F.);
#10308=ORIENTED_EDGE('',*,*,#7872,.T.);
#10309=ORIENTED_EDGE('',*,*,#7873,.T.);
#10310=ORIENTED_EDGE('',*,*,#7870,.F.);
#10311=ORIENTED_EDGE('',*,*,#7874,.T.);
#10312=ORIENTED_EDGE('',*,*,#7875,.T.);
#10313=ORIENTED_EDGE('',*,*,#7872,.F.);
#10314=ORIENTED_EDGE('',*,*,#7821,.F.);
#10315=ORIENTED_EDGE('',*,*,#7876,.F.);
#10316=ORIENTED_EDGE('',*,*,#7877,.T.);
#10317=ORIENTED_EDGE('',*,*,#7874,.F.);
#10318=ORIENTED_EDGE('',*,*,#7820,.F.);
#10319=ORIENTED_EDGE('',*,*,#7878,.T.);
#10320=ORIENTED_EDGE('',*,*,#7876,.T.);
#10321=ORIENTED_EDGE('',*,*,#7819,.F.);
#10322=ORIENTED_EDGE('',*,*,#7879,.T.);
#10323=ORIENTED_EDGE('',*,*,#7846,.T.);
#10324=ORIENTED_EDGE('',*,*,#7880,.T.);
#10325=ORIENTED_EDGE('',*,*,#7879,.F.);
#10326=ORIENTED_EDGE('',*,*,#7818,.F.);
#10327=ORIENTED_EDGE('',*,*,#7881,.F.);
#10328=ORIENTED_EDGE('',*,*,#7847,.F.);
#10329=ORIENTED_EDGE('',*,*,#7851,.F.);
#10330=ORIENTED_EDGE('',*,*,#7853,.F.);
#10331=ORIENTED_EDGE('',*,*,#7855,.F.);
#10332=ORIENTED_EDGE('',*,*,#7857,.F.);
#10333=ORIENTED_EDGE('',*,*,#7858,.F.);
#10334=ORIENTED_EDGE('',*,*,#7861,.F.);
#10335=ORIENTED_EDGE('',*,*,#7863,.F.);
#10336=ORIENTED_EDGE('',*,*,#7865,.F.);
#10337=ORIENTED_EDGE('',*,*,#7867,.F.);
#10338=ORIENTED_EDGE('',*,*,#7868,.F.);
#10339=ORIENTED_EDGE('',*,*,#7871,.F.);
#10340=ORIENTED_EDGE('',*,*,#7873,.F.);
#10341=ORIENTED_EDGE('',*,*,#7875,.F.);
#10342=ORIENTED_EDGE('',*,*,#7877,.F.);
#10343=ORIENTED_EDGE('',*,*,#7878,.F.);
#10344=ORIENTED_EDGE('',*,*,#7880,.F.);
#10345=ORIENTED_EDGE('',*,*,#7845,.F.);
#10346=ORIENTED_EDGE('',*,*,#7882,.F.);
#10347=ORIENTED_EDGE('',*,*,#7883,.T.);
#10348=ORIENTED_EDGE('',*,*,#7882,.T.);
#10349=ORIENTED_EDGE('',*,*,#7844,.F.);
#10350=ORIENTED_EDGE('',*,*,#7816,.F.);
#10351=ORIENTED_EDGE('',*,*,#7848,.F.);
#10352=ORIENTED_EDGE('',*,*,#7881,.T.);
#10353=ORIENTED_EDGE('',*,*,#7883,.F.);
#10354=ORIENTED_EDGE('',*,*,#7815,.F.);
#10355=ORIENTED_EDGE('',*,*,#7884,.F.);
#10356=ORIENTED_EDGE('',*,*,#7885,.T.);
#10357=ORIENTED_EDGE('',*,*,#7886,.T.);
#10358=ORIENTED_EDGE('',*,*,#7887,.T.);
#10359=ORIENTED_EDGE('',*,*,#7888,.T.);
#10360=ORIENTED_EDGE('',*,*,#7889,.F.);
#10361=ORIENTED_EDGE('',*,*,#7890,.F.);
#10362=ORIENTED_EDGE('',*,*,#7891,.F.);
#10363=ORIENTED_EDGE('',*,*,#7892,.T.);
#10364=ORIENTED_EDGE('',*,*,#7893,.T.);
#10365=ORIENTED_EDGE('',*,*,#7894,.T.);
#10366=ORIENTED_EDGE('',*,*,#7895,.T.);
#10367=ORIENTED_EDGE('',*,*,#7896,.F.);
#10368=ORIENTED_EDGE('',*,*,#7895,.F.);
#10369=ORIENTED_EDGE('',*,*,#7897,.T.);
#10370=ORIENTED_EDGE('',*,*,#7898,.T.);
#10371=ORIENTED_EDGE('',*,*,#7896,.T.);
#10372=ORIENTED_EDGE('',*,*,#7899,.T.);
#10373=ORIENTED_EDGE('',*,*,#7900,.T.);
#10374=ORIENTED_EDGE('',*,*,#7901,.T.);
#10375=ORIENTED_EDGE('',*,*,#7902,.T.);
#10376=ORIENTED_EDGE('',*,*,#7903,.T.);
#10377=ORIENTED_EDGE('',*,*,#7904,.T.);
#10378=ORIENTED_EDGE('',*,*,#7905,.T.);
#10379=ORIENTED_EDGE('',*,*,#7906,.T.);
#10380=ORIENTED_EDGE('',*,*,#7907,.T.);
#10381=ORIENTED_EDGE('',*,*,#7908,.T.);
#10382=ORIENTED_EDGE('',*,*,#7909,.T.);
#10383=ORIENTED_EDGE('',*,*,#7910,.T.);
#10384=ORIENTED_EDGE('',*,*,#7911,.T.);
#10385=ORIENTED_EDGE('',*,*,#7912,.T.);
#10386=ORIENTED_EDGE('',*,*,#7913,.T.);
#10387=ORIENTED_EDGE('',*,*,#7914,.T.);
#10388=ORIENTED_EDGE('',*,*,#7915,.T.);
#10389=ORIENTED_EDGE('',*,*,#7916,.T.);
#10390=ORIENTED_EDGE('',*,*,#7917,.T.);
#10391=ORIENTED_EDGE('',*,*,#7918,.T.);
#10392=ORIENTED_EDGE('',*,*,#7919,.T.);
#10393=ORIENTED_EDGE('',*,*,#7920,.T.);
#10394=ORIENTED_EDGE('',*,*,#7921,.F.);
#10395=ORIENTED_EDGE('',*,*,#7922,.T.);
#10396=ORIENTED_EDGE('',*,*,#7923,.T.);
#10397=ORIENTED_EDGE('',*,*,#7924,.T.);
#10398=ORIENTED_EDGE('',*,*,#7925,.T.);
#10399=ORIENTED_EDGE('',*,*,#7926,.T.);
#10400=ORIENTED_EDGE('',*,*,#7927,.F.);
#10401=ORIENTED_EDGE('',*,*,#7926,.F.);
#10402=ORIENTED_EDGE('',*,*,#7928,.T.);
#10403=ORIENTED_EDGE('',*,*,#7929,.F.);
#10404=ORIENTED_EDGE('',*,*,#7930,.F.);
#10405=ORIENTED_EDGE('',*,*,#7931,.F.);
#10406=ORIENTED_EDGE('',*,*,#7932,.F.);
#10407=ORIENTED_EDGE('',*,*,#7920,.F.);
#10408=ORIENTED_EDGE('',*,*,#7933,.T.);
#10409=ORIENTED_EDGE('',*,*,#7934,.F.);
#10410=ORIENTED_EDGE('',*,*,#7935,.F.);
#10411=ORIENTED_EDGE('',*,*,#7936,.F.);
#10412=ORIENTED_EDGE('',*,*,#7937,.F.);
#10413=ORIENTED_EDGE('',*,*,#7938,.T.);
#10414=ORIENTED_EDGE('',*,*,#7939,.T.);
#10415=ORIENTED_EDGE('',*,*,#7940,.T.);
#10416=ORIENTED_EDGE('',*,*,#7941,.F.);
#10417=ORIENTED_EDGE('',*,*,#7942,.T.);
#10418=ORIENTED_EDGE('',*,*,#7943,.T.);
#10419=ORIENTED_EDGE('',*,*,#7944,.F.);
#10420=ORIENTED_EDGE('',*,*,#7945,.F.);
#10421=ORIENTED_EDGE('',*,*,#7946,.T.);
#10422=ORIENTED_EDGE('',*,*,#7947,.T.);
#10423=ORIENTED_EDGE('',*,*,#7948,.T.);
#10424=ORIENTED_EDGE('',*,*,#7949,.T.);
#10425=ORIENTED_EDGE('',*,*,#7950,.T.);
#10426=ORIENTED_EDGE('',*,*,#7951,.T.);
#10427=ORIENTED_EDGE('',*,*,#7952,.F.);
#10428=ORIENTED_EDGE('',*,*,#7953,.F.);
#10429=ORIENTED_EDGE('',*,*,#7954,.F.);
#10430=ORIENTED_EDGE('',*,*,#7955,.F.);
#10431=ORIENTED_EDGE('',*,*,#7956,.F.);
#10432=ORIENTED_EDGE('',*,*,#7957,.T.);
#10433=ORIENTED_EDGE('',*,*,#7958,.T.);
#10434=ORIENTED_EDGE('',*,*,#7959,.T.);
#10435=ORIENTED_EDGE('',*,*,#7960,.T.);
#10436=ORIENTED_EDGE('',*,*,#7961,.T.);
#10437=ORIENTED_EDGE('',*,*,#7962,.T.);
#10438=ORIENTED_EDGE('',*,*,#7963,.T.);
#10439=ORIENTED_EDGE('',*,*,#7964,.T.);
#10440=ORIENTED_EDGE('',*,*,#7965,.T.);
#10441=ORIENTED_EDGE('',*,*,#7966,.T.);
#10442=ORIENTED_EDGE('',*,*,#7967,.T.);
#10443=ORIENTED_EDGE('',*,*,#7968,.T.);
#10444=ORIENTED_EDGE('',*,*,#7969,.T.);
#10445=ORIENTED_EDGE('',*,*,#7970,.T.);
#10446=ORIENTED_EDGE('',*,*,#7971,.T.);
#10447=ORIENTED_EDGE('',*,*,#7972,.T.);
#10448=ORIENTED_EDGE('',*,*,#7973,.T.);
#10449=ORIENTED_EDGE('',*,*,#7974,.T.);
#10450=ORIENTED_EDGE('',*,*,#7975,.T.);
#10451=ORIENTED_EDGE('',*,*,#7976,.T.);
#10452=ORIENTED_EDGE('',*,*,#7977,.T.);
#10453=ORIENTED_EDGE('',*,*,#7978,.T.);
#10454=ORIENTED_EDGE('',*,*,#7979,.T.);
#10455=ORIENTED_EDGE('',*,*,#7980,.T.);
#10456=ORIENTED_EDGE('',*,*,#7981,.T.);
#10457=ORIENTED_EDGE('',*,*,#7957,.F.);
#10458=ORIENTED_EDGE('',*,*,#7981,.F.);
#10459=ORIENTED_EDGE('',*,*,#7982,.T.);
#10460=ORIENTED_EDGE('',*,*,#7983,.T.);
#10461=ORIENTED_EDGE('',*,*,#7984,.F.);
#10462=ORIENTED_EDGE('',*,*,#7929,.T.);
#10463=ORIENTED_EDGE('',*,*,#7985,.T.);
#10464=ORIENTED_EDGE('',*,*,#7940,.F.);
#10465=ORIENTED_EDGE('',*,*,#7887,.F.);
#10466=ORIENTED_EDGE('',*,*,#7938,.F.);
#10467=ORIENTED_EDGE('',*,*,#7986,.F.);
#10468=ORIENTED_EDGE('',*,*,#7931,.T.);
#10469=ORIENTED_EDGE('',*,*,#7924,.F.);
#10470=ORIENTED_EDGE('',*,*,#7987,.T.);
#10471=ORIENTED_EDGE('',*,*,#7934,.T.);
#10472=ORIENTED_EDGE('',*,*,#7988,.T.);
#10473=ORIENTED_EDGE('',*,*,#7949,.F.);
#10474=ORIENTED_EDGE('',*,*,#7982,.F.);
#10475=ORIENTED_EDGE('',*,*,#7980,.F.);
#10476=ORIENTED_EDGE('',*,*,#7989,.F.);
#10477=ORIENTED_EDGE('',*,*,#7990,.T.);
#10478=ORIENTED_EDGE('',*,*,#7991,.F.);
#10479=ORIENTED_EDGE('',*,*,#7960,.F.);
#10480=ORIENTED_EDGE('',*,*,#7991,.T.);
#10481=ORIENTED_EDGE('',*,*,#7992,.T.);
#10482=ORIENTED_EDGE('',*,*,#7993,.F.);
#10483=ORIENTED_EDGE('',*,*,#7961,.F.);
#10484=ORIENTED_EDGE('',*,*,#7990,.F.);
#10485=ORIENTED_EDGE('',*,*,#7994,.F.);
#10486=ORIENTED_EDGE('',*,*,#7995,.F.);
#10487=ORIENTED_EDGE('',*,*,#7996,.F.);
#10488=ORIENTED_EDGE('',*,*,#7997,.F.);
#10489=ORIENTED_EDGE('',*,*,#7998,.F.);
#10490=ORIENTED_EDGE('',*,*,#7999,.F.);
#10491=ORIENTED_EDGE('',*,*,#8000,.F.);
#10492=ORIENTED_EDGE('',*,*,#8001,.F.);
#10493=ORIENTED_EDGE('',*,*,#8002,.F.);
#10494=ORIENTED_EDGE('',*,*,#8003,.F.);
#10495=ORIENTED_EDGE('',*,*,#8004,.F.);
#10496=ORIENTED_EDGE('',*,*,#8005,.F.);
#10497=ORIENTED_EDGE('',*,*,#8006,.F.);
#10498=ORIENTED_EDGE('',*,*,#8007,.F.);
#10499=ORIENTED_EDGE('',*,*,#8008,.F.);
#10500=ORIENTED_EDGE('',*,*,#8009,.F.);
#10501=ORIENTED_EDGE('',*,*,#8010,.F.);
#10502=ORIENTED_EDGE('',*,*,#8011,.F.);
#10503=ORIENTED_EDGE('',*,*,#7992,.F.);
#10504=ORIENTED_EDGE('',*,*,#8012,.T.);
#10505=ORIENTED_EDGE('',*,*,#8010,.T.);
#10506=ORIENTED_EDGE('',*,*,#8013,.F.);
#10507=ORIENTED_EDGE('',*,*,#7963,.F.);
#10508=ORIENTED_EDGE('',*,*,#8009,.T.);
#10509=ORIENTED_EDGE('',*,*,#8014,.T.);
#10510=ORIENTED_EDGE('',*,*,#7964,.F.);
#10511=ORIENTED_EDGE('',*,*,#8013,.T.);
#10512=ORIENTED_EDGE('',*,*,#8014,.F.);
#10513=ORIENTED_EDGE('',*,*,#8008,.T.);
#10514=ORIENTED_EDGE('',*,*,#8015,.F.);
#10515=ORIENTED_EDGE('',*,*,#7965,.F.);
#10516=ORIENTED_EDGE('',*,*,#8015,.T.);
#10517=ORIENTED_EDGE('',*,*,#8007,.T.);
#10518=ORIENTED_EDGE('',*,*,#8016,.F.);
#10519=ORIENTED_EDGE('',*,*,#7966,.F.);
#10520=ORIENTED_EDGE('',*,*,#7967,.F.);
#10521=ORIENTED_EDGE('',*,*,#8016,.T.);
#10522=ORIENTED_EDGE('',*,*,#8006,.T.);
#10523=ORIENTED_EDGE('',*,*,#8017,.F.);
#10524=ORIENTED_EDGE('',*,*,#8017,.T.);
#10525=ORIENTED_EDGE('',*,*,#8005,.T.);
#10526=ORIENTED_EDGE('',*,*,#8018,.F.);
#10527=ORIENTED_EDGE('',*,*,#7968,.F.);
#10528=ORIENTED_EDGE('',*,*,#8004,.T.);
#10529=ORIENTED_EDGE('',*,*,#8019,.T.);
#10530=ORIENTED_EDGE('',*,*,#7969,.F.);
#10531=ORIENTED_EDGE('',*,*,#8018,.T.);
#10532=ORIENTED_EDGE('',*,*,#8019,.F.);
#10533=ORIENTED_EDGE('',*,*,#8003,.T.);
#10534=ORIENTED_EDGE('',*,*,#8020,.F.);
#10535=ORIENTED_EDGE('',*,*,#7970,.F.);
#10536=ORIENTED_EDGE('',*,*,#8020,.T.);
#10537=ORIENTED_EDGE('',*,*,#8002,.T.);
#10538=ORIENTED_EDGE('',*,*,#8021,.F.);
#10539=ORIENTED_EDGE('',*,*,#7971,.F.);
#10540=ORIENTED_EDGE('',*,*,#7972,.F.);
#10541=ORIENTED_EDGE('',*,*,#8021,.T.);
#10542=ORIENTED_EDGE('',*,*,#8001,.T.);
#10543=ORIENTED_EDGE('',*,*,#8022,.F.);
#10544=ORIENTED_EDGE('',*,*,#8022,.T.);
#10545=ORIENTED_EDGE('',*,*,#8000,.T.);
#10546=ORIENTED_EDGE('',*,*,#8023,.F.);
#10547=ORIENTED_EDGE('',*,*,#7973,.F.);
#10548=ORIENTED_EDGE('',*,*,#7999,.T.);
#10549=ORIENTED_EDGE('',*,*,#8024,.T.);
#10550=ORIENTED_EDGE('',*,*,#7974,.F.);
#10551=ORIENTED_EDGE('',*,*,#8023,.T.);
#10552=ORIENTED_EDGE('',*,*,#8024,.F.);
#10553=ORIENTED_EDGE('',*,*,#7998,.T.);
#10554=ORIENTED_EDGE('',*,*,#8025,.F.);
#10555=ORIENTED_EDGE('',*,*,#7975,.F.);
#10556=ORIENTED_EDGE('',*,*,#8025,.T.);
#10557=ORIENTED_EDGE('',*,*,#7997,.T.);
#10558=ORIENTED_EDGE('',*,*,#8026,.F.);
#10559=ORIENTED_EDGE('',*,*,#7976,.F.);
#10560=ORIENTED_EDGE('',*,*,#7977,.F.);
#10561=ORIENTED_EDGE('',*,*,#8026,.T.);
#10562=ORIENTED_EDGE('',*,*,#7996,.T.);
#10563=ORIENTED_EDGE('',*,*,#8027,.F.);
#10564=ORIENTED_EDGE('',*,*,#8027,.T.);
#10565=ORIENTED_EDGE('',*,*,#7995,.T.);
#10566=ORIENTED_EDGE('',*,*,#8028,.F.);
#10567=ORIENTED_EDGE('',*,*,#7958,.F.);
#10568=ORIENTED_EDGE('',*,*,#7994,.T.);
#10569=ORIENTED_EDGE('',*,*,#7989,.T.);
#10570=ORIENTED_EDGE('',*,*,#7959,.F.);
#10571=ORIENTED_EDGE('',*,*,#8028,.T.);
#10572=ORIENTED_EDGE('',*,*,#7962,.F.);
#10573=ORIENTED_EDGE('',*,*,#7993,.T.);
#10574=ORIENTED_EDGE('',*,*,#8011,.T.);
#10575=ORIENTED_EDGE('',*,*,#8012,.F.);
#10576=ORIENTED_EDGE('',*,*,#7978,.F.);
#10577=ORIENTED_EDGE('',*,*,#7953,.T.);
#10578=ORIENTED_EDGE('',*,*,#7979,.F.);
#10579=ORIENTED_EDGE('',*,*,#7952,.T.);
#10580=ORIENTED_EDGE('',*,*,#8029,.T.);
#10581=ORIENTED_EDGE('',*,*,#7950,.F.);
#10582=ORIENTED_EDGE('',*,*,#7983,.F.);
#10583=ORIENTED_EDGE('',*,*,#7948,.F.);
#10584=ORIENTED_EDGE('',*,*,#7893,.F.);
#10585=ORIENTED_EDGE('',*,*,#7954,.T.);
#10586=ORIENTED_EDGE('',*,*,#7919,.F.);
#10587=ORIENTED_EDGE('',*,*,#7937,.T.);
#10588=ORIENTED_EDGE('',*,*,#8030,.T.);
#10589=ORIENTED_EDGE('',*,*,#7921,.T.);
#10590=ORIENTED_EDGE('',*,*,#7932,.T.);
#10591=ORIENTED_EDGE('',*,*,#7986,.T.);
#10592=ORIENTED_EDGE('',*,*,#8029,.F.);
#10593=ORIENTED_EDGE('',*,*,#7951,.F.);
#10594=ORIENTED_EDGE('',*,*,#7927,.T.);
#10595=ORIENTED_EDGE('',*,*,#7898,.F.);
#10596=ORIENTED_EDGE('',*,*,#7946,.F.);
#10597=ORIENTED_EDGE('',*,*,#8031,.F.);
#10598=ORIENTED_EDGE('',*,*,#7956,.T.);
#10599=ORIENTED_EDGE('',*,*,#7945,.T.);
#10600=ORIENTED_EDGE('',*,*,#8031,.T.);
#10601=ORIENTED_EDGE('',*,*,#7925,.F.);
#10602=ORIENTED_EDGE('',*,*,#7988,.F.);
#10603=ORIENTED_EDGE('',*,*,#7933,.F.);
#10604=ORIENTED_EDGE('',*,*,#7985,.F.);
#10605=ORIENTED_EDGE('',*,*,#7928,.F.);
#10606=ORIENTED_EDGE('',*,*,#8032,.F.);
#10607=ORIENTED_EDGE('',*,*,#7943,.F.);
#10608=ORIENTED_EDGE('',*,*,#8032,.T.);
#10609=ORIENTED_EDGE('',*,*,#7942,.F.);
#10610=ORIENTED_EDGE('',*,*,#8033,.F.);
#10611=ORIENTED_EDGE('',*,*,#7944,.T.);
#10612=ORIENTED_EDGE('',*,*,#7941,.T.);
#10613=ORIENTED_EDGE('',*,*,#8033,.T.);
#10614=ORIENTED_EDGE('',*,*,#7936,.T.);
#10615=ORIENTED_EDGE('',*,*,#7891,.T.);
#10616=ORIENTED_EDGE('',*,*,#7922,.F.);
#10617=ORIENTED_EDGE('',*,*,#8030,.F.);
#10618=ORIENTED_EDGE('',*,*,#8034,.F.);
#10619=ORIENTED_EDGE('',*,*,#8035,.F.);
#10620=ORIENTED_EDGE('',*,*,#8036,.F.);
#10621=ORIENTED_EDGE('',*,*,#8037,.F.);
#10622=ORIENTED_EDGE('',*,*,#8038,.F.);
#10623=ORIENTED_EDGE('',*,*,#8039,.F.);
#10624=ORIENTED_EDGE('',*,*,#8040,.F.);
#10625=ORIENTED_EDGE('',*,*,#8041,.F.);
#10626=ORIENTED_EDGE('',*,*,#8042,.F.);
#10627=ORIENTED_EDGE('',*,*,#8043,.F.);
#10628=ORIENTED_EDGE('',*,*,#8044,.F.);
#10629=ORIENTED_EDGE('',*,*,#8045,.F.);
#10630=ORIENTED_EDGE('',*,*,#8046,.F.);
#10631=ORIENTED_EDGE('',*,*,#8047,.F.);
#10632=ORIENTED_EDGE('',*,*,#8048,.F.);
#10633=ORIENTED_EDGE('',*,*,#8049,.F.);
#10634=ORIENTED_EDGE('',*,*,#8050,.F.);
#10635=ORIENTED_EDGE('',*,*,#8051,.F.);
#10636=ORIENTED_EDGE('',*,*,#8052,.F.);
#10637=ORIENTED_EDGE('',*,*,#8053,.F.);
#10638=ORIENTED_EDGE('',*,*,#8054,.T.);
#10639=ORIENTED_EDGE('',*,*,#8036,.T.);
#10640=ORIENTED_EDGE('',*,*,#8055,.F.);
#10641=ORIENTED_EDGE('',*,*,#7899,.F.);
#10642=ORIENTED_EDGE('',*,*,#7918,.F.);
#10643=ORIENTED_EDGE('',*,*,#8056,.T.);
#10644=ORIENTED_EDGE('',*,*,#8037,.T.);
#10645=ORIENTED_EDGE('',*,*,#8054,.F.);
#10646=ORIENTED_EDGE('',*,*,#8057,.T.);
#10647=ORIENTED_EDGE('',*,*,#8038,.T.);
#10648=ORIENTED_EDGE('',*,*,#8056,.F.);
#10649=ORIENTED_EDGE('',*,*,#7917,.F.);
#10650=ORIENTED_EDGE('',*,*,#8058,.F.);
#10651=ORIENTED_EDGE('',*,*,#8039,.T.);
#10652=ORIENTED_EDGE('',*,*,#8057,.F.);
#10653=ORIENTED_EDGE('',*,*,#7916,.F.);
#10654=ORIENTED_EDGE('',*,*,#8040,.T.);
#10655=ORIENTED_EDGE('',*,*,#8058,.T.);
#10656=ORIENTED_EDGE('',*,*,#7915,.F.);
#10657=ORIENTED_EDGE('',*,*,#8059,.T.);
#10658=ORIENTED_EDGE('',*,*,#8060,.T.);
#10659=ORIENTED_EDGE('',*,*,#8041,.T.);
#10660=ORIENTED_EDGE('',*,*,#8059,.F.);
#10661=ORIENTED_EDGE('',*,*,#7914,.F.);
#10662=ORIENTED_EDGE('',*,*,#7913,.F.);
#10663=ORIENTED_EDGE('',*,*,#8061,.T.);
#10664=ORIENTED_EDGE('',*,*,#8042,.T.);
#10665=ORIENTED_EDGE('',*,*,#8060,.F.);
#10666=ORIENTED_EDGE('',*,*,#8062,.T.);
#10667=ORIENTED_EDGE('',*,*,#8043,.T.);
#10668=ORIENTED_EDGE('',*,*,#8061,.F.);
#10669=ORIENTED_EDGE('',*,*,#7912,.F.);
#10670=ORIENTED_EDGE('',*,*,#8063,.F.);
#10671=ORIENTED_EDGE('',*,*,#8044,.T.);
#10672=ORIENTED_EDGE('',*,*,#8062,.F.);
#10673=ORIENTED_EDGE('',*,*,#7911,.F.);
#10674=ORIENTED_EDGE('',*,*,#8045,.T.);
#10675=ORIENTED_EDGE('',*,*,#8063,.T.);
#10676=ORIENTED_EDGE('',*,*,#7910,.F.);
#10677=ORIENTED_EDGE('',*,*,#8064,.T.);
#10678=ORIENTED_EDGE('',*,*,#8065,.T.);
#10679=ORIENTED_EDGE('',*,*,#8046,.T.);
#10680=ORIENTED_EDGE('',*,*,#8064,.F.);
#10681=ORIENTED_EDGE('',*,*,#7909,.F.);
#10682=ORIENTED_EDGE('',*,*,#7908,.F.);
#10683=ORIENTED_EDGE('',*,*,#8066,.T.);
#10684=ORIENTED_EDGE('',*,*,#8047,.T.);
#10685=ORIENTED_EDGE('',*,*,#8065,.F.);
#10686=ORIENTED_EDGE('',*,*,#8067,.T.);
#10687=ORIENTED_EDGE('',*,*,#8048,.T.);
#10688=ORIENTED_EDGE('',*,*,#8066,.F.);
#10689=ORIENTED_EDGE('',*,*,#7907,.F.);
#10690=ORIENTED_EDGE('',*,*,#8068,.F.);
#10691=ORIENTED_EDGE('',*,*,#8049,.T.);
#10692=ORIENTED_EDGE('',*,*,#8067,.F.);
#10693=ORIENTED_EDGE('',*,*,#7906,.F.);
#10694=ORIENTED_EDGE('',*,*,#8050,.T.);
#10695=ORIENTED_EDGE('',*,*,#8068,.T.);
#10696=ORIENTED_EDGE('',*,*,#7905,.F.);
#10697=ORIENTED_EDGE('',*,*,#8069,.T.);
#10698=ORIENTED_EDGE('',*,*,#8070,.T.);
#10699=ORIENTED_EDGE('',*,*,#8051,.T.);
#10700=ORIENTED_EDGE('',*,*,#8069,.F.);
#10701=ORIENTED_EDGE('',*,*,#7904,.F.);
#10702=ORIENTED_EDGE('',*,*,#7903,.F.);
#10703=ORIENTED_EDGE('',*,*,#8071,.T.);
#10704=ORIENTED_EDGE('',*,*,#8052,.T.);
#10705=ORIENTED_EDGE('',*,*,#8070,.F.);
#10706=ORIENTED_EDGE('',*,*,#8072,.T.);
#10707=ORIENTED_EDGE('',*,*,#8053,.T.);
#10708=ORIENTED_EDGE('',*,*,#8071,.F.);
#10709=ORIENTED_EDGE('',*,*,#7902,.F.);
#10710=ORIENTED_EDGE('',*,*,#8073,.F.);
#10711=ORIENTED_EDGE('',*,*,#8034,.T.);
#10712=ORIENTED_EDGE('',*,*,#8072,.F.);
#10713=ORIENTED_EDGE('',*,*,#7901,.F.);
#10714=ORIENTED_EDGE('',*,*,#8035,.T.);
#10715=ORIENTED_EDGE('',*,*,#8073,.T.);
#10716=ORIENTED_EDGE('',*,*,#7900,.F.);
#10717=ORIENTED_EDGE('',*,*,#8055,.T.);
#10718=ORIENTED_EDGE('',*,*,#7892,.F.);
#10719=ORIENTED_EDGE('',*,*,#7955,.T.);
#10720=ORIENTED_EDGE('',*,*,#7947,.F.);
#10721=ORIENTED_EDGE('',*,*,#7897,.F.);
#10722=ORIENTED_EDGE('',*,*,#7894,.F.);
#10723=ORIENTED_EDGE('',*,*,#7939,.F.);
#10724=ORIENTED_EDGE('',*,*,#7886,.F.);
#10725=ORIENTED_EDGE('',*,*,#8074,.F.);
#10726=ORIENTED_EDGE('',*,*,#8075,.T.);
#10727=ORIENTED_EDGE('',*,*,#7884,.T.);
#10728=ORIENTED_EDGE('',*,*,#7935,.T.);
#10729=ORIENTED_EDGE('',*,*,#7888,.F.);
#10730=ORIENTED_EDGE('',*,*,#7930,.T.);
#10731=ORIENTED_EDGE('',*,*,#8076,.F.);
#10732=ORIENTED_EDGE('',*,*,#7885,.F.);
#10733=ORIENTED_EDGE('',*,*,#8075,.F.);
#10734=ORIENTED_EDGE('',*,*,#7987,.F.);
#10735=ORIENTED_EDGE('',*,*,#8077,.F.);
#10736=ORIENTED_EDGE('',*,*,#7889,.T.);
#10737=ORIENTED_EDGE('',*,*,#8076,.T.);
#10738=ORIENTED_EDGE('',*,*,#7984,.T.);
#10739=ORIENTED_EDGE('',*,*,#8074,.T.);
#10740=ORIENTED_EDGE('',*,*,#7923,.F.);
#10741=ORIENTED_EDGE('',*,*,#7890,.T.);
#10742=ORIENTED_EDGE('',*,*,#8077,.T.);
#10743=ORIENTED_EDGE('',*,*,#8078,.F.);
#10744=ORIENTED_EDGE('',*,*,#8079,.F.);
#10745=ORIENTED_EDGE('',*,*,#8080,.F.);
#10746=ORIENTED_EDGE('',*,*,#8081,.F.);
#10747=ORIENTED_EDGE('',*,*,#8082,.T.);
#10748=ORIENTED_EDGE('',*,*,#8083,.T.);
#10749=ORIENTED_EDGE('',*,*,#8084,.F.);
#10750=ORIENTED_EDGE('',*,*,#8085,.T.);
#10751=ORIENTED_EDGE('',*,*,#8086,.T.);
#10752=ORIENTED_EDGE('',*,*,#8085,.F.);
#10753=ORIENTED_EDGE('',*,*,#8087,.F.);
#10754=ORIENTED_EDGE('',*,*,#8088,.F.);
#10755=ORIENTED_EDGE('',*,*,#8089,.T.);
#10756=ORIENTED_EDGE('',*,*,#8090,.T.);
#10757=ORIENTED_EDGE('',*,*,#8091,.F.);
#10758=ORIENTED_EDGE('',*,*,#8092,.F.);
#10759=ORIENTED_EDGE('',*,*,#8093,.T.);
#10760=ORIENTED_EDGE('',*,*,#8094,.T.);
#10761=ORIENTED_EDGE('',*,*,#8095,.F.);
#10762=ORIENTED_EDGE('',*,*,#8096,.F.);
#10763=ORIENTED_EDGE('',*,*,#8097,.T.);
#10764=ORIENTED_EDGE('',*,*,#8098,.T.);
#10765=ORIENTED_EDGE('',*,*,#8099,.T.);
#10766=ORIENTED_EDGE('',*,*,#8100,.T.);
#10767=ORIENTED_EDGE('',*,*,#8101,.F.);
#10768=ORIENTED_EDGE('',*,*,#8102,.F.);
#10769=ORIENTED_EDGE('',*,*,#8103,.T.);
#10770=ORIENTED_EDGE('',*,*,#8104,.T.);
#10771=ORIENTED_EDGE('',*,*,#8103,.F.);
#10772=ORIENTED_EDGE('',*,*,#8105,.F.);
#10773=ORIENTED_EDGE('',*,*,#8106,.T.);
#10774=ORIENTED_EDGE('',*,*,#8107,.T.);
#10775=ORIENTED_EDGE('',*,*,#8106,.F.);
#10776=ORIENTED_EDGE('',*,*,#8108,.F.);
#10777=ORIENTED_EDGE('',*,*,#8109,.T.);
#10778=ORIENTED_EDGE('',*,*,#8110,.F.);
#10779=ORIENTED_EDGE('',*,*,#8111,.F.);
#10780=ORIENTED_EDGE('',*,*,#8112,.F.);
#10781=ORIENTED_EDGE('',*,*,#8113,.F.);
#10782=ORIENTED_EDGE('',*,*,#8114,.F.);
#10783=ORIENTED_EDGE('',*,*,#8115,.F.);
#10784=ORIENTED_EDGE('',*,*,#8111,.T.);
#10785=ORIENTED_EDGE('',*,*,#8116,.T.);
#10786=ORIENTED_EDGE('',*,*,#8117,.F.);
#10787=ORIENTED_EDGE('',*,*,#8118,.F.);
#10788=ORIENTED_EDGE('',*,*,#8113,.T.);
#10789=ORIENTED_EDGE('',*,*,#8119,.T.);
#10790=ORIENTED_EDGE('',*,*,#8120,.T.);
#10791=ORIENTED_EDGE('',*,*,#8121,.T.);
#10792=ORIENTED_EDGE('',*,*,#8122,.T.);
#10793=ORIENTED_EDGE('',*,*,#8123,.T.);
#10794=ORIENTED_EDGE('',*,*,#8124,.F.);
#10795=ORIENTED_EDGE('',*,*,#8125,.T.);
#10796=ORIENTED_EDGE('',*,*,#8126,.T.);
#10797=ORIENTED_EDGE('',*,*,#8127,.T.);
#10798=ORIENTED_EDGE('',*,*,#8122,.F.);
#10799=ORIENTED_EDGE('',*,*,#8128,.T.);
#10800=ORIENTED_EDGE('',*,*,#8124,.T.);
#10801=ORIENTED_EDGE('',*,*,#8129,.T.);
#10802=ORIENTED_EDGE('',*,*,#8130,.T.);
#10803=ORIENTED_EDGE('',*,*,#8131,.F.);
#10804=ORIENTED_EDGE('',*,*,#8126,.F.);
#10805=ORIENTED_EDGE('',*,*,#8132,.T.);
#10806=ORIENTED_EDGE('',*,*,#8120,.F.);
#10807=ORIENTED_EDGE('',*,*,#8133,.F.);
#10808=ORIENTED_EDGE('',*,*,#8134,.F.);
#10809=ORIENTED_EDGE('',*,*,#8135,.F.);
#10810=ORIENTED_EDGE('',*,*,#8136,.T.);
#10811=ORIENTED_EDGE('',*,*,#8137,.T.);
#10812=ORIENTED_EDGE('',*,*,#8138,.F.);
#10813=ORIENTED_EDGE('',*,*,#8139,.F.);
#10814=ORIENTED_EDGE('',*,*,#8135,.T.);
#10815=ORIENTED_EDGE('',*,*,#8140,.T.);
#10816=ORIENTED_EDGE('',*,*,#8141,.F.);
#10817=ORIENTED_EDGE('',*,*,#8142,.F.);
#10818=ORIENTED_EDGE('',*,*,#8133,.T.);
#10819=ORIENTED_EDGE('',*,*,#8143,.T.);
#10820=ORIENTED_EDGE('',*,*,#8144,.T.);
#10821=ORIENTED_EDGE('',*,*,#8145,.F.);
#10822=ORIENTED_EDGE('',*,*,#8146,.F.);
#10823=ORIENTED_EDGE('',*,*,#8131,.T.);
#10824=ORIENTED_EDGE('',*,*,#8147,.F.);
#10825=ORIENTED_EDGE('',*,*,#8148,.F.);
#10826=ORIENTED_EDGE('',*,*,#8149,.T.);
#10827=ORIENTED_EDGE('',*,*,#8150,.T.);
#10828=ORIENTED_EDGE('',*,*,#8151,.T.);
#10829=ORIENTED_EDGE('',*,*,#8152,.F.);
#10830=ORIENTED_EDGE('',*,*,#8153,.F.);
#10831=ORIENTED_EDGE('',*,*,#8154,.F.);
#10832=ORIENTED_EDGE('',*,*,#8145,.T.);
#10833=ORIENTED_EDGE('',*,*,#8155,.T.);
#10834=ORIENTED_EDGE('',*,*,#8156,.T.);
#10835=ORIENTED_EDGE('',*,*,#8157,.T.);
#10836=ORIENTED_EDGE('',*,*,#8158,.T.);
#10837=ORIENTED_EDGE('',*,*,#8159,.T.);
#10838=ORIENTED_EDGE('',*,*,#8160,.T.);
#10839=ORIENTED_EDGE('',*,*,#8161,.F.);
#10840=ORIENTED_EDGE('',*,*,#8162,.F.);
#10841=ORIENTED_EDGE('',*,*,#8163,.T.);
#10842=ORIENTED_EDGE('',*,*,#8164,.F.);
#10843=ORIENTED_EDGE('',*,*,#8165,.T.);
#10844=ORIENTED_EDGE('',*,*,#8166,.T.);
#10845=ORIENTED_EDGE('',*,*,#8167,.T.);
#10846=ORIENTED_EDGE('',*,*,#8166,.F.);
#10847=ORIENTED_EDGE('',*,*,#8168,.T.);
#10848=ORIENTED_EDGE('',*,*,#8169,.T.);
#10849=ORIENTED_EDGE('',*,*,#8170,.T.);
#10850=ORIENTED_EDGE('',*,*,#8171,.F.);
#10851=ORIENTED_EDGE('',*,*,#8172,.T.);
#10852=ORIENTED_EDGE('',*,*,#8173,.T.);
#10853=ORIENTED_EDGE('',*,*,#8174,.T.);
#10854=ORIENTED_EDGE('',*,*,#8175,.F.);
#10855=ORIENTED_EDGE('',*,*,#8176,.T.);
#10856=ORIENTED_EDGE('',*,*,#8177,.T.);
#10857=ORIENTED_EDGE('',*,*,#8178,.T.);
#10858=ORIENTED_EDGE('',*,*,#8173,.F.);
#10859=ORIENTED_EDGE('',*,*,#8179,.T.);
#10860=ORIENTED_EDGE('',*,*,#8180,.F.);
#10861=ORIENTED_EDGE('',*,*,#8168,.F.);
#10862=ORIENTED_EDGE('',*,*,#8165,.F.);
#10863=ORIENTED_EDGE('',*,*,#8181,.F.);
#10864=ORIENTED_EDGE('',*,*,#8163,.F.);
#10865=ORIENTED_EDGE('',*,*,#8182,.F.);
#10866=ORIENTED_EDGE('',*,*,#8183,.F.);
#10867=ORIENTED_EDGE('',*,*,#8184,.F.);
#10868=ORIENTED_EDGE('',*,*,#8164,.T.);
#10869=ORIENTED_EDGE('',*,*,#8184,.T.);
#10870=ORIENTED_EDGE('',*,*,#8185,.T.);
#10871=ORIENTED_EDGE('',*,*,#8181,.T.);
#10872=ORIENTED_EDGE('',*,*,#8179,.F.);
#10873=ORIENTED_EDGE('',*,*,#8172,.F.);
#10874=ORIENTED_EDGE('',*,*,#8186,.F.);
#10875=ORIENTED_EDGE('',*,*,#8187,.F.);
#10876=ORIENTED_EDGE('',*,*,#8188,.F.);
#10877=ORIENTED_EDGE('',*,*,#8189,.F.);
#10878=ORIENTED_EDGE('',*,*,#8176,.F.);
#10879=ORIENTED_EDGE('',*,*,#8190,.F.);
#10880=ORIENTED_EDGE('',*,*,#8108,.T.);
#10881=ORIENTED_EDGE('',*,*,#8105,.T.);
#10882=ORIENTED_EDGE('',*,*,#8102,.T.);
#10883=ORIENTED_EDGE('',*,*,#8191,.T.);
#10884=ORIENTED_EDGE('',*,*,#8192,.F.);
#10885=ORIENTED_EDGE('',*,*,#8193,.F.);
#10886=ORIENTED_EDGE('',*,*,#8194,.F.);
#10887=ORIENTED_EDGE('',*,*,#8195,.F.);
#10888=ORIENTED_EDGE('',*,*,#8194,.T.);
#10889=ORIENTED_EDGE('',*,*,#8196,.F.);
#10890=ORIENTED_EDGE('',*,*,#8197,.F.);
#10891=ORIENTED_EDGE('',*,*,#8198,.F.);
#10892=ORIENTED_EDGE('',*,*,#8192,.T.);
#10893=ORIENTED_EDGE('',*,*,#8199,.F.);
#10894=ORIENTED_EDGE('',*,*,#8200,.F.);
#10895=ORIENTED_EDGE('',*,*,#8201,.F.);
#10896=ORIENTED_EDGE('',*,*,#8197,.T.);
#10897=ORIENTED_EDGE('',*,*,#8202,.F.);
#10898=ORIENTED_EDGE('',*,*,#8203,.F.);
#10899=ORIENTED_EDGE('',*,*,#8204,.F.);
#10900=ORIENTED_EDGE('',*,*,#8200,.T.);
#10901=ORIENTED_EDGE('',*,*,#8205,.F.);
#10902=ORIENTED_EDGE('',*,*,#8206,.F.);
#10903=ORIENTED_EDGE('',*,*,#8207,.F.);
#10904=ORIENTED_EDGE('',*,*,#8203,.T.);
#10905=ORIENTED_EDGE('',*,*,#8208,.F.);
#10906=ORIENTED_EDGE('',*,*,#8209,.F.);
#10907=ORIENTED_EDGE('',*,*,#8210,.F.);
#10908=ORIENTED_EDGE('',*,*,#8206,.T.);
#10909=ORIENTED_EDGE('',*,*,#8211,.F.);
#10910=ORIENTED_EDGE('',*,*,#8212,.F.);
#10911=ORIENTED_EDGE('',*,*,#8213,.F.);
#10912=ORIENTED_EDGE('',*,*,#8177,.F.);
#10913=ORIENTED_EDGE('',*,*,#8189,.T.);
#10914=ORIENTED_EDGE('',*,*,#8214,.T.);
#10915=ORIENTED_EDGE('',*,*,#8215,.T.);
#10916=ORIENTED_EDGE('',*,*,#8209,.T.);
#10917=ORIENTED_EDGE('',*,*,#8216,.F.);
#10918=ORIENTED_EDGE('',*,*,#8212,.T.);
#10919=ORIENTED_EDGE('',*,*,#8217,.F.);
#10920=ORIENTED_EDGE('',*,*,#8218,.F.);
#10921=ORIENTED_EDGE('',*,*,#8116,.F.);
#10922=ORIENTED_EDGE('',*,*,#8110,.T.);
#10923=ORIENTED_EDGE('',*,*,#8118,.T.);
#10924=ORIENTED_EDGE('',*,*,#8130,.F.);
#10925=ORIENTED_EDGE('',*,*,#8219,.T.);
#10926=ORIENTED_EDGE('',*,*,#8136,.F.);
#10927=ORIENTED_EDGE('',*,*,#8220,.F.);
#10928=ORIENTED_EDGE('',*,*,#8137,.F.);
#10929=ORIENTED_EDGE('',*,*,#8219,.F.);
#10930=ORIENTED_EDGE('',*,*,#8129,.F.);
#10931=ORIENTED_EDGE('',*,*,#8127,.F.);
#10932=ORIENTED_EDGE('',*,*,#8132,.F.);
#10933=ORIENTED_EDGE('',*,*,#8125,.F.);
#10934=ORIENTED_EDGE('',*,*,#8128,.F.);
#10935=ORIENTED_EDGE('',*,*,#8121,.F.);
#10936=ORIENTED_EDGE('',*,*,#8221,.F.);
#10937=ORIENTED_EDGE('',*,*,#8222,.F.);
#10938=ORIENTED_EDGE('',*,*,#8223,.T.);
#10939=ORIENTED_EDGE('',*,*,#8224,.T.);
#10940=ORIENTED_EDGE('',*,*,#8225,.T.);
#10941=ORIENTED_EDGE('',*,*,#8096,.T.);
#10942=ORIENTED_EDGE('',*,*,#8226,.F.);
#10943=ORIENTED_EDGE('',*,*,#8099,.F.);
#10944=ORIENTED_EDGE('',*,*,#8227,.T.);
#10945=ORIENTED_EDGE('',*,*,#8228,.T.);
#10946=ORIENTED_EDGE('',*,*,#8229,.F.);
#10947=ORIENTED_EDGE('',*,*,#8228,.F.);
#10948=ORIENTED_EDGE('',*,*,#8230,.T.);
#10949=ORIENTED_EDGE('',*,*,#8231,.T.);
#10950=ORIENTED_EDGE('',*,*,#8232,.F.);
#10951=ORIENTED_EDGE('',*,*,#8231,.F.);
#10952=ORIENTED_EDGE('',*,*,#8233,.T.);
#10953=ORIENTED_EDGE('',*,*,#8234,.T.);
#10954=ORIENTED_EDGE('',*,*,#8235,.T.);
#10955=ORIENTED_EDGE('',*,*,#8236,.F.);
#10956=ORIENTED_EDGE('',*,*,#8235,.F.);
#10957=ORIENTED_EDGE('',*,*,#8237,.T.);
#10958=ORIENTED_EDGE('',*,*,#8238,.T.);
#10959=ORIENTED_EDGE('',*,*,#8239,.F.);
#10960=ORIENTED_EDGE('',*,*,#8240,.F.);
#10961=ORIENTED_EDGE('',*,*,#8241,.T.);
#10962=ORIENTED_EDGE('',*,*,#8222,.T.);
#10963=ORIENTED_EDGE('',*,*,#8242,.F.);
#10964=ORIENTED_EDGE('',*,*,#8238,.F.);
#10965=ORIENTED_EDGE('',*,*,#8243,.T.);
#10966=ORIENTED_EDGE('',*,*,#8240,.T.);
#10967=ORIENTED_EDGE('',*,*,#8244,.F.);
#10968=ORIENTED_EDGE('',*,*,#8245,.F.);
#10969=ORIENTED_EDGE('',*,*,#8246,.T.);
#10970=ORIENTED_EDGE('',*,*,#8092,.T.);
#10971=ORIENTED_EDGE('',*,*,#8247,.F.);
#10972=ORIENTED_EDGE('',*,*,#8094,.F.);
#10973=ORIENTED_EDGE('',*,*,#8248,.T.);
#10974=ORIENTED_EDGE('',*,*,#8249,.T.);
#10975=ORIENTED_EDGE('',*,*,#8250,.F.);
#10976=ORIENTED_EDGE('',*,*,#8249,.F.);
#10977=ORIENTED_EDGE('',*,*,#8251,.T.);
#10978=ORIENTED_EDGE('',*,*,#8252,.T.);
#10979=ORIENTED_EDGE('',*,*,#8253,.F.);
#10980=ORIENTED_EDGE('',*,*,#8252,.F.);
#10981=ORIENTED_EDGE('',*,*,#8254,.T.);
#10982=ORIENTED_EDGE('',*,*,#8088,.T.);
#10983=ORIENTED_EDGE('',*,*,#8255,.F.);
#10984=ORIENTED_EDGE('',*,*,#8090,.F.);
#10985=ORIENTED_EDGE('',*,*,#8256,.T.);
#10986=ORIENTED_EDGE('',*,*,#8257,.T.);
#10987=ORIENTED_EDGE('',*,*,#8078,.T.);
#10988=ORIENTED_EDGE('',*,*,#8258,.T.);
#10989=ORIENTED_EDGE('',*,*,#8097,.F.);
#10990=ORIENTED_EDGE('',*,*,#8225,.F.);
#10991=ORIENTED_EDGE('',*,*,#8239,.T.);
#10992=ORIENTED_EDGE('',*,*,#8221,.T.);
#10993=ORIENTED_EDGE('',*,*,#8095,.T.);
#10994=ORIENTED_EDGE('',*,*,#8226,.T.);
#10995=ORIENTED_EDGE('',*,*,#8229,.T.);
#10996=ORIENTED_EDGE('',*,*,#8232,.T.);
#10997=ORIENTED_EDGE('',*,*,#8236,.T.);
#10998=ORIENTED_EDGE('',*,*,#8242,.T.);
#10999=ORIENTED_EDGE('',*,*,#8259,.T.);
#11000=ORIENTED_EDGE('',*,*,#8244,.T.);
#11001=ORIENTED_EDGE('',*,*,#8091,.T.);
#11002=ORIENTED_EDGE('',*,*,#8247,.T.);
#11003=ORIENTED_EDGE('',*,*,#8250,.T.);
#11004=ORIENTED_EDGE('',*,*,#8253,.T.);
#11005=ORIENTED_EDGE('',*,*,#8087,.T.);
#11006=ORIENTED_EDGE('',*,*,#8255,.T.);
#11007=ORIENTED_EDGE('',*,*,#8246,.F.);
#11008=ORIENTED_EDGE('',*,*,#8260,.F.);
#11009=ORIENTED_EDGE('',*,*,#8256,.F.);
#11010=ORIENTED_EDGE('',*,*,#8089,.F.);
#11011=ORIENTED_EDGE('',*,*,#8254,.F.);
#11012=ORIENTED_EDGE('',*,*,#8251,.F.);
#11013=ORIENTED_EDGE('',*,*,#8248,.F.);
#11014=ORIENTED_EDGE('',*,*,#8093,.F.);
#11015=ORIENTED_EDGE('',*,*,#8084,.T.);
#11016=ORIENTED_EDGE('',*,*,#8259,.F.);
#11017=ORIENTED_EDGE('',*,*,#8257,.F.);
#11018=ORIENTED_EDGE('',*,*,#8260,.T.);
#11019=ORIENTED_EDGE('',*,*,#8245,.T.);
#11020=ORIENTED_EDGE('',*,*,#8261,.F.);
#11021=ORIENTED_EDGE('',*,*,#8262,.T.);
#11022=ORIENTED_EDGE('',*,*,#8263,.T.);
#11023=ORIENTED_EDGE('',*,*,#8264,.T.);
#11024=ORIENTED_EDGE('',*,*,#8265,.T.);
#11025=ORIENTED_EDGE('',*,*,#8234,.F.);
#11026=ORIENTED_EDGE('',*,*,#8266,.T.);
#11027=ORIENTED_EDGE('',*,*,#8080,.T.);
#11028=ORIENTED_EDGE('',*,*,#8223,.F.);
#11029=ORIENTED_EDGE('',*,*,#8241,.F.);
#11030=ORIENTED_EDGE('',*,*,#8243,.F.);
#11031=ORIENTED_EDGE('',*,*,#8237,.F.);
#11032=ORIENTED_EDGE('',*,*,#8086,.F.);
#11033=ORIENTED_EDGE('',*,*,#8267,.F.);
#11034=ORIENTED_EDGE('',*,*,#8268,.F.);
#11035=ORIENTED_EDGE('',*,*,#8269,.F.);
#11036=ORIENTED_EDGE('',*,*,#8270,.F.);
#11037=ORIENTED_EDGE('',*,*,#8258,.F.);
#11038=ORIENTED_EDGE('',*,*,#8083,.F.);
#11039=ORIENTED_EDGE('',*,*,#8271,.T.);
#11040=ORIENTED_EDGE('',*,*,#8272,.T.);
#11041=ORIENTED_EDGE('',*,*,#8224,.F.);
#11042=ORIENTED_EDGE('',*,*,#8079,.T.);
#11043=ORIENTED_EDGE('',*,*,#8273,.T.);
#11044=ORIENTED_EDGE('',*,*,#8274,.T.);
#11045=ORIENTED_EDGE('',*,*,#8275,.F.);
#11046=ORIENTED_EDGE('',*,*,#8276,.T.);
#11047=ORIENTED_EDGE('',*,*,#8272,.F.);
#11048=ORIENTED_EDGE('',*,*,#8277,.T.);
#11049=ORIENTED_EDGE('',*,*,#8278,.T.);
#11050=ORIENTED_EDGE('',*,*,#8279,.T.);
#11051=ORIENTED_EDGE('',*,*,#8160,.F.);
#11052=ORIENTED_EDGE('',*,*,#8280,.T.);
#11053=ORIENTED_EDGE('',*,*,#8081,.T.);
#11054=ORIENTED_EDGE('',*,*,#8266,.F.);
#11055=ORIENTED_EDGE('',*,*,#8281,.F.);
#11056=ORIENTED_EDGE('',*,*,#8282,.T.);
#11057=ORIENTED_EDGE('',*,*,#8283,.F.);
#11058=ORIENTED_EDGE('',*,*,#8284,.F.);
#11059=ORIENTED_EDGE('',*,*,#8285,.T.);
#11060=ORIENTED_EDGE('',*,*,#8286,.F.);
#11061=ORIENTED_EDGE('',*,*,#8287,.T.);
#11062=ORIENTED_EDGE('',*,*,#8288,.T.);
#11063=ORIENTED_EDGE('',*,*,#8261,.T.);
#11064=ORIENTED_EDGE('',*,*,#8289,.T.);
#11065=ORIENTED_EDGE('',*,*,#8290,.T.);
#11066=ORIENTED_EDGE('',*,*,#8281,.T.);
#11067=ORIENTED_EDGE('',*,*,#8233,.F.);
#11068=ORIENTED_EDGE('',*,*,#8230,.F.);
#11069=ORIENTED_EDGE('',*,*,#8227,.F.);
#11070=ORIENTED_EDGE('',*,*,#8098,.F.);
#11071=ORIENTED_EDGE('',*,*,#8270,.T.);
#11072=ORIENTED_EDGE('',*,*,#8271,.F.);
#11073=ORIENTED_EDGE('',*,*,#8082,.F.);
#11074=ORIENTED_EDGE('',*,*,#8280,.F.);
#11075=ORIENTED_EDGE('',*,*,#8159,.F.);
#11076=ORIENTED_EDGE('',*,*,#8291,.F.);
#11077=ORIENTED_EDGE('',*,*,#8292,.F.);
#11078=ORIENTED_EDGE('',*,*,#8293,.F.);
#11079=ORIENTED_EDGE('',*,*,#8277,.F.);
#11080=ORIENTED_EDGE('',*,*,#8278,.F.);
#11081=ORIENTED_EDGE('',*,*,#8294,.F.);
#11082=ORIENTED_EDGE('',*,*,#8295,.T.);
#11083=ORIENTED_EDGE('',*,*,#8296,.T.);
#11084=ORIENTED_EDGE('',*,*,#8279,.F.);
#11085=ORIENTED_EDGE('',*,*,#8296,.F.);
#11086=ORIENTED_EDGE('',*,*,#8297,.T.);
#11087=ORIENTED_EDGE('',*,*,#8161,.T.);
#11088=ORIENTED_EDGE('',*,*,#8282,.F.);
#11089=ORIENTED_EDGE('',*,*,#8290,.F.);
#11090=ORIENTED_EDGE('',*,*,#8298,.T.);
#11091=ORIENTED_EDGE('',*,*,#8294,.T.);
#11092=ORIENTED_EDGE('',*,*,#8295,.F.);
#11093=ORIENTED_EDGE('',*,*,#8298,.F.);
#11094=ORIENTED_EDGE('',*,*,#8289,.F.);
#11095=ORIENTED_EDGE('',*,*,#8265,.F.);
#11096=ORIENTED_EDGE('',*,*,#8299,.F.);
#11097=ORIENTED_EDGE('',*,*,#8156,.F.);
#11098=ORIENTED_EDGE('',*,*,#8297,.F.);
#11099=ORIENTED_EDGE('',*,*,#8268,.T.);
#11100=ORIENTED_EDGE('',*,*,#8300,.F.);
#11101=ORIENTED_EDGE('',*,*,#8301,.F.);
#11102=ORIENTED_EDGE('',*,*,#8302,.T.);
#11103=ORIENTED_EDGE('',*,*,#8267,.T.);
#11104=ORIENTED_EDGE('',*,*,#8276,.F.);
#11105=ORIENTED_EDGE('',*,*,#8303,.F.);
#11106=ORIENTED_EDGE('',*,*,#8300,.T.);
#11107=ORIENTED_EDGE('',*,*,#8269,.T.);
#11108=ORIENTED_EDGE('',*,*,#8302,.F.);
#11109=ORIENTED_EDGE('',*,*,#8304,.F.);
#11110=ORIENTED_EDGE('',*,*,#8283,.T.);
#11111=ORIENTED_EDGE('',*,*,#8301,.T.);
#11112=ORIENTED_EDGE('',*,*,#8303,.T.);
#11113=ORIENTED_EDGE('',*,*,#8275,.T.);
#11114=ORIENTED_EDGE('',*,*,#8305,.T.);
#11115=ORIENTED_EDGE('',*,*,#8306,.T.);
#11116=ORIENTED_EDGE('',*,*,#8284,.T.);
#11117=ORIENTED_EDGE('',*,*,#8304,.T.);
#11118=ORIENTED_EDGE('',*,*,#8274,.F.);
#11119=ORIENTED_EDGE('',*,*,#8307,.F.);
#11120=ORIENTED_EDGE('',*,*,#8308,.T.);
#11121=ORIENTED_EDGE('',*,*,#8309,.T.);
#11122=ORIENTED_EDGE('',*,*,#8310,.F.);
#11123=ORIENTED_EDGE('',*,*,#8311,.F.);
#11124=ORIENTED_EDGE('',*,*,#8309,.F.);
#11125=ORIENTED_EDGE('',*,*,#8312,.T.);
#11126=ORIENTED_EDGE('',*,*,#8313,.T.);
#11127=ORIENTED_EDGE('',*,*,#8314,.F.);
#11128=ORIENTED_EDGE('',*,*,#8313,.F.);
#11129=ORIENTED_EDGE('',*,*,#8315,.T.);
#11130=ORIENTED_EDGE('',*,*,#8316,.T.);
#11131=ORIENTED_EDGE('',*,*,#8317,.F.);
#11132=ORIENTED_EDGE('',*,*,#8318,.F.);
#11133=ORIENTED_EDGE('',*,*,#8316,.F.);
#11134=ORIENTED_EDGE('',*,*,#8319,.T.);
#11135=ORIENTED_EDGE('',*,*,#8320,.T.);
#11136=ORIENTED_EDGE('',*,*,#8321,.F.);
#11137=ORIENTED_EDGE('',*,*,#8320,.F.);
#11138=ORIENTED_EDGE('',*,*,#8322,.T.);
#11139=ORIENTED_EDGE('',*,*,#8286,.T.);
#11140=ORIENTED_EDGE('',*,*,#8262,.F.);
#11141=ORIENTED_EDGE('',*,*,#8288,.F.);
#11142=ORIENTED_EDGE('',*,*,#8323,.T.);
#11143=ORIENTED_EDGE('',*,*,#8324,.T.);
#11144=ORIENTED_EDGE('',*,*,#8263,.F.);
#11145=ORIENTED_EDGE('',*,*,#8324,.F.);
#11146=ORIENTED_EDGE('',*,*,#8325,.T.);
#11147=ORIENTED_EDGE('',*,*,#8326,.T.);
#11148=ORIENTED_EDGE('',*,*,#8264,.F.);
#11149=ORIENTED_EDGE('',*,*,#8326,.F.);
#11150=ORIENTED_EDGE('',*,*,#8327,.T.);
#11151=ORIENTED_EDGE('',*,*,#8328,.T.);
#11152=ORIENTED_EDGE('',*,*,#8329,.F.);
#11153=ORIENTED_EDGE('',*,*,#8330,.F.);
#11154=ORIENTED_EDGE('',*,*,#8328,.F.);
#11155=ORIENTED_EDGE('',*,*,#8331,.T.);
#11156=ORIENTED_EDGE('',*,*,#8332,.T.);
#11157=ORIENTED_EDGE('',*,*,#8333,.F.);
#11158=ORIENTED_EDGE('',*,*,#8332,.F.);
#11159=ORIENTED_EDGE('',*,*,#8334,.T.);
#11160=ORIENTED_EDGE('',*,*,#8335,.T.);
#11161=ORIENTED_EDGE('',*,*,#8157,.F.);
#11162=ORIENTED_EDGE('',*,*,#8151,.F.);
#11163=ORIENTED_EDGE('',*,*,#8336,.T.);
#11164=ORIENTED_EDGE('',*,*,#8337,.F.);
#11165=ORIENTED_EDGE('',*,*,#8158,.F.);
#11166=ORIENTED_EDGE('',*,*,#8335,.F.);
#11167=ORIENTED_EDGE('',*,*,#8338,.T.);
#11168=ORIENTED_EDGE('',*,*,#8339,.T.);
#11169=ORIENTED_EDGE('',*,*,#8138,.T.);
#11170=ORIENTED_EDGE('',*,*,#8340,.T.);
#11171=ORIENTED_EDGE('',*,*,#8341,.T.);
#11172=ORIENTED_EDGE('',*,*,#8342,.T.);
#11173=ORIENTED_EDGE('',*,*,#8293,.T.);
#11174=ORIENTED_EDGE('',*,*,#8343,.T.);
#11175=ORIENTED_EDGE('',*,*,#8344,.T.);
#11176=ORIENTED_EDGE('',*,*,#8155,.F.);
#11177=ORIENTED_EDGE('',*,*,#8144,.F.);
#11178=ORIENTED_EDGE('',*,*,#8345,.T.);
#11179=ORIENTED_EDGE('',*,*,#8346,.F.);
#11180=ORIENTED_EDGE('',*,*,#8336,.F.);
#11181=ORIENTED_EDGE('',*,*,#8347,.F.);
#11182=ORIENTED_EDGE('',*,*,#8348,.T.);
#11183=ORIENTED_EDGE('',*,*,#8341,.F.);
#11184=ORIENTED_EDGE('',*,*,#8349,.F.);
#11185=ORIENTED_EDGE('',*,*,#8149,.F.);
#11186=ORIENTED_EDGE('',*,*,#8305,.F.);
#11187=ORIENTED_EDGE('',*,*,#8310,.T.);
#11188=ORIENTED_EDGE('',*,*,#8311,.T.);
#11189=ORIENTED_EDGE('',*,*,#8314,.T.);
#11190=ORIENTED_EDGE('',*,*,#8350,.T.);
#11191=ORIENTED_EDGE('',*,*,#8141,.T.);
#11192=ORIENTED_EDGE('',*,*,#8351,.T.);
#11193=ORIENTED_EDGE('',*,*,#8352,.T.);
#11194=ORIENTED_EDGE('',*,*,#8353,.T.);
#11195=ORIENTED_EDGE('',*,*,#8291,.T.);
#11196=ORIENTED_EDGE('',*,*,#8337,.T.);
#11197=ORIENTED_EDGE('',*,*,#8346,.T.);
#11198=ORIENTED_EDGE('',*,*,#8354,.F.);
#11199=ORIENTED_EDGE('',*,*,#8355,.T.);
#11200=ORIENTED_EDGE('',*,*,#8307,.T.);
#11201=ORIENTED_EDGE('',*,*,#8273,.F.);
#11202=ORIENTED_EDGE('',*,*,#8342,.F.);
#11203=ORIENTED_EDGE('',*,*,#8348,.F.);
#11204=ORIENTED_EDGE('',*,*,#8355,.F.);
#11205=ORIENTED_EDGE('',*,*,#8356,.T.);
#11206=ORIENTED_EDGE('',*,*,#8357,.F.);
#11207=ORIENTED_EDGE('',*,*,#8358,.F.);
#11208=ORIENTED_EDGE('',*,*,#8359,.F.);
#11209=ORIENTED_EDGE('',*,*,#8152,.T.);
#11210=ORIENTED_EDGE('',*,*,#8338,.F.);
#11211=ORIENTED_EDGE('',*,*,#8334,.F.);
#11212=ORIENTED_EDGE('',*,*,#8331,.F.);
#11213=ORIENTED_EDGE('',*,*,#8327,.F.);
#11214=ORIENTED_EDGE('',*,*,#8325,.F.);
#11215=ORIENTED_EDGE('',*,*,#8323,.F.);
#11216=ORIENTED_EDGE('',*,*,#8287,.F.);
#11217=ORIENTED_EDGE('',*,*,#8322,.F.);
#11218=ORIENTED_EDGE('',*,*,#8319,.F.);
#11219=ORIENTED_EDGE('',*,*,#8315,.F.);
#11220=ORIENTED_EDGE('',*,*,#8312,.F.);
#11221=ORIENTED_EDGE('',*,*,#8308,.F.);
#11222=ORIENTED_EDGE('',*,*,#8213,.T.);
#11223=ORIENTED_EDGE('',*,*,#8216,.T.);
#11224=ORIENTED_EDGE('',*,*,#8208,.T.);
#11225=ORIENTED_EDGE('',*,*,#8202,.T.);
#11226=ORIENTED_EDGE('',*,*,#8196,.T.);
#11227=ORIENTED_EDGE('',*,*,#8193,.T.);
#11228=ORIENTED_EDGE('',*,*,#8201,.T.);
#11229=ORIENTED_EDGE('',*,*,#8207,.T.);
#11230=ORIENTED_EDGE('',*,*,#8134,.T.);
#11231=ORIENTED_EDGE('',*,*,#8142,.T.);
#11232=ORIENTED_EDGE('',*,*,#8350,.F.);
#11233=ORIENTED_EDGE('',*,*,#8345,.F.);
#11234=ORIENTED_EDGE('',*,*,#8150,.F.);
#11235=ORIENTED_EDGE('',*,*,#8349,.T.);
#11236=ORIENTED_EDGE('',*,*,#8340,.F.);
#11237=ORIENTED_EDGE('',*,*,#8140,.F.);
#11238=ORIENTED_EDGE('',*,*,#8306,.F.);
#11239=ORIENTED_EDGE('',*,*,#8317,.T.);
#11240=ORIENTED_EDGE('',*,*,#8318,.T.);
#11241=ORIENTED_EDGE('',*,*,#8321,.T.);
#11242=ORIENTED_EDGE('',*,*,#8285,.F.);
#11243=ORIENTED_EDGE('',*,*,#8147,.T.);
#11244=ORIENTED_EDGE('',*,*,#8220,.T.);
#11245=ORIENTED_EDGE('',*,*,#8139,.T.);
#11246=ORIENTED_EDGE('',*,*,#8339,.F.);
#11247=ORIENTED_EDGE('',*,*,#8360,.T.);
#11248=ORIENTED_EDGE('',*,*,#8361,.T.);
#11249=ORIENTED_EDGE('',*,*,#8362,.T.);
#11250=ORIENTED_EDGE('',*,*,#8360,.F.);
#11251=ORIENTED_EDGE('',*,*,#8344,.F.);
#11252=ORIENTED_EDGE('',*,*,#8363,.T.);
#11253=ORIENTED_EDGE('',*,*,#8154,.T.);
#11254=ORIENTED_EDGE('',*,*,#8364,.F.);
#11255=ORIENTED_EDGE('',*,*,#8352,.F.);
#11256=ORIENTED_EDGE('',*,*,#8364,.T.);
#11257=ORIENTED_EDGE('',*,*,#8153,.T.);
#11258=ORIENTED_EDGE('',*,*,#8359,.T.);
#11259=ORIENTED_EDGE('',*,*,#8365,.F.);
#11260=ORIENTED_EDGE('',*,*,#8366,.F.);
#11261=ORIENTED_EDGE('',*,*,#8353,.F.);
#11262=ORIENTED_EDGE('',*,*,#8333,.T.);
#11263=ORIENTED_EDGE('',*,*,#8299,.T.);
#11264=ORIENTED_EDGE('',*,*,#8329,.T.);
#11265=ORIENTED_EDGE('',*,*,#8330,.T.);
#11266=ORIENTED_EDGE('',*,*,#8357,.T.);
#11267=ORIENTED_EDGE('',*,*,#8367,.T.);
#11268=ORIENTED_EDGE('',*,*,#8361,.F.);
#11269=ORIENTED_EDGE('',*,*,#8343,.F.);
#11270=ORIENTED_EDGE('',*,*,#8368,.F.);
#11271=ORIENTED_EDGE('',*,*,#8369,.T.);
#11272=ORIENTED_EDGE('',*,*,#8292,.T.);
#11273=ORIENTED_EDGE('',*,*,#8366,.T.);
#11274=ORIENTED_EDGE('',*,*,#8370,.T.);
#11275=ORIENTED_EDGE('',*,*,#8368,.T.);
#11276=ORIENTED_EDGE('',*,*,#8358,.T.);
#11277=ORIENTED_EDGE('',*,*,#8369,.F.);
#11278=ORIENTED_EDGE('',*,*,#8370,.F.);
#11279=ORIENTED_EDGE('',*,*,#8365,.T.);
#11280=ORIENTED_EDGE('',*,*,#8371,.T.);
#11281=ORIENTED_EDGE('',*,*,#8198,.T.);
#11282=ORIENTED_EDGE('',*,*,#8372,.F.);
#11283=ORIENTED_EDGE('',*,*,#8373,.F.);
#11284=ORIENTED_EDGE('',*,*,#8372,.T.);
#11285=ORIENTED_EDGE('',*,*,#8204,.T.);
#11286=ORIENTED_EDGE('',*,*,#8374,.F.);
#11287=ORIENTED_EDGE('',*,*,#8375,.F.);
#11288=ORIENTED_EDGE('',*,*,#8374,.T.);
#11289=ORIENTED_EDGE('',*,*,#8210,.T.);
#11290=ORIENTED_EDGE('',*,*,#8376,.F.);
#11291=ORIENTED_EDGE('',*,*,#8377,.F.);
#11292=ORIENTED_EDGE('',*,*,#8376,.T.);
#11293=ORIENTED_EDGE('',*,*,#8217,.T.);
#11294=ORIENTED_EDGE('',*,*,#8378,.F.);
#11295=ORIENTED_EDGE('',*,*,#8379,.F.);
#11296=ORIENTED_EDGE('',*,*,#8378,.T.);
#11297=ORIENTED_EDGE('',*,*,#8211,.T.);
#11298=ORIENTED_EDGE('',*,*,#8380,.F.);
#11299=ORIENTED_EDGE('',*,*,#8381,.F.);
#11300=ORIENTED_EDGE('',*,*,#8380,.T.);
#11301=ORIENTED_EDGE('',*,*,#8205,.T.);
#11302=ORIENTED_EDGE('',*,*,#8382,.F.);
#11303=ORIENTED_EDGE('',*,*,#8383,.F.);
#11304=ORIENTED_EDGE('',*,*,#8384,.T.);
#11305=ORIENTED_EDGE('',*,*,#8195,.T.);
#11306=ORIENTED_EDGE('',*,*,#8371,.F.);
#11307=ORIENTED_EDGE('',*,*,#8385,.F.);
#11308=ORIENTED_EDGE('',*,*,#8347,.T.);
#11309=ORIENTED_EDGE('',*,*,#8148,.T.);
#11310=ORIENTED_EDGE('',*,*,#8362,.F.);
#11311=ORIENTED_EDGE('',*,*,#8367,.F.);
#11312=ORIENTED_EDGE('',*,*,#8356,.F.);
#11313=ORIENTED_EDGE('',*,*,#8354,.T.);
#11314=ORIENTED_EDGE('',*,*,#8123,.F.);
#11315=ORIENTED_EDGE('',*,*,#8146,.T.);
#11316=ORIENTED_EDGE('',*,*,#8363,.F.);
#11317=ORIENTED_EDGE('',*,*,#8351,.F.);
#11318=ORIENTED_EDGE('',*,*,#8143,.F.);
#11319=ORIENTED_EDGE('',*,*,#8382,.T.);
#11320=ORIENTED_EDGE('',*,*,#8199,.T.);
#11321=ORIENTED_EDGE('',*,*,#8384,.F.);
#11322=ORIENTED_EDGE('',*,*,#8386,.F.);
#11323=ORIENTED_EDGE('',*,*,#8119,.F.);
#11324=ORIENTED_EDGE('',*,*,#8112,.T.);
#11325=ORIENTED_EDGE('',*,*,#8115,.T.);
#11326=ORIENTED_EDGE('',*,*,#8387,.F.);
#11327=ORIENTED_EDGE('',*,*,#8109,.F.);
#11328=ORIENTED_EDGE('',*,*,#8191,.F.);
#11329=ORIENTED_EDGE('',*,*,#8101,.T.);
#11330=ORIENTED_EDGE('',*,*,#8388,.F.);
#11331=ORIENTED_EDGE('',*,*,#8214,.F.);
#11332=ORIENTED_EDGE('',*,*,#8188,.T.);
#11333=ORIENTED_EDGE('',*,*,#8389,.F.);
#11334=ORIENTED_EDGE('',*,*,#8186,.T.);
#11335=ORIENTED_EDGE('',*,*,#8171,.T.);
#11336=ORIENTED_EDGE('',*,*,#8390,.T.);
#11337=ORIENTED_EDGE('',*,*,#8389,.T.);
#11338=ORIENTED_EDGE('',*,*,#8190,.T.);
#11339=ORIENTED_EDGE('',*,*,#8175,.T.);
#11340=ORIENTED_EDGE('',*,*,#8187,.T.);
#11341=ORIENTED_EDGE('',*,*,#8391,.F.);
#11342=ORIENTED_EDGE('',*,*,#8392,.T.);
#11343=ORIENTED_EDGE('',*,*,#8393,.T.);
#11344=ORIENTED_EDGE('',*,*,#8394,.T.);
#11345=ORIENTED_EDGE('',*,*,#8395,.F.);
#11346=ORIENTED_EDGE('',*,*,#8396,.T.);
#11347=ORIENTED_EDGE('',*,*,#8397,.T.);
#11348=ORIENTED_EDGE('',*,*,#8398,.T.);
#11349=ORIENTED_EDGE('',*,*,#8399,.F.);
#11350=ORIENTED_EDGE('',*,*,#8400,.T.);
#11351=ORIENTED_EDGE('',*,*,#8395,.T.);
#11352=ORIENTED_EDGE('',*,*,#8401,.T.);
#11353=ORIENTED_EDGE('',*,*,#8393,.F.);
#11354=ORIENTED_EDGE('',*,*,#8402,.T.);
#11355=ORIENTED_EDGE('',*,*,#8403,.F.);
#11356=ORIENTED_EDGE('',*,*,#8396,.F.);
#11357=ORIENTED_EDGE('',*,*,#8400,.F.);
#11358=ORIENTED_EDGE('',*,*,#8404,.F.);
#11359=ORIENTED_EDGE('',*,*,#8405,.T.);
#11360=ORIENTED_EDGE('',*,*,#8404,.T.);
#11361=ORIENTED_EDGE('',*,*,#8399,.T.);
#11362=ORIENTED_EDGE('',*,*,#8406,.T.);
#11363=ORIENTED_EDGE('',*,*,#8397,.F.);
#11364=ORIENTED_EDGE('',*,*,#8403,.T.);
#11365=ORIENTED_EDGE('',*,*,#8405,.F.);
#11366=ORIENTED_EDGE('',*,*,#8407,.T.);
#11367=ORIENTED_EDGE('',*,*,#8391,.T.);
#11368=ORIENTED_EDGE('',*,*,#8408,.T.);
#11369=ORIENTED_EDGE('',*,*,#8409,.F.);
#11370=ORIENTED_EDGE('',*,*,#8182,.T.);
#11371=ORIENTED_EDGE('',*,*,#8162,.T.);
#11372=ORIENTED_EDGE('',*,*,#8410,.T.);
#11373=ORIENTED_EDGE('',*,*,#8185,.F.);
#11374=ORIENTED_EDGE('',*,*,#8183,.T.);
#11375=ORIENTED_EDGE('',*,*,#8409,.T.);
#11376=ORIENTED_EDGE('',*,*,#8411,.T.);
#11377=ORIENTED_EDGE('',*,*,#8169,.F.);
#11378=ORIENTED_EDGE('',*,*,#8180,.T.);
#11379=ORIENTED_EDGE('',*,*,#8402,.F.);
#11380=ORIENTED_EDGE('',*,*,#8392,.F.);
#11381=ORIENTED_EDGE('',*,*,#8407,.F.);
#11382=ORIENTED_EDGE('',*,*,#8406,.F.);
#11383=ORIENTED_EDGE('',*,*,#8104,.F.);
#11384=ORIENTED_EDGE('',*,*,#8107,.F.);
#11385=ORIENTED_EDGE('',*,*,#8387,.T.);
#11386=ORIENTED_EDGE('',*,*,#8114,.T.);
#11387=ORIENTED_EDGE('',*,*,#8218,.T.);
#11388=ORIENTED_EDGE('',*,*,#8117,.T.);
#11389=ORIENTED_EDGE('',*,*,#8386,.T.);
#11390=ORIENTED_EDGE('',*,*,#8385,.T.);
#11391=ORIENTED_EDGE('',*,*,#8373,.T.);
#11392=ORIENTED_EDGE('',*,*,#8375,.T.);
#11393=ORIENTED_EDGE('',*,*,#8377,.T.);
#11394=ORIENTED_EDGE('',*,*,#8379,.T.);
#11395=ORIENTED_EDGE('',*,*,#8381,.T.);
#11396=ORIENTED_EDGE('',*,*,#8383,.T.);
#11397=ORIENTED_EDGE('',*,*,#8388,.T.);
#11398=ORIENTED_EDGE('',*,*,#8100,.F.);
#11399=ORIENTED_EDGE('',*,*,#8411,.F.);
#11400=ORIENTED_EDGE('',*,*,#8410,.F.);
#11401=ORIENTED_EDGE('',*,*,#8167,.F.);
#11402=ORIENTED_EDGE('',*,*,#8170,.F.);
#11403=ORIENTED_EDGE('',*,*,#8178,.F.);
#11404=ORIENTED_EDGE('',*,*,#8215,.F.);
#11405=ORIENTED_EDGE('',*,*,#8390,.F.);
#11406=ORIENTED_EDGE('',*,*,#8174,.F.);
#11407=ORIENTED_EDGE('',*,*,#8408,.F.);
#11408=ORIENTED_EDGE('',*,*,#8394,.F.);
#11409=ORIENTED_EDGE('',*,*,#8401,.F.);
#11410=ORIENTED_EDGE('',*,*,#8398,.F.);
#11411=ORIENTED_EDGE('',*,*,#8412,.T.);
#11412=ORIENTED_EDGE('',*,*,#8413,.T.);
#11413=ORIENTED_EDGE('',*,*,#8414,.T.);
#11414=ORIENTED_EDGE('',*,*,#8415,.T.);
#11415=ORIENTED_EDGE('',*,*,#8416,.T.);
#11416=ORIENTED_EDGE('',*,*,#8417,.T.);
#11417=ORIENTED_EDGE('',*,*,#8418,.T.);
#11418=ORIENTED_EDGE('',*,*,#8414,.F.);
#11419=ORIENTED_EDGE('',*,*,#8419,.F.);
#11420=ORIENTED_EDGE('',*,*,#8420,.F.);
#11421=ORIENTED_EDGE('',*,*,#8421,.F.);
#11422=ORIENTED_EDGE('',*,*,#8422,.F.);
#11423=ORIENTED_EDGE('',*,*,#8423,.T.);
#11424=ORIENTED_EDGE('',*,*,#8424,.F.);
#11425=ORIENTED_EDGE('',*,*,#8425,.F.);
#11426=ORIENTED_EDGE('',*,*,#8423,.F.);
#11427=ORIENTED_EDGE('',*,*,#8426,.F.);
#11428=ORIENTED_EDGE('',*,*,#8427,.T.);
#11429=ORIENTED_EDGE('',*,*,#8428,.T.);
#11430=ORIENTED_EDGE('',*,*,#8429,.T.);
#11431=ORIENTED_EDGE('',*,*,#8430,.T.);
#11432=ORIENTED_EDGE('',*,*,#8431,.F.);
#11433=ORIENTED_EDGE('',*,*,#8432,.T.);
#11434=ORIENTED_EDGE('',*,*,#8433,.F.);
#11435=ORIENTED_EDGE('',*,*,#8432,.F.);
#11436=ORIENTED_EDGE('',*,*,#8434,.T.);
#11437=ORIENTED_EDGE('',*,*,#8435,.T.);
#11438=ORIENTED_EDGE('',*,*,#8436,.T.);
#11439=ORIENTED_EDGE('',*,*,#8437,.T.);
#11440=ORIENTED_EDGE('',*,*,#8438,.T.);
#11441=ORIENTED_EDGE('',*,*,#8439,.T.);
#11442=ORIENTED_EDGE('',*,*,#8435,.F.);
#11443=ORIENTED_EDGE('',*,*,#8440,.T.);
#11444=ORIENTED_EDGE('',*,*,#8441,.T.);
#11445=ORIENTED_EDGE('',*,*,#8412,.F.);
#11446=ORIENTED_EDGE('',*,*,#8413,.F.);
#11447=ORIENTED_EDGE('',*,*,#8441,.F.);
#11448=ORIENTED_EDGE('',*,*,#8425,.T.);
#11449=ORIENTED_EDGE('',*,*,#8442,.T.);
#11450=ORIENTED_EDGE('',*,*,#8443,.F.);
#11451=ORIENTED_EDGE('',*,*,#8442,.F.);
#11452=ORIENTED_EDGE('',*,*,#8424,.T.);
#11453=ORIENTED_EDGE('',*,*,#8444,.F.);
#11454=ORIENTED_EDGE('',*,*,#8445,.T.);
#11455=ORIENTED_EDGE('',*,*,#8446,.T.);
#11456=ORIENTED_EDGE('',*,*,#8445,.F.);
#11457=ORIENTED_EDGE('',*,*,#8447,.F.);
#11458=ORIENTED_EDGE('',*,*,#8448,.F.);
#11459=ORIENTED_EDGE('',*,*,#8449,.T.);
#11460=ORIENTED_EDGE('',*,*,#8450,.F.);
#11461=ORIENTED_EDGE('',*,*,#8449,.F.);
#11462=ORIENTED_EDGE('',*,*,#8451,.T.);
#11463=ORIENTED_EDGE('',*,*,#8452,.T.);
#11464=ORIENTED_EDGE('',*,*,#8453,.T.);
#11465=ORIENTED_EDGE('',*,*,#8447,.T.);
#11466=ORIENTED_EDGE('',*,*,#8448,.T.);
#11467=ORIENTED_EDGE('',*,*,#8453,.F.);
#11468=ORIENTED_EDGE('',*,*,#8454,.T.);
#11469=ORIENTED_EDGE('',*,*,#8455,.T.);
#11470=ORIENTED_EDGE('',*,*,#8456,.T.);
#11471=ORIENTED_EDGE('',*,*,#8457,.F.);
#11472=ORIENTED_EDGE('',*,*,#8458,.T.);
#11473=ORIENTED_EDGE('',*,*,#8459,.T.);
#11474=ORIENTED_EDGE('',*,*,#8460,.T.);
#11475=ORIENTED_EDGE('',*,*,#8461,.T.);
#11476=ORIENTED_EDGE('',*,*,#8462,.T.);
#11477=ORIENTED_EDGE('',*,*,#8463,.F.);
#11478=ORIENTED_EDGE('',*,*,#8464,.T.);
#11479=ORIENTED_EDGE('',*,*,#8465,.T.);
#11480=ORIENTED_EDGE('',*,*,#8466,.T.);
#11481=ORIENTED_EDGE('',*,*,#8455,.F.);
#11482=ORIENTED_EDGE('',*,*,#8467,.T.);
#11483=ORIENTED_EDGE('',*,*,#8468,.T.);
#11484=ORIENTED_EDGE('',*,*,#8469,.T.);
#11485=ORIENTED_EDGE('',*,*,#8470,.T.);
#11486=ORIENTED_EDGE('',*,*,#8471,.T.);
#11487=ORIENTED_EDGE('',*,*,#8472,.T.);
#11488=ORIENTED_EDGE('',*,*,#8473,.T.);
#11489=ORIENTED_EDGE('',*,*,#8474,.T.);
#11490=ORIENTED_EDGE('',*,*,#8475,.T.);
#11491=ORIENTED_EDGE('',*,*,#8476,.T.);
#11492=ORIENTED_EDGE('',*,*,#8477,.T.);
#11493=ORIENTED_EDGE('',*,*,#8478,.F.);
#11494=ORIENTED_EDGE('',*,*,#8479,.T.);
#11495=ORIENTED_EDGE('',*,*,#8480,.F.);
#11496=ORIENTED_EDGE('',*,*,#8481,.T.);
#11497=ORIENTED_EDGE('',*,*,#8469,.F.);
#11498=ORIENTED_EDGE('',*,*,#8426,.T.);
#11499=ORIENTED_EDGE('',*,*,#8431,.T.);
#11500=ORIENTED_EDGE('',*,*,#8482,.T.);
#11501=ORIENTED_EDGE('',*,*,#8483,.F.);
#11502=ORIENTED_EDGE('',*,*,#8484,.T.);
#11503=ORIENTED_EDGE('',*,*,#8451,.F.);
#11504=ORIENTED_EDGE('',*,*,#8452,.F.);
#11505=ORIENTED_EDGE('',*,*,#8484,.F.);
#11506=ORIENTED_EDGE('',*,*,#8485,.F.);
#11507=ORIENTED_EDGE('',*,*,#8486,.T.);
#11508=ORIENTED_EDGE('',*,*,#8487,.F.);
#11509=ORIENTED_EDGE('',*,*,#8488,.T.);
#11510=ORIENTED_EDGE('',*,*,#8489,.F.);
#11511=ORIENTED_EDGE('',*,*,#8490,.F.);
#11512=ORIENTED_EDGE('',*,*,#8491,.F.);
#11513=ORIENTED_EDGE('',*,*,#8492,.F.);
#11514=ORIENTED_EDGE('',*,*,#8493,.T.);
#11515=ORIENTED_EDGE('',*,*,#8494,.T.);
#11516=ORIENTED_EDGE('',*,*,#8495,.T.);
#11517=ORIENTED_EDGE('',*,*,#8496,.T.);
#11518=ORIENTED_EDGE('',*,*,#8497,.T.);
#11519=ORIENTED_EDGE('',*,*,#8498,.T.);
#11520=ORIENTED_EDGE('',*,*,#8499,.T.);
#11521=ORIENTED_EDGE('',*,*,#8500,.T.);
#11522=ORIENTED_EDGE('',*,*,#8501,.T.);
#11523=ORIENTED_EDGE('',*,*,#8502,.T.);
#11524=ORIENTED_EDGE('',*,*,#8503,.T.);
#11525=ORIENTED_EDGE('',*,*,#8504,.T.);
#11526=ORIENTED_EDGE('',*,*,#8505,.T.);
#11527=ORIENTED_EDGE('',*,*,#8506,.T.);
#11528=ORIENTED_EDGE('',*,*,#8507,.F.);
#11529=ORIENTED_EDGE('',*,*,#8508,.T.);
#11530=ORIENTED_EDGE('',*,*,#8509,.F.);
#11531=ORIENTED_EDGE('',*,*,#8477,.F.);
#11532=ORIENTED_EDGE('',*,*,#8466,.F.);
#11533=ORIENTED_EDGE('',*,*,#8510,.F.);
#11534=ORIENTED_EDGE('',*,*,#8511,.F.);
#11535=ORIENTED_EDGE('',*,*,#8512,.F.);
#11536=ORIENTED_EDGE('',*,*,#8513,.F.);
#11537=ORIENTED_EDGE('',*,*,#8514,.F.);
#11538=ORIENTED_EDGE('',*,*,#8515,.F.);
#11539=ORIENTED_EDGE('',*,*,#8456,.F.);
#11540=ORIENTED_EDGE('',*,*,#8516,.F.);
#11541=ORIENTED_EDGE('',*,*,#8517,.F.);
#11542=ORIENTED_EDGE('',*,*,#8518,.F.);
#11543=ORIENTED_EDGE('',*,*,#8519,.T.);
#11544=ORIENTED_EDGE('',*,*,#8468,.F.);
#11545=ORIENTED_EDGE('',*,*,#8520,.T.);
#11546=ORIENTED_EDGE('',*,*,#8521,.F.);
#11547=ORIENTED_EDGE('',*,*,#8520,.F.);
#11548=ORIENTED_EDGE('',*,*,#8522,.F.);
#11549=ORIENTED_EDGE('',*,*,#8523,.T.);
#11550=ORIENTED_EDGE('',*,*,#8524,.T.);
#11551=ORIENTED_EDGE('',*,*,#8523,.F.);
#11552=ORIENTED_EDGE('',*,*,#8525,.T.);
#11553=ORIENTED_EDGE('',*,*,#8508,.F.);
#11554=ORIENTED_EDGE('',*,*,#8526,.F.);
#11555=ORIENTED_EDGE('',*,*,#8527,.T.);
#11556=ORIENTED_EDGE('',*,*,#8528,.T.);
#11557=ORIENTED_EDGE('',*,*,#8529,.T.);
#11558=ORIENTED_EDGE('',*,*,#8530,.T.);
#11559=ORIENTED_EDGE('',*,*,#8511,.T.);
#11560=ORIENTED_EDGE('',*,*,#8531,.F.);
#11561=ORIENTED_EDGE('',*,*,#8532,.T.);
#11562=ORIENTED_EDGE('',*,*,#8533,.F.);
#11563=ORIENTED_EDGE('',*,*,#8472,.F.);
#11564=ORIENTED_EDGE('',*,*,#8534,.F.);
#11565=ORIENTED_EDGE('',*,*,#8535,.F.);
#11566=ORIENTED_EDGE('',*,*,#8536,.F.);
#11567=ORIENTED_EDGE('',*,*,#8537,.F.);
#11568=ORIENTED_EDGE('',*,*,#8538,.F.);
#11569=ORIENTED_EDGE('',*,*,#8457,.T.);
#11570=ORIENTED_EDGE('',*,*,#8515,.T.);
#11571=ORIENTED_EDGE('',*,*,#8539,.F.);
#11572=ORIENTED_EDGE('',*,*,#8540,.F.);
#11573=ORIENTED_EDGE('',*,*,#8541,.F.);
#11574=ORIENTED_EDGE('',*,*,#8542,.T.);
#11575=ORIENTED_EDGE('',*,*,#8543,.F.);
#11576=ORIENTED_EDGE('',*,*,#8495,.F.);
#11577=ORIENTED_EDGE('',*,*,#8544,.F.);
#11578=ORIENTED_EDGE('',*,*,#8481,.F.);
#11579=ORIENTED_EDGE('',*,*,#8545,.F.);
#11580=ORIENTED_EDGE('',*,*,#8546,.F.);
#11581=ORIENTED_EDGE('',*,*,#8547,.F.);
#11582=ORIENTED_EDGE('',*,*,#8470,.F.);
#11583=ORIENTED_EDGE('',*,*,#8548,.T.);
#11584=ORIENTED_EDGE('',*,*,#8549,.T.);
#11585=ORIENTED_EDGE('',*,*,#8550,.F.);
#11586=ORIENTED_EDGE('',*,*,#8551,.F.);
#11587=ORIENTED_EDGE('',*,*,#8552,.T.);
#11588=ORIENTED_EDGE('',*,*,#8553,.T.);
#11589=ORIENTED_EDGE('',*,*,#8554,.F.);
#11590=ORIENTED_EDGE('',*,*,#8555,.T.);
#11591=ORIENTED_EDGE('',*,*,#8556,.F.);
#11592=ORIENTED_EDGE('',*,*,#8557,.F.);
#11593=ORIENTED_EDGE('',*,*,#8558,.T.);
#11594=ORIENTED_EDGE('',*,*,#8559,.F.);
#11595=ORIENTED_EDGE('',*,*,#8560,.F.);
#11596=ORIENTED_EDGE('',*,*,#8561,.T.);
#11597=ORIENTED_EDGE('',*,*,#8562,.T.);
#11598=ORIENTED_EDGE('',*,*,#8563,.T.);
#11599=ORIENTED_EDGE('',*,*,#8564,.T.);
#11600=ORIENTED_EDGE('',*,*,#8565,.F.);
#11601=ORIENTED_EDGE('',*,*,#8564,.F.);
#11602=ORIENTED_EDGE('',*,*,#8566,.F.);
#11603=ORIENTED_EDGE('',*,*,#8567,.F.);
#11604=ORIENTED_EDGE('',*,*,#8568,.F.);
#11605=ORIENTED_EDGE('',*,*,#8569,.T.);
#11606=ORIENTED_EDGE('',*,*,#8570,.T.);
#11607=ORIENTED_EDGE('',*,*,#8571,.F.);
#11608=ORIENTED_EDGE('',*,*,#8548,.F.);
#11609=ORIENTED_EDGE('',*,*,#8572,.F.);
#11610=ORIENTED_EDGE('',*,*,#8573,.F.);
#11611=ORIENTED_EDGE('',*,*,#8574,.T.);
#11612=ORIENTED_EDGE('',*,*,#8575,.F.);
#11613=ORIENTED_EDGE('',*,*,#8576,.T.);
#11614=ORIENTED_EDGE('',*,*,#8577,.F.);
#11615=ORIENTED_EDGE('',*,*,#8578,.T.);
#11616=ORIENTED_EDGE('',*,*,#8579,.F.);
#11617=ORIENTED_EDGE('',*,*,#8580,.F.);
#11618=ORIENTED_EDGE('',*,*,#8581,.F.);
#11619=ORIENTED_EDGE('',*,*,#8582,.F.);
#11620=ORIENTED_EDGE('',*,*,#8418,.F.);
#11621=ORIENTED_EDGE('',*,*,#8583,.T.);
#11622=ORIENTED_EDGE('',*,*,#8419,.T.);
#11623=ORIENTED_EDGE('',*,*,#8422,.T.);
#11624=ORIENTED_EDGE('',*,*,#8584,.F.);
#11625=ORIENTED_EDGE('',*,*,#8415,.F.);
#11626=ORIENTED_EDGE('',*,*,#8437,.F.);
#11627=ORIENTED_EDGE('',*,*,#8585,.T.);
#11628=ORIENTED_EDGE('',*,*,#8586,.F.);
#11629=ORIENTED_EDGE('',*,*,#8587,.F.);
#11630=ORIENTED_EDGE('',*,*,#8438,.F.);
#11631=ORIENTED_EDGE('',*,*,#8430,.F.);
#11632=ORIENTED_EDGE('',*,*,#8588,.T.);
#11633=ORIENTED_EDGE('',*,*,#8589,.F.);
#11634=ORIENTED_EDGE('',*,*,#8590,.F.);
#11635=ORIENTED_EDGE('',*,*,#8427,.F.);
#11636=ORIENTED_EDGE('',*,*,#8482,.F.);
#11637=ORIENTED_EDGE('',*,*,#8440,.F.);
#11638=ORIENTED_EDGE('',*,*,#8591,.T.);
#11639=ORIENTED_EDGE('',*,*,#8433,.T.);
#11640=ORIENTED_EDGE('',*,*,#8591,.F.);
#11641=ORIENTED_EDGE('',*,*,#8434,.F.);
#11642=ORIENTED_EDGE('',*,*,#8592,.T.);
#11643=ORIENTED_EDGE('',*,*,#8443,.T.);
#11644=ORIENTED_EDGE('',*,*,#8592,.F.);
#11645=ORIENTED_EDGE('',*,*,#8586,.T.);
#11646=ORIENTED_EDGE('',*,*,#8593,.T.);
#11647=ORIENTED_EDGE('',*,*,#8588,.F.);
#11648=ORIENTED_EDGE('',*,*,#8429,.F.);
#11649=ORIENTED_EDGE('',*,*,#8428,.F.);
#11650=ORIENTED_EDGE('',*,*,#8590,.T.);
#11651=ORIENTED_EDGE('',*,*,#8594,.F.);
#11652=ORIENTED_EDGE('',*,*,#8585,.F.);
#11653=ORIENTED_EDGE('',*,*,#8436,.F.);
#11654=ORIENTED_EDGE('',*,*,#8439,.F.);
#11655=ORIENTED_EDGE('',*,*,#8587,.T.);
#11656=ORIENTED_EDGE('',*,*,#8593,.F.);
#11657=ORIENTED_EDGE('',*,*,#8589,.T.);
#11658=ORIENTED_EDGE('',*,*,#8594,.T.);
#11659=ORIENTED_EDGE('',*,*,#8583,.F.);
#11660=ORIENTED_EDGE('',*,*,#8417,.F.);
#11661=ORIENTED_EDGE('',*,*,#8416,.F.);
#11662=ORIENTED_EDGE('',*,*,#8584,.T.);
#11663=ORIENTED_EDGE('',*,*,#8421,.T.);
#11664=ORIENTED_EDGE('',*,*,#8420,.T.);
#11665=ORIENTED_EDGE('',*,*,#8595,.F.);
#11666=ORIENTED_EDGE('',*,*,#8491,.T.);
#11667=ORIENTED_EDGE('',*,*,#8596,.F.);
#11668=ORIENTED_EDGE('',*,*,#8577,.T.);
#11669=ORIENTED_EDGE('',*,*,#8530,.F.);
#11670=ORIENTED_EDGE('',*,*,#8597,.T.);
#11671=ORIENTED_EDGE('',*,*,#8598,.T.);
#11672=ORIENTED_EDGE('',*,*,#8599,.T.);
#11673=ORIENTED_EDGE('',*,*,#8596,.T.);
#11674=ORIENTED_EDGE('',*,*,#8600,.T.);
#11675=ORIENTED_EDGE('',*,*,#8601,.F.);
#11676=ORIENTED_EDGE('',*,*,#8602,.T.);
#11677=ORIENTED_EDGE('',*,*,#8603,.T.);
#11678=ORIENTED_EDGE('',*,*,#8604,.T.);
#11679=ORIENTED_EDGE('',*,*,#8595,.T.);
#11680=ORIENTED_EDGE('',*,*,#8605,.T.);
#11681=ORIENTED_EDGE('',*,*,#8606,.T.);
#11682=ORIENTED_EDGE('',*,*,#8607,.T.);
#11683=ORIENTED_EDGE('',*,*,#8608,.F.);
#11684=ORIENTED_EDGE('',*,*,#8609,.T.);
#11685=ORIENTED_EDGE('',*,*,#8610,.T.);
#11686=ORIENTED_EDGE('',*,*,#8611,.T.);
#11687=ORIENTED_EDGE('',*,*,#8612,.F.);
#11688=ORIENTED_EDGE('',*,*,#8613,.T.);
#11689=ORIENTED_EDGE('',*,*,#8614,.T.);
#11690=ORIENTED_EDGE('',*,*,#8615,.T.);
#11691=ORIENTED_EDGE('',*,*,#8616,.T.);
#11692=ORIENTED_EDGE('',*,*,#8617,.T.);
#11693=ORIENTED_EDGE('',*,*,#8473,.F.);
#11694=ORIENTED_EDGE('',*,*,#8537,.T.);
#11695=ORIENTED_EDGE('',*,*,#8618,.T.);
#11696=ORIENTED_EDGE('',*,*,#8582,.T.);
#11697=ORIENTED_EDGE('',*,*,#8619,.F.);
#11698=ORIENTED_EDGE('',*,*,#8578,.F.);
#11699=ORIENTED_EDGE('',*,*,#8602,.F.);
#11700=ORIENTED_EDGE('',*,*,#8580,.T.);
#11701=ORIENTED_EDGE('',*,*,#8605,.F.);
#11702=ORIENTED_EDGE('',*,*,#8576,.F.);
#11703=ORIENTED_EDGE('',*,*,#8620,.F.);
#11704=ORIENTED_EDGE('',*,*,#8621,.F.);
#11705=ORIENTED_EDGE('',*,*,#8622,.F.);
#11706=ORIENTED_EDGE('',*,*,#8623,.F.);
#11707=ORIENTED_EDGE('',*,*,#8624,.F.);
#11708=ORIENTED_EDGE('',*,*,#8623,.T.);
#11709=ORIENTED_EDGE('',*,*,#8625,.F.);
#11710=ORIENTED_EDGE('',*,*,#8626,.F.);
#11711=ORIENTED_EDGE('',*,*,#8609,.F.);
#11712=ORIENTED_EDGE('',*,*,#8621,.T.);
#11713=ORIENTED_EDGE('',*,*,#8617,.F.);
#11714=ORIENTED_EDGE('',*,*,#8627,.F.);
#11715=ORIENTED_EDGE('',*,*,#8628,.F.);
#11716=ORIENTED_EDGE('',*,*,#8490,.T.);
#11717=ORIENTED_EDGE('',*,*,#8629,.F.);
#11718=ORIENTED_EDGE('',*,*,#8486,.F.);
#11719=ORIENTED_EDGE('',*,*,#8600,.F.);
#11720=ORIENTED_EDGE('',*,*,#8492,.T.);
#11721=ORIENTED_EDGE('',*,*,#8604,.F.);
#11722=ORIENTED_EDGE('',*,*,#8488,.F.);
#11723=ORIENTED_EDGE('',*,*,#8630,.F.);
#11724=ORIENTED_EDGE('',*,*,#8631,.T.);
#11725=ORIENTED_EDGE('',*,*,#8632,.F.);
#11726=ORIENTED_EDGE('',*,*,#8633,.F.);
#11727=ORIENTED_EDGE('',*,*,#8634,.F.);
#11728=ORIENTED_EDGE('',*,*,#8635,.T.);
#11729=ORIENTED_EDGE('',*,*,#8636,.F.);
#11730=ORIENTED_EDGE('',*,*,#8637,.F.);
#11731=ORIENTED_EDGE('',*,*,#8638,.F.);
#11732=ORIENTED_EDGE('',*,*,#8479,.F.);
#11733=ORIENTED_EDGE('',*,*,#8639,.F.);
#11734=ORIENTED_EDGE('',*,*,#8635,.F.);
#11735=ORIENTED_EDGE('',*,*,#8640,.F.);
#11736=ORIENTED_EDGE('',*,*,#8641,.T.);
#11737=ORIENTED_EDGE('',*,*,#8642,.T.);
#11738=ORIENTED_EDGE('',*,*,#8643,.T.);
#11739=ORIENTED_EDGE('',*,*,#8644,.T.);
#11740=ORIENTED_EDGE('',*,*,#8645,.F.);
#11741=ORIENTED_EDGE('',*,*,#8646,.T.);
#11742=ORIENTED_EDGE('',*,*,#8647,.F.);
#11743=ORIENTED_EDGE('',*,*,#8648,.F.);
#11744=ORIENTED_EDGE('',*,*,#8647,.T.);
#11745=ORIENTED_EDGE('',*,*,#8649,.F.);
#11746=ORIENTED_EDGE('',*,*,#8650,.F.);
#11747=ORIENTED_EDGE('',*,*,#8651,.F.);
#11748=ORIENTED_EDGE('',*,*,#8501,.F.);
#11749=ORIENTED_EDGE('',*,*,#8652,.F.);
#11750=ORIENTED_EDGE('',*,*,#8650,.T.);
#11751=ORIENTED_EDGE('',*,*,#8653,.F.);
#11752=ORIENTED_EDGE('',*,*,#8502,.F.);
#11753=ORIENTED_EDGE('',*,*,#8653,.T.);
#11754=ORIENTED_EDGE('',*,*,#8649,.T.);
#11755=ORIENTED_EDGE('',*,*,#8654,.T.);
#11756=ORIENTED_EDGE('',*,*,#8655,.F.);
#11757=ORIENTED_EDGE('',*,*,#8656,.T.);
#11758=ORIENTED_EDGE('',*,*,#8645,.T.);
#11759=ORIENTED_EDGE('',*,*,#8657,.T.);
#11760=ORIENTED_EDGE('',*,*,#8658,.F.);
#11761=ORIENTED_EDGE('',*,*,#8659,.T.);
#11762=ORIENTED_EDGE('',*,*,#8660,.T.);
#11763=ORIENTED_EDGE('',*,*,#8661,.T.);
#11764=ORIENTED_EDGE('',*,*,#8534,.T.);
#11765=ORIENTED_EDGE('',*,*,#8471,.F.);
#11766=ORIENTED_EDGE('',*,*,#8662,.F.);
#11767=ORIENTED_EDGE('',*,*,#8562,.F.);
#11768=ORIENTED_EDGE('',*,*,#8663,.F.);
#11769=ORIENTED_EDGE('',*,*,#8664,.F.);
#11770=ORIENTED_EDGE('',*,*,#8559,.T.);
#11771=ORIENTED_EDGE('',*,*,#8665,.T.);
#11772=ORIENTED_EDGE('',*,*,#8666,.T.);
#11773=ORIENTED_EDGE('',*,*,#8667,.T.);
#11774=ORIENTED_EDGE('',*,*,#8557,.T.);
#11775=ORIENTED_EDGE('',*,*,#8668,.F.);
#11776=ORIENTED_EDGE('',*,*,#8565,.T.);
#11777=ORIENTED_EDGE('',*,*,#8571,.T.);
#11778=ORIENTED_EDGE('',*,*,#8669,.T.);
#11779=ORIENTED_EDGE('',*,*,#8563,.F.);
#11780=ORIENTED_EDGE('',*,*,#8670,.T.);
#11781=ORIENTED_EDGE('',*,*,#8566,.T.);
#11782=ORIENTED_EDGE('',*,*,#8671,.T.);
#11783=ORIENTED_EDGE('',*,*,#8672,.T.);
#11784=ORIENTED_EDGE('',*,*,#8554,.T.);
#11785=ORIENTED_EDGE('',*,*,#8673,.T.);
#11786=ORIENTED_EDGE('',*,*,#8674,.F.);
#11787=ORIENTED_EDGE('',*,*,#8675,.F.);
#11788=ORIENTED_EDGE('',*,*,#8553,.F.);
#11789=ORIENTED_EDGE('',*,*,#8675,.T.);
#11790=ORIENTED_EDGE('',*,*,#8676,.F.);
#11791=ORIENTED_EDGE('',*,*,#8677,.F.);
#11792=ORIENTED_EDGE('',*,*,#8671,.F.);
#11793=ORIENTED_EDGE('',*,*,#8678,.F.);
#11794=ORIENTED_EDGE('',*,*,#8679,.F.);
#11795=ORIENTED_EDGE('',*,*,#8680,.F.);
#11796=ORIENTED_EDGE('',*,*,#8677,.T.);
#11797=ORIENTED_EDGE('',*,*,#8681,.F.);
#11798=ORIENTED_EDGE('',*,*,#8680,.T.);
#11799=ORIENTED_EDGE('',*,*,#8682,.F.);
#11800=ORIENTED_EDGE('',*,*,#8555,.F.);
#11801=ORIENTED_EDGE('',*,*,#8672,.F.);
#11802=ORIENTED_EDGE('',*,*,#8683,.F.);
#11803=ORIENTED_EDGE('',*,*,#8684,.F.);
#11804=ORIENTED_EDGE('',*,*,#8572,.T.);
#11805=ORIENTED_EDGE('',*,*,#8669,.F.);
#11806=ORIENTED_EDGE('',*,*,#8568,.T.);
#11807=ORIENTED_EDGE('',*,*,#8685,.T.);
#11808=ORIENTED_EDGE('',*,*,#8686,.F.);
#11809=ORIENTED_EDGE('',*,*,#8683,.T.);
#11810=ORIENTED_EDGE('',*,*,#8570,.F.);
#11811=ORIENTED_EDGE('',*,*,#8569,.F.);
#11812=ORIENTED_EDGE('',*,*,#8670,.F.);
#11813=ORIENTED_EDGE('',*,*,#8662,.T.);
#11814=ORIENTED_EDGE('',*,*,#8687,.F.);
#11815=ORIENTED_EDGE('',*,*,#8685,.F.);
#11816=ORIENTED_EDGE('',*,*,#8567,.T.);
#11817=ORIENTED_EDGE('',*,*,#8688,.F.);
#11818=ORIENTED_EDGE('',*,*,#8549,.F.);
#11819=ORIENTED_EDGE('',*,*,#8574,.F.);
#11820=ORIENTED_EDGE('',*,*,#8689,.F.);
#11821=ORIENTED_EDGE('',*,*,#8521,.T.);
#11822=ORIENTED_EDGE('',*,*,#8666,.F.);
#11823=ORIENTED_EDGE('',*,*,#8690,.T.);
#11824=ORIENTED_EDGE('',*,*,#8691,.F.);
#11825=ORIENTED_EDGE('',*,*,#8692,.F.);
#11826=ORIENTED_EDGE('',*,*,#8673,.F.);
#11827=ORIENTED_EDGE('',*,*,#8552,.F.);
#11828=ORIENTED_EDGE('',*,*,#8693,.F.);
#11829=ORIENTED_EDGE('',*,*,#8652,.T.);
#11830=ORIENTED_EDGE('',*,*,#8500,.F.);
#11831=ORIENTED_EDGE('',*,*,#8694,.T.);
#11832=ORIENTED_EDGE('',*,*,#8689,.T.);
#11833=ORIENTED_EDGE('',*,*,#8497,.F.);
#11834=ORIENTED_EDGE('',*,*,#8695,.T.);
#11835=ORIENTED_EDGE('',*,*,#8696,.F.);
#11836=ORIENTED_EDGE('',*,*,#8692,.T.);
#11837=ORIENTED_EDGE('',*,*,#8697,.F.);
#11838=ORIENTED_EDGE('',*,*,#8698,.T.);
#11839=ORIENTED_EDGE('',*,*,#8699,.F.);
#11840=ORIENTED_EDGE('',*,*,#8700,.F.);
#11841=ORIENTED_EDGE('',*,*,#8474,.F.);
#11842=ORIENTED_EDGE('',*,*,#8700,.T.);
#11843=ORIENTED_EDGE('',*,*,#8695,.F.);
#11844=ORIENTED_EDGE('',*,*,#8476,.F.);
#11845=ORIENTED_EDGE('',*,*,#8475,.F.);
#11846=ORIENTED_EDGE('',*,*,#8701,.F.);
#11847=ORIENTED_EDGE('',*,*,#8702,.T.);
#11848=ORIENTED_EDGE('',*,*,#8661,.F.);
#11849=ORIENTED_EDGE('',*,*,#8547,.T.);
#11850=ORIENTED_EDGE('',*,*,#8703,.F.);
#11851=ORIENTED_EDGE('',*,*,#8704,.T.);
#11852=ORIENTED_EDGE('',*,*,#8705,.T.);
#11853=ORIENTED_EDGE('',*,*,#8459,.F.);
#11854=ORIENTED_EDGE('',*,*,#8706,.T.);
#11855=ORIENTED_EDGE('',*,*,#8707,.T.);
#11856=ORIENTED_EDGE('',*,*,#8708,.T.);
#11857=ORIENTED_EDGE('',*,*,#8709,.T.);
#11858=ORIENTED_EDGE('',*,*,#8710,.T.);
#11859=ORIENTED_EDGE('',*,*,#8711,.T.);
#11860=ORIENTED_EDGE('',*,*,#8712,.T.);
#11861=ORIENTED_EDGE('',*,*,#8527,.F.);
#11862=ORIENTED_EDGE('',*,*,#8713,.T.);
#11863=ORIENTED_EDGE('',*,*,#8637,.T.);
#11864=ORIENTED_EDGE('',*,*,#8714,.F.);
#11865=ORIENTED_EDGE('',*,*,#8715,.F.);
#11866=ORIENTED_EDGE('',*,*,#8707,.F.);
#11867=ORIENTED_EDGE('',*,*,#8708,.F.);
#11868=ORIENTED_EDGE('',*,*,#8716,.T.);
#11869=ORIENTED_EDGE('',*,*,#8710,.F.);
#11870=ORIENTED_EDGE('',*,*,#8717,.F.);
#11871=ORIENTED_EDGE('',*,*,#8718,.F.);
#11872=ORIENTED_EDGE('',*,*,#8719,.T.);
#11873=ORIENTED_EDGE('',*,*,#8494,.F.);
#11874=ORIENTED_EDGE('',*,*,#8720,.F.);
#11875=ORIENTED_EDGE('',*,*,#8721,.F.);
#11876=ORIENTED_EDGE('',*,*,#8638,.T.);
#11877=ORIENTED_EDGE('',*,*,#8706,.F.);
#11878=ORIENTED_EDGE('',*,*,#8722,.F.);
#11879=ORIENTED_EDGE('',*,*,#8510,.T.);
#11880=ORIENTED_EDGE('',*,*,#8465,.F.);
#11881=ORIENTED_EDGE('',*,*,#8723,.T.);
#11882=ORIENTED_EDGE('',*,*,#8724,.T.);
#11883=ORIENTED_EDGE('',*,*,#8531,.T.);
#11884=ORIENTED_EDGE('',*,*,#8723,.F.);
#11885=ORIENTED_EDGE('',*,*,#8464,.F.);
#11886=ORIENTED_EDGE('',*,*,#8725,.F.);
#11887=ORIENTED_EDGE('',*,*,#8726,.T.);
#11888=ORIENTED_EDGE('',*,*,#8727,.T.);
#11889=ORIENTED_EDGE('',*,*,#8728,.T.);
#11890=ORIENTED_EDGE('',*,*,#8729,.T.);
#11891=ORIENTED_EDGE('',*,*,#8730,.T.);
#11892=ORIENTED_EDGE('',*,*,#8731,.T.);
#11893=ORIENTED_EDGE('',*,*,#8732,.F.);
#11894=ORIENTED_EDGE('',*,*,#8733,.F.);
#11895=ORIENTED_EDGE('',*,*,#8704,.F.);
#11896=ORIENTED_EDGE('',*,*,#8734,.F.);
#11897=ORIENTED_EDGE('',*,*,#8735,.T.);
#11898=ORIENTED_EDGE('',*,*,#8736,.T.);
#11899=ORIENTED_EDGE('',*,*,#8618,.F.);
#11900=ORIENTED_EDGE('',*,*,#8737,.T.);
#11901=ORIENTED_EDGE('',*,*,#8738,.F.);
#11902=ORIENTED_EDGE('',*,*,#8698,.F.);
#11903=ORIENTED_EDGE('',*,*,#8535,.T.);
#11904=ORIENTED_EDGE('',*,*,#8702,.F.);
#11905=ORIENTED_EDGE('',*,*,#8739,.F.);
#11906=ORIENTED_EDGE('',*,*,#8740,.F.);
#11907=ORIENTED_EDGE('',*,*,#8741,.F.);
#11908=ORIENTED_EDGE('',*,*,#8737,.F.);
#11909=ORIENTED_EDGE('',*,*,#8536,.T.);
#11910=ORIENTED_EDGE('',*,*,#8742,.F.);
#11911=ORIENTED_EDGE('',*,*,#8597,.F.);
#11912=ORIENTED_EDGE('',*,*,#8743,.T.);
#11913=ORIENTED_EDGE('',*,*,#8744,.F.);
#11914=ORIENTED_EDGE('',*,*,#8745,.T.);
#11915=ORIENTED_EDGE('',*,*,#8746,.F.);
#11916=ORIENTED_EDGE('',*,*,#8747,.T.);
#11917=ORIENTED_EDGE('',*,*,#8716,.F.);
#11918=ORIENTED_EDGE('',*,*,#8715,.T.);
#11919=ORIENTED_EDGE('',*,*,#8743,.F.);
#11920=ORIENTED_EDGE('',*,*,#8529,.F.);
#11921=ORIENTED_EDGE('',*,*,#8748,.F.);
#11922=ORIENTED_EDGE('',*,*,#8749,.F.);
#11923=ORIENTED_EDGE('',*,*,#8750,.T.);
#11924=ORIENTED_EDGE('',*,*,#8711,.F.);
#11925=ORIENTED_EDGE('',*,*,#8747,.F.);
#11926=ORIENTED_EDGE('',*,*,#8751,.F.);
#11927=ORIENTED_EDGE('',*,*,#8528,.F.);
#11928=ORIENTED_EDGE('',*,*,#8712,.F.);
#11929=ORIENTED_EDGE('',*,*,#8750,.F.);
#11930=ORIENTED_EDGE('',*,*,#8748,.T.);
#11931=ORIENTED_EDGE('',*,*,#8752,.T.);
#11932=ORIENTED_EDGE('',*,*,#8753,.T.);
#11933=ORIENTED_EDGE('',*,*,#8718,.T.);
#11934=ORIENTED_EDGE('',*,*,#8754,.T.);
#11935=ORIENTED_EDGE('',*,*,#8540,.T.);
#11936=ORIENTED_EDGE('',*,*,#8544,.T.);
#11937=ORIENTED_EDGE('',*,*,#8719,.F.);
#11938=ORIENTED_EDGE('',*,*,#8753,.F.);
#11939=ORIENTED_EDGE('',*,*,#8755,.F.);
#11940=ORIENTED_EDGE('',*,*,#8756,.F.);
#11941=ORIENTED_EDGE('',*,*,#8458,.F.);
#11942=ORIENTED_EDGE('',*,*,#8538,.T.);
#11943=ORIENTED_EDGE('',*,*,#8754,.F.);
#11944=ORIENTED_EDGE('',*,*,#8720,.T.);
#11945=ORIENTED_EDGE('',*,*,#8493,.F.);
#11946=ORIENTED_EDGE('',*,*,#8757,.T.);
#11947=ORIENTED_EDGE('',*,*,#8734,.T.);
#11948=ORIENTED_EDGE('',*,*,#8703,.T.);
#11949=ORIENTED_EDGE('',*,*,#8532,.F.);
#11950=ORIENTED_EDGE('',*,*,#8724,.F.);
#11951=ORIENTED_EDGE('',*,*,#8758,.F.);
#11952=ORIENTED_EDGE('',*,*,#8756,.T.);
#11953=ORIENTED_EDGE('',*,*,#8513,.T.);
#11954=ORIENTED_EDGE('',*,*,#8759,.T.);
#11955=ORIENTED_EDGE('',*,*,#8760,.T.);
#11956=ORIENTED_EDGE('',*,*,#8761,.T.);
#11957=ORIENTED_EDGE('',*,*,#8541,.T.);
#11958=ORIENTED_EDGE('',*,*,#8762,.T.);
#11959=ORIENTED_EDGE('',*,*,#8763,.F.);
#11960=ORIENTED_EDGE('',*,*,#8764,.T.);
#11961=ORIENTED_EDGE('',*,*,#8765,.T.);
#11962=ORIENTED_EDGE('',*,*,#8620,.T.);
#11963=ORIENTED_EDGE('',*,*,#8575,.T.);
#11964=ORIENTED_EDGE('',*,*,#8619,.T.);
#11965=ORIENTED_EDGE('',*,*,#8581,.T.);
#11966=ORIENTED_EDGE('',*,*,#8628,.T.);
#11967=ORIENTED_EDGE('',*,*,#8766,.T.);
#11968=ORIENTED_EDGE('',*,*,#8625,.T.);
#11969=ORIENTED_EDGE('',*,*,#8622,.T.);
#11970=ORIENTED_EDGE('',*,*,#8483,.T.);
#11971=ORIENTED_EDGE('',*,*,#8644,.F.);
#11972=ORIENTED_EDGE('',*,*,#8767,.T.);
#11973=ORIENTED_EDGE('',*,*,#8729,.F.);
#11974=ORIENTED_EDGE('',*,*,#8768,.T.);
#11975=ORIENTED_EDGE('',*,*,#8658,.T.);
#11976=ORIENTED_EDGE('',*,*,#8769,.T.);
#11977=ORIENTED_EDGE('',*,*,#8506,.F.);
#11978=ORIENTED_EDGE('',*,*,#8770,.T.);
#11979=ORIENTED_EDGE('',*,*,#8524,.F.);
#11980=ORIENTED_EDGE('',*,*,#8630,.T.);
#11981=ORIENTED_EDGE('',*,*,#8487,.T.);
#11982=ORIENTED_EDGE('',*,*,#8629,.T.);
#11983=ORIENTED_EDGE('',*,*,#8489,.T.);
#11984=ORIENTED_EDGE('',*,*,#8608,.T.);
#11985=ORIENTED_EDGE('',*,*,#8771,.T.);
#11986=ORIENTED_EDGE('',*,*,#8614,.F.);
#11987=ORIENTED_EDGE('',*,*,#8624,.T.);
#11988=ORIENTED_EDGE('',*,*,#8612,.T.);
#11989=ORIENTED_EDGE('',*,*,#8772,.T.);
#11990=ORIENTED_EDGE('',*,*,#8773,.F.);
#11991=ORIENTED_EDGE('',*,*,#8774,.T.);
#11992=ORIENTED_EDGE('',*,*,#8749,.T.);
#11993=ORIENTED_EDGE('',*,*,#8751,.T.);
#11994=ORIENTED_EDGE('',*,*,#8746,.T.);
#11995=ORIENTED_EDGE('',*,*,#8714,.T.);
#11996=ORIENTED_EDGE('',*,*,#8636,.T.);
#11997=ORIENTED_EDGE('',*,*,#8639,.T.);
#11998=ORIENTED_EDGE('',*,*,#8478,.T.);
#11999=ORIENTED_EDGE('',*,*,#8509,.T.);
#12000=ORIENTED_EDGE('',*,*,#8525,.F.);
#12001=ORIENTED_EDGE('',*,*,#8775,.F.);
#12002=ORIENTED_EDGE('',*,*,#8462,.F.);
#12003=ORIENTED_EDGE('',*,*,#8776,.F.);
#12004=ORIENTED_EDGE('',*,*,#8777,.T.);
#12005=ORIENTED_EDGE('',*,*,#8778,.T.);
#12006=ORIENTED_EDGE('',*,*,#8744,.T.);
#12007=ORIENTED_EDGE('',*,*,#8779,.T.);
#12008=ORIENTED_EDGE('',*,*,#8780,.T.);
#12009=ORIENTED_EDGE('',*,*,#8781,.T.);
#12010=ORIENTED_EDGE('',*,*,#8782,.T.);
#12011=ORIENTED_EDGE('',*,*,#8634,.T.);
#12012=ORIENTED_EDGE('',*,*,#8783,.T.);
#12013=ORIENTED_EDGE('',*,*,#8784,.T.);
#12014=ORIENTED_EDGE('',*,*,#8785,.T.);
#12015=ORIENTED_EDGE('',*,*,#8773,.T.);
#12016=ORIENTED_EDGE('',*,*,#8786,.T.);
#12017=ORIENTED_EDGE('',*,*,#8787,.T.);
#12018=ORIENTED_EDGE('',*,*,#8788,.T.);
#12019=ORIENTED_EDGE('',*,*,#8598,.F.);
#12020=ORIENTED_EDGE('',*,*,#8789,.T.);
#12021=ORIENTED_EDGE('',*,*,#8730,.F.);
#12022=ORIENTED_EDGE('',*,*,#8790,.T.);
#12023=ORIENTED_EDGE('',*,*,#8601,.T.);
#12024=ORIENTED_EDGE('',*,*,#8485,.T.);
#12025=ORIENTED_EDGE('',*,*,#8603,.F.);
#12026=ORIENTED_EDGE('',*,*,#8579,.T.);
#12027=ORIENTED_EDGE('',*,*,#8616,.F.);
#12028=ORIENTED_EDGE('',*,*,#8791,.T.);
#12029=ORIENTED_EDGE('',*,*,#8606,.F.);
#12030=ORIENTED_EDGE('',*,*,#8792,.T.);
#12031=ORIENTED_EDGE('',*,*,#8787,.F.);
#12032=ORIENTED_EDGE('',*,*,#8632,.T.);
#12033=ORIENTED_EDGE('',*,*,#8610,.F.);
#12034=ORIENTED_EDGE('',*,*,#8793,.T.);
#12035=ORIENTED_EDGE('',*,*,#8763,.T.);
#12036=ORIENTED_EDGE('',*,*,#8794,.T.);
#12037=ORIENTED_EDGE('',*,*,#8626,.T.);
#12038=ORIENTED_EDGE('',*,*,#8766,.F.);
#12039=ORIENTED_EDGE('',*,*,#8627,.T.);
#12040=ORIENTED_EDGE('',*,*,#8792,.F.);
#12041=ORIENTED_EDGE('',*,*,#8795,.T.);
#12042=ORIENTED_EDGE('',*,*,#8774,.F.);
#12043=ORIENTED_EDGE('',*,*,#8796,.F.);
#12044=ORIENTED_EDGE('',*,*,#8765,.F.);
#12045=ORIENTED_EDGE('',*,*,#8793,.F.);
#12046=ORIENTED_EDGE('',*,*,#8613,.F.);
#12047=ORIENTED_EDGE('',*,*,#8795,.F.);
#12048=ORIENTED_EDGE('',*,*,#8764,.F.);
#12049=ORIENTED_EDGE('',*,*,#8759,.F.);
#12050=ORIENTED_EDGE('',*,*,#8512,.T.);
#12051=ORIENTED_EDGE('',*,*,#8599,.F.);
#12052=ORIENTED_EDGE('',*,*,#8797,.T.);
#12053=ORIENTED_EDGE('',*,*,#8796,.T.);
#12054=ORIENTED_EDGE('',*,*,#8788,.F.);
#12055=ORIENTED_EDGE('',*,*,#8794,.F.);
#12056=ORIENTED_EDGE('',*,*,#8762,.F.);
#12057=ORIENTED_EDGE('',*,*,#8798,.T.);
#12058=ORIENTED_EDGE('',*,*,#8760,.F.);
#12059=ORIENTED_EDGE('',*,*,#8797,.F.);
#12060=ORIENTED_EDGE('',*,*,#8790,.F.);
#12061=ORIENTED_EDGE('',*,*,#8542,.F.);
#12062=ORIENTED_EDGE('',*,*,#8761,.F.);
#12063=ORIENTED_EDGE('',*,*,#8798,.F.);
#12064=ORIENTED_EDGE('',*,*,#8736,.F.);
#12065=ORIENTED_EDGE('',*,*,#8799,.F.);
#12066=ORIENTED_EDGE('',*,*,#8800,.F.);
#12067=ORIENTED_EDGE('',*,*,#8742,.T.);
#12068=ORIENTED_EDGE('',*,*,#8740,.T.);
#12069=ORIENTED_EDGE('',*,*,#8543,.T.);
#12070=ORIENTED_EDGE('',*,*,#8799,.T.);
#12071=ORIENTED_EDGE('',*,*,#8735,.F.);
#12072=ORIENTED_EDGE('',*,*,#8757,.F.);
#12073=ORIENTED_EDGE('',*,*,#8496,.F.);
#12074=ORIENTED_EDGE('',*,*,#8667,.F.);
#12075=ORIENTED_EDGE('',*,*,#8690,.F.);
#12076=ORIENTED_EDGE('',*,*,#8665,.F.);
#12077=ORIENTED_EDGE('',*,*,#8558,.F.);
#12078=ORIENTED_EDGE('',*,*,#8801,.T.);
#12079=ORIENTED_EDGE('',*,*,#8802,.T.);
#12080=ORIENTED_EDGE('',*,*,#8726,.F.);
#12081=ORIENTED_EDGE('',*,*,#8767,.F.);
#12082=ORIENTED_EDGE('',*,*,#8643,.F.);
#12083=ORIENTED_EDGE('',*,*,#8517,.T.);
#12084=ORIENTED_EDGE('',*,*,#8803,.F.);
#12085=ORIENTED_EDGE('',*,*,#8804,.T.);
#12086=ORIENTED_EDGE('',*,*,#8660,.F.);
#12087=ORIENTED_EDGE('',*,*,#8505,.F.);
#12088=ORIENTED_EDGE('',*,*,#8805,.T.);
#12089=ORIENTED_EDGE('',*,*,#8641,.F.);
#12090=ORIENTED_EDGE('',*,*,#8770,.F.);
#12091=ORIENTED_EDGE('',*,*,#8655,.T.);
#12092=ORIENTED_EDGE('',*,*,#8803,.T.);
#12093=ORIENTED_EDGE('',*,*,#8516,.T.);
#12094=ORIENTED_EDGE('',*,*,#8806,.T.);
#12095=ORIENTED_EDGE('',*,*,#8807,.T.);
#12096=ORIENTED_EDGE('',*,*,#8808,.T.);
#12097=ORIENTED_EDGE('',*,*,#8503,.F.);
#12098=ORIENTED_EDGE('',*,*,#8522,.T.);
#12099=ORIENTED_EDGE('',*,*,#8807,.F.);
#12100=ORIENTED_EDGE('',*,*,#8809,.T.);
#12101=ORIENTED_EDGE('',*,*,#8801,.F.);
#12102=ORIENTED_EDGE('',*,*,#8642,.F.);
#12103=ORIENTED_EDGE('',*,*,#8810,.F.);
#12104=ORIENTED_EDGE('',*,*,#8809,.F.);
#12105=ORIENTED_EDGE('',*,*,#8806,.F.);
#12106=ORIENTED_EDGE('',*,*,#8519,.F.);
#12107=ORIENTED_EDGE('',*,*,#8727,.F.);
#12108=ORIENTED_EDGE('',*,*,#8802,.F.);
#12109=ORIENTED_EDGE('',*,*,#8810,.T.);
#12110=ORIENTED_EDGE('',*,*,#8805,.F.);
#12111=ORIENTED_EDGE('',*,*,#8504,.F.);
#12112=ORIENTED_EDGE('',*,*,#8808,.F.);
#12113=ORIENTED_EDGE('',*,*,#8697,.T.);
#12114=ORIENTED_EDGE('',*,*,#8691,.T.);
#12115=ORIENTED_EDGE('',*,*,#8551,.T.);
#12116=ORIENTED_EDGE('',*,*,#8498,.F.);
#12117=ORIENTED_EDGE('',*,*,#8728,.F.);
#12118=ORIENTED_EDGE('',*,*,#8518,.T.);
#12119=ORIENTED_EDGE('',*,*,#8659,.F.);
#12120=ORIENTED_EDGE('',*,*,#8768,.F.);
#12121=ORIENTED_EDGE('',*,*,#8738,.T.);
#12122=ORIENTED_EDGE('',*,*,#8741,.T.);
#12123=ORIENTED_EDGE('',*,*,#8800,.T.);
#12124=ORIENTED_EDGE('',*,*,#8739,.T.);
#12125=ORIENTED_EDGE('',*,*,#8701,.T.);
#12126=ORIENTED_EDGE('',*,*,#8546,.T.);
#12127=ORIENTED_EDGE('',*,*,#8811,.F.);
#12128=ORIENTED_EDGE('',*,*,#8722,.T.);
#12129=ORIENTED_EDGE('',*,*,#8709,.F.);
#12130=ORIENTED_EDGE('',*,*,#8717,.T.);
#12131=ORIENTED_EDGE('',*,*,#8713,.F.);
#12132=ORIENTED_EDGE('',*,*,#8526,.T.);
#12133=ORIENTED_EDGE('',*,*,#8507,.T.);
#12134=ORIENTED_EDGE('',*,*,#8769,.F.);
#12135=ORIENTED_EDGE('',*,*,#8467,.F.);
#12136=ORIENTED_EDGE('',*,*,#8454,.F.);
#12137=ORIENTED_EDGE('',*,*,#8657,.F.);
#12138=ORIENTED_EDGE('',*,*,#8648,.T.);
#12139=ORIENTED_EDGE('',*,*,#8651,.T.);
#12140=ORIENTED_EDGE('',*,*,#8693,.T.);
#12141=ORIENTED_EDGE('',*,*,#8573,.T.);
#12142=ORIENTED_EDGE('',*,*,#8684,.T.);
#12143=ORIENTED_EDGE('',*,*,#8686,.T.);
#12144=ORIENTED_EDGE('',*,*,#8687,.T.);
#12145=ORIENTED_EDGE('',*,*,#8664,.T.);
#12146=ORIENTED_EDGE('',*,*,#8812,.T.);
#12147=ORIENTED_EDGE('',*,*,#8681,.T.);
#12148=ORIENTED_EDGE('',*,*,#8676,.T.);
#12149=ORIENTED_EDGE('',*,*,#8674,.T.);
#12150=ORIENTED_EDGE('',*,*,#8696,.T.);
#12151=ORIENTED_EDGE('',*,*,#8699,.T.);
#12152=ORIENTED_EDGE('',*,*,#8446,.F.);
#12153=ORIENTED_EDGE('',*,*,#8480,.T.);
#12154=ORIENTED_EDGE('',*,*,#8640,.T.);
#12155=ORIENTED_EDGE('',*,*,#8721,.T.);
#12156=ORIENTED_EDGE('',*,*,#8811,.T.);
#12157=ORIENTED_EDGE('',*,*,#8545,.T.);
#12158=ORIENTED_EDGE('',*,*,#8813,.T.);
#12159=ORIENTED_EDGE('',*,*,#8781,.F.);
#12160=ORIENTED_EDGE('',*,*,#8814,.F.);
#12161=ORIENTED_EDGE('',*,*,#8615,.F.);
#12162=ORIENTED_EDGE('',*,*,#8815,.T.);
#12163=ORIENTED_EDGE('',*,*,#8607,.F.);
#12164=ORIENTED_EDGE('',*,*,#8816,.F.);
#12165=ORIENTED_EDGE('',*,*,#8779,.F.);
#12166=ORIENTED_EDGE('',*,*,#8550,.T.);
#12167=ORIENTED_EDGE('',*,*,#8688,.T.);
#12168=ORIENTED_EDGE('',*,*,#8694,.F.);
#12169=ORIENTED_EDGE('',*,*,#8499,.F.);
#12170=ORIENTED_EDGE('',*,*,#8814,.T.);
#12171=ORIENTED_EDGE('',*,*,#8780,.F.);
#12172=ORIENTED_EDGE('',*,*,#8816,.T.);
#12173=ORIENTED_EDGE('',*,*,#8791,.F.);
#12174=ORIENTED_EDGE('',*,*,#8815,.F.);
#12175=ORIENTED_EDGE('',*,*,#8782,.F.);
#12176=ORIENTED_EDGE('',*,*,#8813,.F.);
#12177=ORIENTED_EDGE('',*,*,#8771,.F.);
#12178=ORIENTED_EDGE('',*,*,#8784,.F.);
#12179=ORIENTED_EDGE('',*,*,#8817,.T.);
#12180=ORIENTED_EDGE('',*,*,#8772,.F.);
#12181=ORIENTED_EDGE('',*,*,#8818,.T.);
#12182=ORIENTED_EDGE('',*,*,#8818,.F.);
#12183=ORIENTED_EDGE('',*,*,#8611,.F.);
#12184=ORIENTED_EDGE('',*,*,#8631,.F.);
#12185=ORIENTED_EDGE('',*,*,#8785,.F.);
#12186=ORIENTED_EDGE('',*,*,#8817,.F.);
#12187=ORIENTED_EDGE('',*,*,#8783,.F.);
#12188=ORIENTED_EDGE('',*,*,#8633,.T.);
#12189=ORIENTED_EDGE('',*,*,#8786,.F.);
#12190=ORIENTED_EDGE('',*,*,#8819,.T.);
#12191=ORIENTED_EDGE('',*,*,#8789,.F.);
#12192=ORIENTED_EDGE('',*,*,#8745,.F.);
#12193=ORIENTED_EDGE('',*,*,#8778,.F.);
#12194=ORIENTED_EDGE('',*,*,#8820,.F.);
#12195=ORIENTED_EDGE('',*,*,#8731,.F.);
#12196=ORIENTED_EDGE('',*,*,#8819,.F.);
#12197=ORIENTED_EDGE('',*,*,#8777,.F.);
#12198=ORIENTED_EDGE('',*,*,#8705,.F.);
#12199=ORIENTED_EDGE('',*,*,#8733,.T.);
#12200=ORIENTED_EDGE('',*,*,#8821,.T.);
#12201=ORIENTED_EDGE('',*,*,#8460,.F.);
#12202=ORIENTED_EDGE('',*,*,#8821,.F.);
#12203=ORIENTED_EDGE('',*,*,#8732,.T.);
#12204=ORIENTED_EDGE('',*,*,#8820,.T.);
#12205=ORIENTED_EDGE('',*,*,#8776,.T.);
#12206=ORIENTED_EDGE('',*,*,#8461,.F.);
#12207=ORIENTED_EDGE('',*,*,#8533,.T.);
#12208=ORIENTED_EDGE('',*,*,#8758,.T.);
#12209=ORIENTED_EDGE('',*,*,#8725,.T.);
#12210=ORIENTED_EDGE('',*,*,#8463,.T.);
#12211=ORIENTED_EDGE('',*,*,#8775,.T.);
#12212=ORIENTED_EDGE('',*,*,#8812,.F.);
#12213=ORIENTED_EDGE('',*,*,#8663,.T.);
#12214=ORIENTED_EDGE('',*,*,#8561,.F.);
#12215=ORIENTED_EDGE('',*,*,#8822,.F.);
#12216=ORIENTED_EDGE('',*,*,#8823,.F.);
#12217=ORIENTED_EDGE('',*,*,#8678,.T.);
#12218=ORIENTED_EDGE('',*,*,#8556,.T.);
#12219=ORIENTED_EDGE('',*,*,#8824,.T.);
#12220=ORIENTED_EDGE('',*,*,#8822,.T.);
#12221=ORIENTED_EDGE('',*,*,#8560,.T.);
#12222=ORIENTED_EDGE('',*,*,#8668,.T.);
#12223=ORIENTED_EDGE('',*,*,#8824,.F.);
#12224=ORIENTED_EDGE('',*,*,#8682,.T.);
#12225=ORIENTED_EDGE('',*,*,#8679,.T.);
#12226=ORIENTED_EDGE('',*,*,#8823,.T.);
#12227=ORIENTED_EDGE('',*,*,#8646,.F.);
#12228=ORIENTED_EDGE('',*,*,#8656,.F.);
#12229=ORIENTED_EDGE('',*,*,#8804,.F.);
#12230=ORIENTED_EDGE('',*,*,#8654,.F.);
#12231=ORIENTED_EDGE('',*,*,#8539,.T.);
#12232=ORIENTED_EDGE('',*,*,#8514,.T.);
#12233=ORIENTED_EDGE('',*,*,#8755,.T.);
#12234=ORIENTED_EDGE('',*,*,#8752,.F.);
#12235=ORIENTED_EDGE('',*,*,#8450,.T.);
#12236=ORIENTED_EDGE('',*,*,#8444,.T.);
#12237=ORIENTED_EDGE('',*,*,#8825,.F.);
#12238=ORIENTED_EDGE('',*,*,#8826,.T.);
#12239=ORIENTED_EDGE('',*,*,#8827,.T.);
#12240=ORIENTED_EDGE('',*,*,#8828,.T.);
#12241=ORIENTED_EDGE('',*,*,#8829,.T.);
#12242=ORIENTED_EDGE('',*,*,#8830,.T.);
#12243=ORIENTED_EDGE('',*,*,#8831,.T.);
#12244=ORIENTED_EDGE('',*,*,#8832,.T.);
#12245=ORIENTED_EDGE('',*,*,#8833,.T.);
#12246=ORIENTED_EDGE('',*,*,#8834,.T.);
#12247=ORIENTED_EDGE('',*,*,#8835,.T.);
#12248=ORIENTED_EDGE('',*,*,#8836,.T.);
#12249=ORIENTED_EDGE('',*,*,#8837,.T.);
#12250=ORIENTED_EDGE('',*,*,#8838,.T.);
#12251=ORIENTED_EDGE('',*,*,#8839,.T.);
#12252=ORIENTED_EDGE('',*,*,#8840,.F.);
#12253=ORIENTED_EDGE('',*,*,#8839,.F.);
#12254=ORIENTED_EDGE('',*,*,#8841,.T.);
#12255=ORIENTED_EDGE('',*,*,#8825,.T.);
#12256=ORIENTED_EDGE('',*,*,#8842,.T.);
#12257=ORIENTED_EDGE('',*,*,#8843,.F.);
#12258=ORIENTED_EDGE('',*,*,#8842,.F.);
#12259=ORIENTED_EDGE('',*,*,#8844,.T.);
#12260=ORIENTED_EDGE('',*,*,#8845,.T.);
#12261=ORIENTED_EDGE('',*,*,#8841,.F.);
#12262=ORIENTED_EDGE('',*,*,#8838,.F.);
#12263=ORIENTED_EDGE('',*,*,#8845,.F.);
#12264=ORIENTED_EDGE('',*,*,#8843,.T.);
#12265=ORIENTED_EDGE('',*,*,#8844,.F.);
#12266=ORIENTED_EDGE('',*,*,#8846,.F.);
#12267=ORIENTED_EDGE('',*,*,#8847,.T.);
#12268=ORIENTED_EDGE('',*,*,#8848,.T.);
#12269=ORIENTED_EDGE('',*,*,#8836,.F.);
#12270=ORIENTED_EDGE('',*,*,#8848,.F.);
#12271=ORIENTED_EDGE('',*,*,#8849,.T.);
#12272=ORIENTED_EDGE('',*,*,#8850,.T.);
#12273=ORIENTED_EDGE('',*,*,#8837,.F.);
#12274=ORIENTED_EDGE('',*,*,#8850,.F.);
#12275=ORIENTED_EDGE('',*,*,#8851,.T.);
#12276=ORIENTED_EDGE('',*,*,#8852,.T.);
#12277=ORIENTED_EDGE('',*,*,#8826,.F.);
#12278=ORIENTED_EDGE('',*,*,#8852,.F.);
#12279=ORIENTED_EDGE('',*,*,#8853,.T.);
#12280=ORIENTED_EDGE('',*,*,#8854,.T.);
#12281=ORIENTED_EDGE('',*,*,#8827,.F.);
#12282=ORIENTED_EDGE('',*,*,#8854,.F.);
#12283=ORIENTED_EDGE('',*,*,#8855,.T.);
#12284=ORIENTED_EDGE('',*,*,#8856,.T.);
#12285=ORIENTED_EDGE('',*,*,#8828,.F.);
#12286=ORIENTED_EDGE('',*,*,#8856,.F.);
#12287=ORIENTED_EDGE('',*,*,#8857,.T.);
#12288=ORIENTED_EDGE('',*,*,#8858,.T.);
#12289=ORIENTED_EDGE('',*,*,#8829,.F.);
#12290=ORIENTED_EDGE('',*,*,#8859,.F.);
#12291=ORIENTED_EDGE('',*,*,#8860,.T.);
#12292=ORIENTED_EDGE('',*,*,#8846,.T.);
#12293=ORIENTED_EDGE('',*,*,#8835,.F.);
#12294=ORIENTED_EDGE('',*,*,#8861,.F.);
#12295=ORIENTED_EDGE('',*,*,#8862,.T.);
#12296=ORIENTED_EDGE('',*,*,#8859,.T.);
#12297=ORIENTED_EDGE('',*,*,#8834,.F.);
#12298=ORIENTED_EDGE('',*,*,#8858,.F.);
#12299=ORIENTED_EDGE('',*,*,#8863,.T.);
#12300=ORIENTED_EDGE('',*,*,#8864,.T.);
#12301=ORIENTED_EDGE('',*,*,#8830,.F.);
#12302=ORIENTED_EDGE('',*,*,#8864,.F.);
#12303=ORIENTED_EDGE('',*,*,#8865,.T.);
#12304=ORIENTED_EDGE('',*,*,#8866,.T.);
#12305=ORIENTED_EDGE('',*,*,#8831,.F.);
#12306=ORIENTED_EDGE('',*,*,#8867,.F.);
#12307=ORIENTED_EDGE('',*,*,#8868,.T.);
#12308=ORIENTED_EDGE('',*,*,#8861,.T.);
#12309=ORIENTED_EDGE('',*,*,#8833,.F.);
#12310=ORIENTED_EDGE('',*,*,#8866,.F.);
#12311=ORIENTED_EDGE('',*,*,#8869,.T.);
#12312=ORIENTED_EDGE('',*,*,#8867,.T.);
#12313=ORIENTED_EDGE('',*,*,#8832,.F.);
#12314=ORIENTED_EDGE('',*,*,#8869,.F.);
#12315=ORIENTED_EDGE('',*,*,#8865,.F.);
#12316=ORIENTED_EDGE('',*,*,#8863,.F.);
#12317=ORIENTED_EDGE('',*,*,#8857,.F.);
#12318=ORIENTED_EDGE('',*,*,#8855,.F.);
#12319=ORIENTED_EDGE('',*,*,#8853,.F.);
#12320=ORIENTED_EDGE('',*,*,#8851,.F.);
#12321=ORIENTED_EDGE('',*,*,#8849,.F.);
#12322=ORIENTED_EDGE('',*,*,#8847,.F.);
#12323=ORIENTED_EDGE('',*,*,#8860,.F.);
#12324=ORIENTED_EDGE('',*,*,#8862,.F.);
#12325=ORIENTED_EDGE('',*,*,#8868,.F.);
#12326=ORIENTED_EDGE('',*,*,#8840,.T.);
#12327=ORIENTED_EDGE('',*,*,#8870,.F.);
#12328=ORIENTED_EDGE('',*,*,#8871,.T.);
#12329=ORIENTED_EDGE('',*,*,#8872,.T.);
#12330=ORIENTED_EDGE('',*,*,#8873,.F.);
#12331=ORIENTED_EDGE('',*,*,#8874,.T.);
#12332=ORIENTED_EDGE('',*,*,#8875,.F.);
#12333=ORIENTED_EDGE('',*,*,#8876,.T.);
#12334=ORIENTED_EDGE('',*,*,#8877,.F.);
#12335=ORIENTED_EDGE('',*,*,#8876,.F.);
#12336=ORIENTED_EDGE('',*,*,#8878,.F.);
#12337=ORIENTED_EDGE('',*,*,#8879,.T.);
#12338=ORIENTED_EDGE('',*,*,#8880,.F.);
#12339=ORIENTED_EDGE('',*,*,#8881,.T.);
#12340=ORIENTED_EDGE('',*,*,#8882,.F.);
#12341=ORIENTED_EDGE('',*,*,#8883,.F.);
#12342=ORIENTED_EDGE('',*,*,#8884,.T.);
#12343=ORIENTED_EDGE('',*,*,#8870,.T.);
#12344=ORIENTED_EDGE('',*,*,#8885,.F.);
#12345=ORIENTED_EDGE('',*,*,#8886,.F.);
#12346=ORIENTED_EDGE('',*,*,#8887,.T.);
#12347=ORIENTED_EDGE('',*,*,#8888,.F.);
#12348=ORIENTED_EDGE('',*,*,#8889,.T.);
#12349=ORIENTED_EDGE('',*,*,#8890,.T.);
#12350=ORIENTED_EDGE('',*,*,#8891,.F.);
#12351=ORIENTED_EDGE('',*,*,#8892,.T.);
#12352=ORIENTED_EDGE('',*,*,#8893,.F.);
#12353=ORIENTED_EDGE('',*,*,#8894,.T.);
#12354=ORIENTED_EDGE('',*,*,#8895,.T.);
#12355=ORIENTED_EDGE('',*,*,#8896,.T.);
#12356=ORIENTED_EDGE('',*,*,#8897,.T.);
#12357=ORIENTED_EDGE('',*,*,#8898,.T.);
#12358=ORIENTED_EDGE('',*,*,#8899,.F.);
#12359=ORIENTED_EDGE('',*,*,#8881,.F.);
#12360=ORIENTED_EDGE('',*,*,#8900,.T.);
#12361=ORIENTED_EDGE('',*,*,#8901,.T.);
#12362=ORIENTED_EDGE('',*,*,#8902,.T.);
#12363=ORIENTED_EDGE('',*,*,#8894,.F.);
#12364=ORIENTED_EDGE('',*,*,#8903,.F.);
#12365=ORIENTED_EDGE('',*,*,#8904,.T.);
#12366=ORIENTED_EDGE('',*,*,#8905,.F.);
#12367=ORIENTED_EDGE('',*,*,#8906,.F.);
#12368=ORIENTED_EDGE('',*,*,#8907,.T.);
#12369=ORIENTED_EDGE('',*,*,#8908,.T.);
#12370=ORIENTED_EDGE('',*,*,#8909,.T.);
#12371=ORIENTED_EDGE('',*,*,#8910,.T.);
#12372=ORIENTED_EDGE('',*,*,#8911,.T.);
#12373=ORIENTED_EDGE('',*,*,#8912,.F.);
#12374=ORIENTED_EDGE('',*,*,#8913,.F.);
#12375=ORIENTED_EDGE('',*,*,#8914,.T.);
#12376=ORIENTED_EDGE('',*,*,#8915,.T.);
#12377=ORIENTED_EDGE('',*,*,#8916,.T.);
#12378=ORIENTED_EDGE('',*,*,#8907,.F.);
#12379=ORIENTED_EDGE('',*,*,#8917,.F.);
#12380=ORIENTED_EDGE('',*,*,#8918,.T.);
#12381=ORIENTED_EDGE('',*,*,#8919,.T.);
#12382=ORIENTED_EDGE('',*,*,#8920,.F.);
#12383=ORIENTED_EDGE('',*,*,#8921,.T.);
#12384=ORIENTED_EDGE('',*,*,#8922,.F.);
#12385=ORIENTED_EDGE('',*,*,#8923,.F.);
#12386=ORIENTED_EDGE('',*,*,#8924,.T.);
#12387=ORIENTED_EDGE('',*,*,#8925,.T.);
#12388=ORIENTED_EDGE('',*,*,#8926,.T.);
#12389=ORIENTED_EDGE('',*,*,#8927,.T.);
#12390=ORIENTED_EDGE('',*,*,#8928,.F.);
#12391=ORIENTED_EDGE('',*,*,#8929,.F.);
#12392=ORIENTED_EDGE('',*,*,#8930,.T.);
#12393=ORIENTED_EDGE('',*,*,#8931,.T.);
#12394=ORIENTED_EDGE('',*,*,#8932,.F.);
#12395=ORIENTED_EDGE('',*,*,#8933,.T.);
#12396=ORIENTED_EDGE('',*,*,#8934,.F.);
#12397=ORIENTED_EDGE('',*,*,#8935,.F.);
#12398=ORIENTED_EDGE('',*,*,#8936,.T.);
#12399=ORIENTED_EDGE('',*,*,#8937,.T.);
#12400=ORIENTED_EDGE('',*,*,#8938,.T.);
#12401=ORIENTED_EDGE('',*,*,#8939,.T.);
#12402=ORIENTED_EDGE('',*,*,#8940,.F.);
#12403=ORIENTED_EDGE('',*,*,#8941,.F.);
#12404=ORIENTED_EDGE('',*,*,#8942,.T.);
#12405=ORIENTED_EDGE('',*,*,#8943,.T.);
#12406=ORIENTED_EDGE('',*,*,#8942,.F.);
#12407=ORIENTED_EDGE('',*,*,#8944,.T.);
#12408=ORIENTED_EDGE('',*,*,#8945,.T.);
#12409=ORIENTED_EDGE('',*,*,#8946,.T.);
#12410=ORIENTED_EDGE('',*,*,#8945,.F.);
#12411=ORIENTED_EDGE('',*,*,#8947,.F.);
#12412=ORIENTED_EDGE('',*,*,#8948,.T.);
#12413=ORIENTED_EDGE('',*,*,#8949,.T.);
#12414=ORIENTED_EDGE('',*,*,#8948,.F.);
#12415=ORIENTED_EDGE('',*,*,#8950,.T.);
#12416=ORIENTED_EDGE('',*,*,#8951,.T.);
#12417=ORIENTED_EDGE('',*,*,#8952,.F.);
#12418=ORIENTED_EDGE('',*,*,#8953,.F.);
#12419=ORIENTED_EDGE('',*,*,#8954,.T.);
#12420=ORIENTED_EDGE('',*,*,#8955,.T.);
#12421=ORIENTED_EDGE('',*,*,#8956,.T.);
#12422=ORIENTED_EDGE('',*,*,#8915,.F.);
#12423=ORIENTED_EDGE('',*,*,#8957,.F.);
#12424=ORIENTED_EDGE('',*,*,#8958,.T.);
#12425=ORIENTED_EDGE('',*,*,#8959,.F.);
#12426=ORIENTED_EDGE('',*,*,#8904,.F.);
#12427=ORIENTED_EDGE('',*,*,#8929,.T.);
#12428=ORIENTED_EDGE('',*,*,#8960,.F.);
#12429=ORIENTED_EDGE('',*,*,#8961,.T.);
#12430=ORIENTED_EDGE('',*,*,#8962,.F.);
#12431=ORIENTED_EDGE('',*,*,#8963,.F.);
#12432=ORIENTED_EDGE('',*,*,#8964,.T.);
#12433=ORIENTED_EDGE('',*,*,#8965,.T.);
#12434=ORIENTED_EDGE('',*,*,#8966,.T.);
#12435=ORIENTED_EDGE('',*,*,#8967,.T.);
#12436=ORIENTED_EDGE('',*,*,#8968,.T.);
#12437=ORIENTED_EDGE('',*,*,#8969,.T.);
#12438=ORIENTED_EDGE('',*,*,#8901,.F.);
#12439=ORIENTED_EDGE('',*,*,#8970,.F.);
#12440=ORIENTED_EDGE('',*,*,#8971,.T.);
#12441=ORIENTED_EDGE('',*,*,#8972,.F.);
#12442=ORIENTED_EDGE('',*,*,#8879,.F.);
#12443=ORIENTED_EDGE('',*,*,#8917,.T.);
#12444=ORIENTED_EDGE('',*,*,#8973,.F.);
#12445=ORIENTED_EDGE('',*,*,#8974,.T.);
#12446=ORIENTED_EDGE('',*,*,#8975,.F.);
#12447=ORIENTED_EDGE('',*,*,#8976,.F.);
#12448=ORIENTED_EDGE('',*,*,#8977,.T.);
#12449=ORIENTED_EDGE('',*,*,#8978,.T.);
#12450=ORIENTED_EDGE('',*,*,#8979,.T.);
#12451=ORIENTED_EDGE('',*,*,#8980,.T.);
#12452=ORIENTED_EDGE('',*,*,#8883,.T.);
#12453=ORIENTED_EDGE('',*,*,#8981,.F.);
#12454=ORIENTED_EDGE('',*,*,#8982,.F.);
#12455=ORIENTED_EDGE('',*,*,#8983,.T.);
#12456=ORIENTED_EDGE('',*,*,#8984,.T.);
#12457=ORIENTED_EDGE('',*,*,#8985,.F.);
#12458=ORIENTED_EDGE('',*,*,#8984,.F.);
#12459=ORIENTED_EDGE('',*,*,#8913,.T.);
#12460=ORIENTED_EDGE('',*,*,#8986,.F.);
#12461=ORIENTED_EDGE('',*,*,#8951,.F.);
#12462=ORIENTED_EDGE('',*,*,#8987,.T.);
#12463=ORIENTED_EDGE('',*,*,#8888,.T.);
#12464=ORIENTED_EDGE('',*,*,#8988,.F.);
#12465=ORIENTED_EDGE('',*,*,#8989,.F.);
#12466=ORIENTED_EDGE('',*,*,#8990,.T.);
#12467=ORIENTED_EDGE('',*,*,#8877,.T.);
#12468=ORIENTED_EDGE('',*,*,#8983,.F.);
#12469=ORIENTED_EDGE('',*,*,#8926,.F.);
#12470=ORIENTED_EDGE('',*,*,#8991,.T.);
#12471=ORIENTED_EDGE('',*,*,#8897,.F.);
#12472=ORIENTED_EDGE('',*,*,#8992,.T.);
#12473=ORIENTED_EDGE('',*,*,#8920,.T.);
#12474=ORIENTED_EDGE('',*,*,#8993,.T.);
#12475=ORIENTED_EDGE('',*,*,#8873,.T.);
#12476=ORIENTED_EDGE('',*,*,#8994,.T.);
#12477=ORIENTED_EDGE('',*,*,#8995,.F.);
#12478=ORIENTED_EDGE('',*,*,#8996,.F.);
#12479=ORIENTED_EDGE('',*,*,#8997,.F.);
#12480=ORIENTED_EDGE('',*,*,#8998,.F.);
#12481=ORIENTED_EDGE('',*,*,#8882,.T.);
#12482=ORIENTED_EDGE('',*,*,#8899,.T.);
#12483=ORIENTED_EDGE('',*,*,#8999,.T.);
#12484=ORIENTED_EDGE('',*,*,#8924,.F.);
#12485=ORIENTED_EDGE('',*,*,#9000,.F.);
#12486=ORIENTED_EDGE('',*,*,#8996,.T.);
#12487=ORIENTED_EDGE('',*,*,#9001,.T.);
#12488=ORIENTED_EDGE('',*,*,#8981,.T.);
#12489=ORIENTED_EDGE('',*,*,#9002,.F.);
#12490=ORIENTED_EDGE('',*,*,#9003,.T.);
#12491=ORIENTED_EDGE('',*,*,#9004,.T.);
#12492=ORIENTED_EDGE('',*,*,#8982,.T.);
#12493=ORIENTED_EDGE('',*,*,#9001,.F.);
#12494=ORIENTED_EDGE('',*,*,#8995,.T.);
#12495=ORIENTED_EDGE('',*,*,#8898,.F.);
#12496=ORIENTED_EDGE('',*,*,#8991,.F.);
#12497=ORIENTED_EDGE('',*,*,#8925,.F.);
#12498=ORIENTED_EDGE('',*,*,#8999,.F.);
#12499=ORIENTED_EDGE('',*,*,#8878,.T.);
#12500=ORIENTED_EDGE('',*,*,#8875,.T.);
#12501=ORIENTED_EDGE('',*,*,#9005,.T.);
#12502=ORIENTED_EDGE('',*,*,#8918,.F.);
#12503=ORIENTED_EDGE('',*,*,#8979,.F.);
#12504=ORIENTED_EDGE('',*,*,#9006,.F.);
#12505=ORIENTED_EDGE('',*,*,#9007,.T.);
#12506=ORIENTED_EDGE('',*,*,#9008,.T.);
#12507=ORIENTED_EDGE('',*,*,#8970,.T.);
#12508=ORIENTED_EDGE('',*,*,#9003,.F.);
#12509=ORIENTED_EDGE('',*,*,#9009,.F.);
#12510=ORIENTED_EDGE('',*,*,#9010,.F.);
#12511=ORIENTED_EDGE('',*,*,#9011,.F.);
#12512=ORIENTED_EDGE('',*,*,#8872,.F.);
#12513=ORIENTED_EDGE('',*,*,#9012,.F.);
#12514=ORIENTED_EDGE('',*,*,#8921,.F.);
#12515=ORIENTED_EDGE('',*,*,#8994,.F.);
#12516=ORIENTED_EDGE('',*,*,#8927,.F.);
#12517=ORIENTED_EDGE('',*,*,#8992,.F.);
#12518=ORIENTED_EDGE('',*,*,#8896,.F.);
#12519=ORIENTED_EDGE('',*,*,#9013,.F.);
#12520=ORIENTED_EDGE('',*,*,#8973,.T.);
#12521=ORIENTED_EDGE('',*,*,#8928,.T.);
#12522=ORIENTED_EDGE('',*,*,#9013,.T.);
#12523=ORIENTED_EDGE('',*,*,#8895,.F.);
#12524=ORIENTED_EDGE('',*,*,#8902,.F.);
#12525=ORIENTED_EDGE('',*,*,#8969,.F.);
#12526=ORIENTED_EDGE('',*,*,#9014,.F.);
#12527=ORIENTED_EDGE('',*,*,#9015,.T.);
#12528=ORIENTED_EDGE('',*,*,#9016,.T.);
#12529=ORIENTED_EDGE('',*,*,#9017,.F.);
#12530=ORIENTED_EDGE('',*,*,#9010,.T.);
#12531=ORIENTED_EDGE('',*,*,#9018,.F.);
#12532=ORIENTED_EDGE('',*,*,#8997,.T.);
#12533=ORIENTED_EDGE('',*,*,#9000,.T.);
#12534=ORIENTED_EDGE('',*,*,#8923,.T.);
#12535=ORIENTED_EDGE('',*,*,#8922,.T.);
#12536=ORIENTED_EDGE('',*,*,#9012,.T.);
#12537=ORIENTED_EDGE('',*,*,#8871,.F.);
#12538=ORIENTED_EDGE('',*,*,#8884,.F.);
#12539=ORIENTED_EDGE('',*,*,#8980,.F.);
#12540=ORIENTED_EDGE('',*,*,#9004,.F.);
#12541=ORIENTED_EDGE('',*,*,#9011,.T.);
#12542=ORIENTED_EDGE('',*,*,#9017,.T.);
#12543=ORIENTED_EDGE('',*,*,#8919,.F.);
#12544=ORIENTED_EDGE('',*,*,#9005,.F.);
#12545=ORIENTED_EDGE('',*,*,#8874,.F.);
#12546=ORIENTED_EDGE('',*,*,#8993,.F.);
#12547=ORIENTED_EDGE('',*,*,#9018,.T.);
#12548=ORIENTED_EDGE('',*,*,#9009,.T.);
#12549=ORIENTED_EDGE('',*,*,#9002,.T.);
#12550=ORIENTED_EDGE('',*,*,#8998,.T.);
#12551=ORIENTED_EDGE('',*,*,#8976,.T.);
#12552=ORIENTED_EDGE('',*,*,#9019,.T.);
#12553=ORIENTED_EDGE('',*,*,#8886,.T.);
#12554=ORIENTED_EDGE('',*,*,#9020,.T.);
#12555=ORIENTED_EDGE('',*,*,#9021,.F.);
#12556=ORIENTED_EDGE('',*,*,#9022,.F.);
#12557=ORIENTED_EDGE('',*,*,#9023,.F.);
#12558=ORIENTED_EDGE('',*,*,#9015,.F.);
#12559=ORIENTED_EDGE('',*,*,#9024,.F.);
#12560=ORIENTED_EDGE('',*,*,#9025,.T.);
#12561=ORIENTED_EDGE('',*,*,#9026,.F.);
#12562=ORIENTED_EDGE('',*,*,#9022,.T.);
#12563=ORIENTED_EDGE('',*,*,#9026,.T.);
#12564=ORIENTED_EDGE('',*,*,#9027,.T.);
#12565=ORIENTED_EDGE('',*,*,#9006,.T.);
#12566=ORIENTED_EDGE('',*,*,#8978,.F.);
#12567=ORIENTED_EDGE('',*,*,#9028,.T.);
#12568=ORIENTED_EDGE('',*,*,#9029,.T.);
#12569=ORIENTED_EDGE('',*,*,#9030,.F.);
#12570=ORIENTED_EDGE('',*,*,#8974,.F.);
#12571=ORIENTED_EDGE('',*,*,#9016,.F.);
#12572=ORIENTED_EDGE('',*,*,#9023,.T.);
#12573=ORIENTED_EDGE('',*,*,#9029,.F.);
#12574=ORIENTED_EDGE('',*,*,#9031,.F.);
#12575=ORIENTED_EDGE('',*,*,#9032,.F.);
#12576=ORIENTED_EDGE('',*,*,#9033,.F.);
#12577=ORIENTED_EDGE('',*,*,#8977,.F.);
#12578=ORIENTED_EDGE('',*,*,#9020,.F.);
#12579=ORIENTED_EDGE('',*,*,#8885,.T.);
#12580=ORIENTED_EDGE('',*,*,#8880,.T.);
#12581=ORIENTED_EDGE('',*,*,#8972,.T.);
#12582=ORIENTED_EDGE('',*,*,#9034,.T.);
#12583=ORIENTED_EDGE('',*,*,#9031,.T.);
#12584=ORIENTED_EDGE('',*,*,#9028,.F.);
#12585=ORIENTED_EDGE('',*,*,#9008,.F.);
#12586=ORIENTED_EDGE('',*,*,#9035,.T.);
#12587=ORIENTED_EDGE('',*,*,#9024,.T.);
#12588=ORIENTED_EDGE('',*,*,#9021,.T.);
#12589=ORIENTED_EDGE('',*,*,#9014,.T.);
#12590=ORIENTED_EDGE('',*,*,#8968,.F.);
#12591=ORIENTED_EDGE('',*,*,#9036,.T.);
#12592=ORIENTED_EDGE('',*,*,#9032,.T.);
#12593=ORIENTED_EDGE('',*,*,#9034,.F.);
#12594=ORIENTED_EDGE('',*,*,#8971,.F.);
#12595=ORIENTED_EDGE('',*,*,#8887,.F.);
#12596=ORIENTED_EDGE('',*,*,#9019,.F.);
#12597=ORIENTED_EDGE('',*,*,#8975,.T.);
#12598=ORIENTED_EDGE('',*,*,#9030,.T.);
#12599=ORIENTED_EDGE('',*,*,#9033,.T.);
#12600=ORIENTED_EDGE('',*,*,#9036,.F.);
#12601=ORIENTED_EDGE('',*,*,#8967,.F.);
#12602=ORIENTED_EDGE('',*,*,#8900,.F.);
#12603=ORIENTED_EDGE('',*,*,#9027,.F.);
#12604=ORIENTED_EDGE('',*,*,#9025,.F.);
#12605=ORIENTED_EDGE('',*,*,#9035,.F.);
#12606=ORIENTED_EDGE('',*,*,#9007,.F.);
#12607=ORIENTED_EDGE('',*,*,#8963,.T.);
#12608=ORIENTED_EDGE('',*,*,#9037,.T.);
#12609=ORIENTED_EDGE('',*,*,#8989,.T.);
#12610=ORIENTED_EDGE('',*,*,#9038,.T.);
#12611=ORIENTED_EDGE('',*,*,#9039,.F.);
#12612=ORIENTED_EDGE('',*,*,#9040,.F.);
#12613=ORIENTED_EDGE('',*,*,#9041,.F.);
#12614=ORIENTED_EDGE('',*,*,#9042,.F.);
#12615=ORIENTED_EDGE('',*,*,#9043,.F.);
#12616=ORIENTED_EDGE('',*,*,#9044,.T.);
#12617=ORIENTED_EDGE('',*,*,#9045,.F.);
#12618=ORIENTED_EDGE('',*,*,#9040,.T.);
#12619=ORIENTED_EDGE('',*,*,#9045,.T.);
#12620=ORIENTED_EDGE('',*,*,#9046,.T.);
#12621=ORIENTED_EDGE('',*,*,#9047,.T.);
#12622=ORIENTED_EDGE('',*,*,#8965,.F.);
#12623=ORIENTED_EDGE('',*,*,#9048,.T.);
#12624=ORIENTED_EDGE('',*,*,#9049,.T.);
#12625=ORIENTED_EDGE('',*,*,#9050,.F.);
#12626=ORIENTED_EDGE('',*,*,#8961,.F.);
#12627=ORIENTED_EDGE('',*,*,#9051,.F.);
#12628=ORIENTED_EDGE('',*,*,#9041,.T.);
#12629=ORIENTED_EDGE('',*,*,#9049,.F.);
#12630=ORIENTED_EDGE('',*,*,#9052,.F.);
#12631=ORIENTED_EDGE('',*,*,#9053,.F.);
#12632=ORIENTED_EDGE('',*,*,#9054,.F.);
#12633=ORIENTED_EDGE('',*,*,#8964,.F.);
#12634=ORIENTED_EDGE('',*,*,#9038,.F.);
#12635=ORIENTED_EDGE('',*,*,#8988,.T.);
#12636=ORIENTED_EDGE('',*,*,#8905,.T.);
#12637=ORIENTED_EDGE('',*,*,#8959,.T.);
#12638=ORIENTED_EDGE('',*,*,#9055,.T.);
#12639=ORIENTED_EDGE('',*,*,#9052,.T.);
#12640=ORIENTED_EDGE('',*,*,#9048,.F.);
#12641=ORIENTED_EDGE('',*,*,#9056,.F.);
#12642=ORIENTED_EDGE('',*,*,#9057,.T.);
#12643=ORIENTED_EDGE('',*,*,#9043,.T.);
#12644=ORIENTED_EDGE('',*,*,#9039,.T.);
#12645=ORIENTED_EDGE('',*,*,#9058,.T.);
#12646=ORIENTED_EDGE('',*,*,#8955,.F.);
#12647=ORIENTED_EDGE('',*,*,#9059,.T.);
#12648=ORIENTED_EDGE('',*,*,#9053,.T.);
#12649=ORIENTED_EDGE('',*,*,#9055,.F.);
#12650=ORIENTED_EDGE('',*,*,#8958,.F.);
#12651=ORIENTED_EDGE('',*,*,#9047,.F.);
#12652=ORIENTED_EDGE('',*,*,#9060,.T.);
#12653=ORIENTED_EDGE('',*,*,#9056,.T.);
#12654=ORIENTED_EDGE('',*,*,#8957,.T.);
#12655=ORIENTED_EDGE('',*,*,#8903,.T.);
#12656=ORIENTED_EDGE('',*,*,#8893,.T.);
#12657=ORIENTED_EDGE('',*,*,#9061,.T.);
#12658=ORIENTED_EDGE('',*,*,#8930,.F.);
#12659=ORIENTED_EDGE('',*,*,#8966,.F.);
#12660=ORIENTED_EDGE('',*,*,#9058,.F.);
#12661=ORIENTED_EDGE('',*,*,#9042,.T.);
#12662=ORIENTED_EDGE('',*,*,#9051,.T.);
#12663=ORIENTED_EDGE('',*,*,#8960,.T.);
#12664=ORIENTED_EDGE('',*,*,#8940,.T.);
#12665=ORIENTED_EDGE('',*,*,#9062,.T.);
#12666=ORIENTED_EDGE('',*,*,#8908,.F.);
#12667=ORIENTED_EDGE('',*,*,#8916,.F.);
#12668=ORIENTED_EDGE('',*,*,#8956,.F.);
#12669=ORIENTED_EDGE('',*,*,#8990,.F.);
#12670=ORIENTED_EDGE('',*,*,#9037,.F.);
#12671=ORIENTED_EDGE('',*,*,#8962,.T.);
#12672=ORIENTED_EDGE('',*,*,#9050,.T.);
#12673=ORIENTED_EDGE('',*,*,#9054,.T.);
#12674=ORIENTED_EDGE('',*,*,#9059,.F.);
#12675=ORIENTED_EDGE('',*,*,#8954,.F.);
#12676=ORIENTED_EDGE('',*,*,#8914,.F.);
#12677=ORIENTED_EDGE('',*,*,#9046,.F.);
#12678=ORIENTED_EDGE('',*,*,#9044,.F.);
#12679=ORIENTED_EDGE('',*,*,#9057,.F.);
#12680=ORIENTED_EDGE('',*,*,#9060,.F.);
#12681=ORIENTED_EDGE('',*,*,#8938,.F.);
#12682=ORIENTED_EDGE('',*,*,#9063,.T.);
#12683=ORIENTED_EDGE('',*,*,#8910,.F.);
#12684=ORIENTED_EDGE('',*,*,#9064,.T.);
#12685=ORIENTED_EDGE('',*,*,#8932,.T.);
#12686=ORIENTED_EDGE('',*,*,#9065,.T.);
#12687=ORIENTED_EDGE('',*,*,#8891,.T.);
#12688=ORIENTED_EDGE('',*,*,#9066,.T.);
#12689=ORIENTED_EDGE('',*,*,#9067,.F.);
#12690=ORIENTED_EDGE('',*,*,#9068,.F.);
#12691=ORIENTED_EDGE('',*,*,#9069,.F.);
#12692=ORIENTED_EDGE('',*,*,#9070,.F.);
#12693=ORIENTED_EDGE('',*,*,#8986,.T.);
#12694=ORIENTED_EDGE('',*,*,#8912,.T.);
#12695=ORIENTED_EDGE('',*,*,#9071,.T.);
#12696=ORIENTED_EDGE('',*,*,#8936,.F.);
#12697=ORIENTED_EDGE('',*,*,#9072,.F.);
#12698=ORIENTED_EDGE('',*,*,#9068,.T.);
#12699=ORIENTED_EDGE('',*,*,#9073,.T.);
#12700=ORIENTED_EDGE('',*,*,#8952,.T.);
#12701=ORIENTED_EDGE('',*,*,#9074,.F.);
#12702=ORIENTED_EDGE('',*,*,#9075,.T.);
#12703=ORIENTED_EDGE('',*,*,#9076,.T.);
#12704=ORIENTED_EDGE('',*,*,#8953,.T.);
#12705=ORIENTED_EDGE('',*,*,#9073,.F.);
#12706=ORIENTED_EDGE('',*,*,#9067,.T.);
#12707=ORIENTED_EDGE('',*,*,#8911,.F.);
#12708=ORIENTED_EDGE('',*,*,#9063,.F.);
#12709=ORIENTED_EDGE('',*,*,#8937,.F.);
#12710=ORIENTED_EDGE('',*,*,#9071,.F.);
#12711=ORIENTED_EDGE('',*,*,#9075,.F.);
#12712=ORIENTED_EDGE('',*,*,#9077,.F.);
#12713=ORIENTED_EDGE('',*,*,#9078,.F.);
#12714=ORIENTED_EDGE('',*,*,#9079,.F.);
#12715=ORIENTED_EDGE('',*,*,#8890,.F.);
#12716=ORIENTED_EDGE('',*,*,#9080,.F.);
#12717=ORIENTED_EDGE('',*,*,#8933,.F.);
#12718=ORIENTED_EDGE('',*,*,#9066,.F.);
#12719=ORIENTED_EDGE('',*,*,#8939,.F.);
#12720=ORIENTED_EDGE('',*,*,#9064,.F.);
#12721=ORIENTED_EDGE('',*,*,#8909,.F.);
#12722=ORIENTED_EDGE('',*,*,#9062,.F.);
#12723=ORIENTED_EDGE('',*,*,#9081,.F.);
#12724=ORIENTED_EDGE('',*,*,#9078,.T.);
#12725=ORIENTED_EDGE('',*,*,#9082,.F.);
#12726=ORIENTED_EDGE('',*,*,#9069,.T.);
#12727=ORIENTED_EDGE('',*,*,#9072,.T.);
#12728=ORIENTED_EDGE('',*,*,#8935,.T.);
#12729=ORIENTED_EDGE('',*,*,#8934,.T.);
#12730=ORIENTED_EDGE('',*,*,#9080,.T.);
#12731=ORIENTED_EDGE('',*,*,#8889,.F.);
#12732=ORIENTED_EDGE('',*,*,#8987,.F.);
#12733=ORIENTED_EDGE('',*,*,#8950,.F.);
#12734=ORIENTED_EDGE('',*,*,#9076,.F.);
#12735=ORIENTED_EDGE('',*,*,#9079,.T.);
#12736=ORIENTED_EDGE('',*,*,#9081,.T.);
#12737=ORIENTED_EDGE('',*,*,#8931,.F.);
#12738=ORIENTED_EDGE('',*,*,#9061,.F.);
#12739=ORIENTED_EDGE('',*,*,#8892,.F.);
#12740=ORIENTED_EDGE('',*,*,#9065,.F.);
#12741=ORIENTED_EDGE('',*,*,#9082,.T.);
#12742=ORIENTED_EDGE('',*,*,#9077,.T.);
#12743=ORIENTED_EDGE('',*,*,#9074,.T.);
#12744=ORIENTED_EDGE('',*,*,#9070,.T.);
#12745=ORIENTED_EDGE('',*,*,#8949,.F.);
#12746=ORIENTED_EDGE('',*,*,#8944,.F.);
#12747=ORIENTED_EDGE('',*,*,#8947,.T.);
#12748=ORIENTED_EDGE('',*,*,#8985,.T.);
#12749=ORIENTED_EDGE('',*,*,#8946,.F.);
#12750=ORIENTED_EDGE('',*,*,#8943,.F.);
#12751=ORIENTED_EDGE('',*,*,#9083,.T.);
#12752=ORIENTED_EDGE('',*,*,#9084,.F.);
#12753=ORIENTED_EDGE('',*,*,#9085,.F.);
#12754=ORIENTED_EDGE('',*,*,#9086,.T.);
#12755=ORIENTED_EDGE('',*,*,#9087,.T.);
#12756=ORIENTED_EDGE('',*,*,#9088,.F.);
#12757=ORIENTED_EDGE('',*,*,#9089,.F.);
#12758=ORIENTED_EDGE('',*,*,#9084,.T.);
#12759=ORIENTED_EDGE('',*,*,#9090,.T.);
#12760=ORIENTED_EDGE('',*,*,#9091,.T.);
#12761=ORIENTED_EDGE('',*,*,#9092,.F.);
#12762=ORIENTED_EDGE('',*,*,#9093,.T.);
#12763=ORIENTED_EDGE('',*,*,#9094,.F.);
#12764=ORIENTED_EDGE('',*,*,#9095,.F.);
#12765=ORIENTED_EDGE('',*,*,#9096,.F.);
#12766=ORIENTED_EDGE('',*,*,#9093,.F.);
#12767=ORIENTED_EDGE('',*,*,#9097,.F.);
#12768=ORIENTED_EDGE('',*,*,#9098,.T.);
#12769=ORIENTED_EDGE('',*,*,#9099,.T.);
#12770=ORIENTED_EDGE('',*,*,#9095,.T.);
#12771=ORIENTED_EDGE('',*,*,#9100,.F.);
#12772=ORIENTED_EDGE('',*,*,#9101,.F.);
#12773=ORIENTED_EDGE('',*,*,#9102,.F.);
#12774=ORIENTED_EDGE('',*,*,#9098,.F.);
#12775=ORIENTED_EDGE('',*,*,#9103,.T.);
#12776=ORIENTED_EDGE('',*,*,#9101,.T.);
#12777=ORIENTED_EDGE('',*,*,#9104,.F.);
#12778=ORIENTED_EDGE('',*,*,#9105,.T.);
#12779=ORIENTED_EDGE('',*,*,#9092,.T.);
#12780=ORIENTED_EDGE('',*,*,#9106,.T.);
#12781=ORIENTED_EDGE('',*,*,#9107,.T.);
#12782=ORIENTED_EDGE('',*,*,#9108,.T.);
#12783=ORIENTED_EDGE('',*,*,#9104,.T.);
#12784=ORIENTED_EDGE('',*,*,#9100,.T.);
#12785=ORIENTED_EDGE('',*,*,#9097,.T.);
#12786=ORIENTED_EDGE('',*,*,#9094,.T.);
#12787=ORIENTED_EDGE('',*,*,#8941,.T.);
#12788=ORIENTED_EDGE('',*,*,#9108,.F.);
#12789=ORIENTED_EDGE('',*,*,#9109,.F.);
#12790=ORIENTED_EDGE('',*,*,#9110,.F.);
#12791=ORIENTED_EDGE('',*,*,#9105,.F.);
#12792=ORIENTED_EDGE('',*,*,#9111,.F.);
#12793=ORIENTED_EDGE('',*,*,#9112,.T.);
#12794=ORIENTED_EDGE('',*,*,#9090,.F.);
#12795=ORIENTED_EDGE('',*,*,#9096,.T.);
#12796=ORIENTED_EDGE('',*,*,#9099,.F.);
#12797=ORIENTED_EDGE('',*,*,#9102,.T.);
#12798=ORIENTED_EDGE('',*,*,#9103,.F.);
#12799=ORIENTED_EDGE('',*,*,#9110,.T.);
#12800=ORIENTED_EDGE('',*,*,#9113,.F.);
#12801=ORIENTED_EDGE('',*,*,#9087,.F.);
#12802=ORIENTED_EDGE('',*,*,#9083,.F.);
#12803=ORIENTED_EDGE('',*,*,#9114,.F.);
#12804=ORIENTED_EDGE('',*,*,#9107,.F.);
#12805=ORIENTED_EDGE('',*,*,#9115,.T.);
#12806=ORIENTED_EDGE('',*,*,#9111,.T.);
#12807=ORIENTED_EDGE('',*,*,#9109,.T.);
#12808=ORIENTED_EDGE('',*,*,#9113,.T.);
#12809=ORIENTED_EDGE('',*,*,#9116,.F.);
#12810=ORIENTED_EDGE('',*,*,#9117,.F.);
#12811=ORIENTED_EDGE('',*,*,#9088,.T.);
#12812=ORIENTED_EDGE('',*,*,#9117,.T.);
#12813=ORIENTED_EDGE('',*,*,#9118,.T.);
#12814=ORIENTED_EDGE('',*,*,#9085,.T.);
#12815=ORIENTED_EDGE('',*,*,#9089,.T.);
#12816=ORIENTED_EDGE('',*,*,#8906,.T.);
#12817=ORIENTED_EDGE('',*,*,#9114,.T.);
#12818=ORIENTED_EDGE('',*,*,#9086,.F.);
#12819=ORIENTED_EDGE('',*,*,#9118,.F.);
#12820=ORIENTED_EDGE('',*,*,#9116,.T.);
#12821=ORIENTED_EDGE('',*,*,#9106,.F.);
#12822=ORIENTED_EDGE('',*,*,#9091,.F.);
#12823=ORIENTED_EDGE('',*,*,#9112,.F.);
#12824=ORIENTED_EDGE('',*,*,#9115,.F.);
#12825=ORIENTED_EDGE('',*,*,#9119,.F.);
#12826=ORIENTED_EDGE('',*,*,#9120,.T.);
#12827=ORIENTED_EDGE('',*,*,#9121,.F.);
#12828=ORIENTED_EDGE('',*,*,#9120,.F.);
#12829=ORIENTED_EDGE('',*,*,#9122,.F.);
#12830=ORIENTED_EDGE('',*,*,#9123,.F.);
#12831=ORIENTED_EDGE('',*,*,#9124,.T.);
#12832=ORIENTED_EDGE('',*,*,#9123,.T.);
#12833=ORIENTED_EDGE('',*,*,#9125,.F.);
#12834=ORIENTED_EDGE('',*,*,#9126,.F.);
#12835=ORIENTED_EDGE('',*,*,#9127,.F.);
#12836=ORIENTED_EDGE('',*,*,#9128,.F.);
#12837=ORIENTED_EDGE('',*,*,#9129,.F.);
#12838=ORIENTED_EDGE('',*,*,#9130,.F.);
#12839=ORIENTED_EDGE('',*,*,#9131,.F.);
#12840=ORIENTED_EDGE('',*,*,#9132,.F.);
#12841=ORIENTED_EDGE('',*,*,#9133,.F.);
#12842=ORIENTED_EDGE('',*,*,#9134,.T.);
#12843=ORIENTED_EDGE('',*,*,#9135,.T.);
#12844=ORIENTED_EDGE('',*,*,#9136,.F.);
#12845=ORIENTED_EDGE('',*,*,#9137,.F.);
#12846=ORIENTED_EDGE('',*,*,#9136,.T.);
#12847=ORIENTED_EDGE('',*,*,#9125,.T.);
#12848=ORIENTED_EDGE('',*,*,#9122,.T.);
#12849=ORIENTED_EDGE('',*,*,#9119,.T.);
#12850=ORIENTED_EDGE('',*,*,#9138,.T.);
#12851=ORIENTED_EDGE('',*,*,#9139,.T.);
#12852=ORIENTED_EDGE('',*,*,#9140,.T.);
#12853=ORIENTED_EDGE('',*,*,#9139,.F.);
#12854=ORIENTED_EDGE('',*,*,#9141,.F.);
#12855=ORIENTED_EDGE('',*,*,#9142,.T.);
#12856=ORIENTED_EDGE('',*,*,#9127,.T.);
#12857=ORIENTED_EDGE('',*,*,#9126,.T.);
#12858=ORIENTED_EDGE('',*,*,#9142,.F.);
#12859=ORIENTED_EDGE('',*,*,#9143,.T.);
#12860=ORIENTED_EDGE('',*,*,#9144,.T.);
#12861=ORIENTED_EDGE('',*,*,#9145,.F.);
#12862=ORIENTED_EDGE('',*,*,#9144,.F.);
#12863=ORIENTED_EDGE('',*,*,#9146,.T.);
#12864=ORIENTED_EDGE('',*,*,#9147,.T.);
#12865=ORIENTED_EDGE('',*,*,#9148,.T.);
#12866=ORIENTED_EDGE('',*,*,#9147,.F.);
#12867=ORIENTED_EDGE('',*,*,#9149,.T.);
#12868=ORIENTED_EDGE('',*,*,#9150,.T.);
#12869=ORIENTED_EDGE('',*,*,#9151,.F.);
#12870=ORIENTED_EDGE('',*,*,#9150,.F.);
#12871=ORIENTED_EDGE('',*,*,#9152,.T.);
#12872=ORIENTED_EDGE('',*,*,#9153,.T.);
#12873=ORIENTED_EDGE('',*,*,#9154,.F.);
#12874=ORIENTED_EDGE('',*,*,#9153,.F.);
#12875=ORIENTED_EDGE('',*,*,#9155,.T.);
#12876=ORIENTED_EDGE('',*,*,#9156,.F.);
#12877=ORIENTED_EDGE('',*,*,#9157,.F.);
#12878=ORIENTED_EDGE('',*,*,#9158,.T.);
#12879=ORIENTED_EDGE('',*,*,#9159,.F.);
#12880=ORIENTED_EDGE('',*,*,#9160,.T.);
#12881=ORIENTED_EDGE('',*,*,#9161,.F.);
#12882=ORIENTED_EDGE('',*,*,#9160,.F.);
#12883=ORIENTED_EDGE('',*,*,#9162,.F.);
#12884=ORIENTED_EDGE('',*,*,#9163,.T.);
#12885=ORIENTED_EDGE('',*,*,#9164,.T.);
#12886=ORIENTED_EDGE('',*,*,#9163,.F.);
#12887=ORIENTED_EDGE('',*,*,#9159,.T.);
#12888=ORIENTED_EDGE('',*,*,#9165,.T.);
#12889=ORIENTED_EDGE('',*,*,#9166,.F.);
#12890=ORIENTED_EDGE('',*,*,#9165,.F.);
#12891=ORIENTED_EDGE('',*,*,#9167,.F.);
#12892=ORIENTED_EDGE('',*,*,#9168,.T.);
#12893=ORIENTED_EDGE('',*,*,#9169,.T.);
#12894=ORIENTED_EDGE('',*,*,#9168,.F.);
#12895=ORIENTED_EDGE('',*,*,#9161,.T.);
#12896=ORIENTED_EDGE('',*,*,#9167,.T.);
#12897=ORIENTED_EDGE('',*,*,#9169,.F.);
#12898=ORIENTED_EDGE('',*,*,#9164,.F.);
#12899=ORIENTED_EDGE('',*,*,#9137,.T.);
#12900=ORIENTED_EDGE('',*,*,#9162,.T.);
#12901=ORIENTED_EDGE('',*,*,#9170,.T.);
#12902=ORIENTED_EDGE('',*,*,#9158,.F.);
#12903=ORIENTED_EDGE('',*,*,#9171,.F.);
#12904=ORIENTED_EDGE('',*,*,#9172,.T.);
#12905=ORIENTED_EDGE('',*,*,#9173,.F.);
#12906=ORIENTED_EDGE('',*,*,#9174,.F.);
#12907=ORIENTED_EDGE('',*,*,#9175,.T.);
#12908=ORIENTED_EDGE('',*,*,#9176,.T.);
#12909=ORIENTED_EDGE('',*,*,#9177,.F.);
#12910=ORIENTED_EDGE('',*,*,#9176,.F.);
#12911=ORIENTED_EDGE('',*,*,#9178,.T.);
#12912=ORIENTED_EDGE('',*,*,#9179,.T.);
#12913=ORIENTED_EDGE('',*,*,#9180,.F.);
#12914=ORIENTED_EDGE('',*,*,#9179,.F.);
#12915=ORIENTED_EDGE('',*,*,#9181,.T.);
#12916=ORIENTED_EDGE('',*,*,#9182,.T.);
#12917=ORIENTED_EDGE('',*,*,#9183,.T.);
#12918=ORIENTED_EDGE('',*,*,#9184,.T.);
#12919=ORIENTED_EDGE('',*,*,#9185,.F.);
#12920=ORIENTED_EDGE('',*,*,#9186,.F.);
#12921=ORIENTED_EDGE('',*,*,#9156,.T.);
#12922=ORIENTED_EDGE('',*,*,#9187,.F.);
#12923=ORIENTED_EDGE('',*,*,#9135,.F.);
#12924=ORIENTED_EDGE('',*,*,#9188,.T.);
#12925=ORIENTED_EDGE('',*,*,#9189,.T.);
#12926=ORIENTED_EDGE('',*,*,#9190,.F.);
#12927=ORIENTED_EDGE('',*,*,#9189,.F.);
#12928=ORIENTED_EDGE('',*,*,#9191,.T.);
#12929=ORIENTED_EDGE('',*,*,#9192,.T.);
#12930=ORIENTED_EDGE('',*,*,#9193,.F.);
#12931=ORIENTED_EDGE('',*,*,#9192,.F.);
#12932=ORIENTED_EDGE('',*,*,#9194,.T.);
#12933=ORIENTED_EDGE('',*,*,#9195,.T.);
#12934=ORIENTED_EDGE('',*,*,#9196,.F.);
#12935=ORIENTED_EDGE('',*,*,#9195,.F.);
#12936=ORIENTED_EDGE('',*,*,#9197,.T.);
#12937=ORIENTED_EDGE('',*,*,#9198,.T.);
#12938=ORIENTED_EDGE('',*,*,#9199,.F.);
#12939=ORIENTED_EDGE('',*,*,#9198,.F.);
#12940=ORIENTED_EDGE('',*,*,#9200,.T.);
#12941=ORIENTED_EDGE('',*,*,#9201,.T.);
#12942=ORIENTED_EDGE('',*,*,#9202,.F.);
#12943=ORIENTED_EDGE('',*,*,#9203,.F.);
#12944=ORIENTED_EDGE('',*,*,#9201,.F.);
#12945=ORIENTED_EDGE('',*,*,#9204,.T.);
#12946=ORIENTED_EDGE('',*,*,#9205,.F.);
#12947=ORIENTED_EDGE('',*,*,#9206,.F.);
#12948=ORIENTED_EDGE('',*,*,#9207,.F.);
#12949=ORIENTED_EDGE('',*,*,#9208,.F.);
#12950=ORIENTED_EDGE('',*,*,#9209,.F.);
#12951=ORIENTED_EDGE('',*,*,#9210,.F.);
#12952=ORIENTED_EDGE('',*,*,#9211,.T.);
#12953=ORIENTED_EDGE('',*,*,#9212,.T.);
#12954=ORIENTED_EDGE('',*,*,#9166,.T.);
#12955=ORIENTED_EDGE('',*,*,#9213,.F.);
#12956=ORIENTED_EDGE('',*,*,#9204,.F.);
#12957=ORIENTED_EDGE('',*,*,#9200,.F.);
#12958=ORIENTED_EDGE('',*,*,#9197,.F.);
#12959=ORIENTED_EDGE('',*,*,#9194,.F.);
#12960=ORIENTED_EDGE('',*,*,#9191,.F.);
#12961=ORIENTED_EDGE('',*,*,#9188,.F.);
#12962=ORIENTED_EDGE('',*,*,#9134,.F.);
#12963=ORIENTED_EDGE('',*,*,#9214,.F.);
#12964=ORIENTED_EDGE('',*,*,#9215,.T.);
#12965=ORIENTED_EDGE('',*,*,#9216,.F.);
#12966=ORIENTED_EDGE('',*,*,#9121,.T.);
#12967=ORIENTED_EDGE('',*,*,#9138,.F.);
#12968=ORIENTED_EDGE('',*,*,#9146,.F.);
#12969=ORIENTED_EDGE('',*,*,#9217,.F.);
#12970=ORIENTED_EDGE('',*,*,#9218,.T.);
#12971=ORIENTED_EDGE('',*,*,#9214,.T.);
#12972=ORIENTED_EDGE('',*,*,#9133,.T.);
#12973=ORIENTED_EDGE('',*,*,#9219,.T.);
#12974=ORIENTED_EDGE('',*,*,#9130,.T.);
#12975=ORIENTED_EDGE('',*,*,#9220,.F.);
#12976=ORIENTED_EDGE('',*,*,#9205,.T.);
#12977=ORIENTED_EDGE('',*,*,#9221,.F.);
#12978=ORIENTED_EDGE('',*,*,#9216,.T.);
#12979=ORIENTED_EDGE('',*,*,#9141,.T.);
#12980=ORIENTED_EDGE('',*,*,#9143,.F.);
#12981=ORIENTED_EDGE('',*,*,#9222,.F.);
#12982=ORIENTED_EDGE('',*,*,#9131,.T.);
#12983=ORIENTED_EDGE('',*,*,#9219,.F.);
#12984=ORIENTED_EDGE('',*,*,#9215,.F.);
#12985=ORIENTED_EDGE('',*,*,#9218,.F.);
#12986=ORIENTED_EDGE('',*,*,#9223,.F.);
#12987=ORIENTED_EDGE('',*,*,#9212,.F.);
#12988=ORIENTED_EDGE('',*,*,#9224,.F.);
#12989=ORIENTED_EDGE('',*,*,#9225,.F.);
#12990=ORIENTED_EDGE('',*,*,#9226,.F.);
#12991=ORIENTED_EDGE('',*,*,#9226,.T.);
#12992=ORIENTED_EDGE('',*,*,#9227,.F.);
#12993=ORIENTED_EDGE('',*,*,#9228,.F.);
#12994=ORIENTED_EDGE('',*,*,#9229,.F.);
#12995=ORIENTED_EDGE('',*,*,#9230,.T.);
#12996=ORIENTED_EDGE('',*,*,#9225,.T.);
#12997=ORIENTED_EDGE('',*,*,#9231,.F.);
#12998=ORIENTED_EDGE('',*,*,#9227,.T.);
#12999=ORIENTED_EDGE('',*,*,#9232,.T.);
#13000=ORIENTED_EDGE('',*,*,#9233,.F.);
#13001=ORIENTED_EDGE('',*,*,#9234,.F.);
#13002=ORIENTED_EDGE('',*,*,#9235,.T.);
#13003=ORIENTED_EDGE('',*,*,#9186,.T.);
#13004=ORIENTED_EDGE('',*,*,#9236,.T.);
#13005=ORIENTED_EDGE('',*,*,#9234,.T.);
#13006=ORIENTED_EDGE('',*,*,#9237,.T.);
#13007=ORIENTED_EDGE('',*,*,#9238,.T.);
#13008=ORIENTED_EDGE('',*,*,#9239,.T.);
#13009=ORIENTED_EDGE('',*,*,#9171,.T.);
#13010=ORIENTED_EDGE('',*,*,#9157,.T.);
#13011=ORIENTED_EDGE('',*,*,#9152,.F.);
#13012=ORIENTED_EDGE('',*,*,#9149,.F.);
#13013=ORIENTED_EDGE('',*,*,#9124,.F.);
#13014=ORIENTED_EDGE('',*,*,#9240,.T.);
#13015=ORIENTED_EDGE('',*,*,#9241,.T.);
#13016=ORIENTED_EDGE('',*,*,#9172,.F.);
#13017=ORIENTED_EDGE('',*,*,#9239,.F.);
#13018=ORIENTED_EDGE('',*,*,#9242,.T.);
#13019=ORIENTED_EDGE('',*,*,#9240,.F.);
#13020=ORIENTED_EDGE('',*,*,#9243,.F.);
#13021=ORIENTED_EDGE('',*,*,#9244,.F.);
#13022=ORIENTED_EDGE('',*,*,#9182,.F.);
#13023=ORIENTED_EDGE('',*,*,#9245,.F.);
#13024=ORIENTED_EDGE('',*,*,#9246,.T.);
#13025=ORIENTED_EDGE('',*,*,#9173,.T.);
#13026=ORIENTED_EDGE('',*,*,#9177,.T.);
#13027=ORIENTED_EDGE('',*,*,#9180,.T.);
#13028=ORIENTED_EDGE('',*,*,#9247,.T.);
#13029=ORIENTED_EDGE('',*,*,#9248,.T.);
#13030=ORIENTED_EDGE('',*,*,#9209,.T.);
#13031=ORIENTED_EDGE('',*,*,#9223,.T.);
#13032=ORIENTED_EDGE('',*,*,#9217,.T.);
#13033=ORIENTED_EDGE('',*,*,#9132,.T.);
#13034=ORIENTED_EDGE('',*,*,#9187,.T.);
#13035=ORIENTED_EDGE('',*,*,#9190,.T.);
#13036=ORIENTED_EDGE('',*,*,#9193,.T.);
#13037=ORIENTED_EDGE('',*,*,#9196,.T.);
#13038=ORIENTED_EDGE('',*,*,#9199,.T.);
#13039=ORIENTED_EDGE('',*,*,#9203,.T.);
#13040=ORIENTED_EDGE('',*,*,#9140,.F.);
#13041=ORIENTED_EDGE('',*,*,#9148,.F.);
#13042=ORIENTED_EDGE('',*,*,#9248,.F.);
#13043=ORIENTED_EDGE('',*,*,#9249,.F.);
#13044=ORIENTED_EDGE('',*,*,#9250,.T.);
#13045=ORIENTED_EDGE('',*,*,#9210,.T.);
#13046=ORIENTED_EDGE('',*,*,#9247,.F.);
#13047=ORIENTED_EDGE('',*,*,#9183,.F.);
#13048=ORIENTED_EDGE('',*,*,#9244,.T.);
#13049=ORIENTED_EDGE('',*,*,#9251,.T.);
#13050=ORIENTED_EDGE('',*,*,#9249,.T.);
#13051=ORIENTED_EDGE('',*,*,#9224,.T.);
#13052=ORIENTED_EDGE('',*,*,#9211,.F.);
#13053=ORIENTED_EDGE('',*,*,#9250,.F.);
#13054=ORIENTED_EDGE('',*,*,#9251,.F.);
#13055=ORIENTED_EDGE('',*,*,#9252,.F.);
#13056=ORIENTED_EDGE('',*,*,#9253,.F.);
#13057=ORIENTED_EDGE('',*,*,#9232,.F.);
#13058=ORIENTED_EDGE('',*,*,#9254,.F.);
#13059=ORIENTED_EDGE('',*,*,#9154,.T.);
#13060=ORIENTED_EDGE('',*,*,#9252,.T.);
#13061=ORIENTED_EDGE('',*,*,#9243,.T.);
#13062=ORIENTED_EDGE('',*,*,#9242,.F.);
#13063=ORIENTED_EDGE('',*,*,#9238,.F.);
#13064=ORIENTED_EDGE('',*,*,#9255,.T.);
#13065=ORIENTED_EDGE('',*,*,#9253,.T.);
#13066=ORIENTED_EDGE('',*,*,#9255,.F.);
#13067=ORIENTED_EDGE('',*,*,#9237,.F.);
#13068=ORIENTED_EDGE('',*,*,#9233,.T.);
#13069=ORIENTED_EDGE('',*,*,#9256,.T.);
#13070=ORIENTED_EDGE('',*,*,#9128,.T.);
#13071=ORIENTED_EDGE('',*,*,#9222,.T.);
#13072=ORIENTED_EDGE('',*,*,#9230,.F.);
#13073=ORIENTED_EDGE('',*,*,#9257,.F.);
#13074=ORIENTED_EDGE('',*,*,#9207,.T.);
#13075=ORIENTED_EDGE('',*,*,#9145,.T.);
#13076=ORIENTED_EDGE('',*,*,#9220,.T.);
#13077=ORIENTED_EDGE('',*,*,#9129,.T.);
#13078=ORIENTED_EDGE('',*,*,#9256,.F.);
#13079=ORIENTED_EDGE('',*,*,#9206,.T.);
#13080=ORIENTED_EDGE('',*,*,#9181,.F.);
#13081=ORIENTED_EDGE('',*,*,#9178,.F.);
#13082=ORIENTED_EDGE('',*,*,#9175,.F.);
#13083=ORIENTED_EDGE('',*,*,#9258,.F.);
#13084=ORIENTED_EDGE('',*,*,#9259,.F.);
#13085=ORIENTED_EDGE('',*,*,#9184,.F.);
#13086=ORIENTED_EDGE('',*,*,#9155,.F.);
#13087=ORIENTED_EDGE('',*,*,#9170,.F.);
#13088=ORIENTED_EDGE('',*,*,#9241,.F.);
#13089=ORIENTED_EDGE('',*,*,#9151,.T.);
#13090=ORIENTED_EDGE('',*,*,#9246,.F.);
#13091=ORIENTED_EDGE('',*,*,#9260,.F.);
#13092=ORIENTED_EDGE('',*,*,#9258,.T.);
#13093=ORIENTED_EDGE('',*,*,#9174,.T.);
#13094=ORIENTED_EDGE('',*,*,#9221,.T.);
#13095=ORIENTED_EDGE('',*,*,#9208,.T.);
#13096=ORIENTED_EDGE('',*,*,#9257,.T.);
#13097=ORIENTED_EDGE('',*,*,#9229,.T.);
#13098=ORIENTED_EDGE('',*,*,#9261,.T.);
#13099=ORIENTED_EDGE('',*,*,#9260,.T.);
#13100=ORIENTED_EDGE('',*,*,#9245,.T.);
#13101=ORIENTED_EDGE('',*,*,#9202,.T.);
#13102=ORIENTED_EDGE('',*,*,#9213,.T.);
#13103=ORIENTED_EDGE('',*,*,#9228,.T.);
#13104=ORIENTED_EDGE('',*,*,#9262,.F.);
#13105=ORIENTED_EDGE('',*,*,#9261,.F.);
#13106=ORIENTED_EDGE('',*,*,#9259,.T.);
#13107=ORIENTED_EDGE('',*,*,#9262,.T.);
#13108=ORIENTED_EDGE('',*,*,#9231,.T.);
#13109=ORIENTED_EDGE('',*,*,#9254,.T.);
#13110=ORIENTED_EDGE('',*,*,#9235,.F.);
#13111=ORIENTED_EDGE('',*,*,#9236,.F.);
#13112=ORIENTED_EDGE('',*,*,#9185,.T.);
#13113=ORIENTED_EDGE('',*,*,#9263,.F.);
#13114=ORIENTED_EDGE('',*,*,#9264,.F.);
#13115=ORIENTED_EDGE('',*,*,#9265,.F.);
#13116=ORIENTED_EDGE('',*,*,#9266,.F.);
#13117=ORIENTED_EDGE('',*,*,#9267,.F.);
#13118=ORIENTED_EDGE('',*,*,#9268,.F.);
#13119=ORIENTED_EDGE('',*,*,#9269,.T.);
#13120=ORIENTED_EDGE('',*,*,#9270,.T.);
#13121=ORIENTED_EDGE('',*,*,#9271,.T.);
#13122=ORIENTED_EDGE('',*,*,#9270,.F.);
#13123=ORIENTED_EDGE('',*,*,#9272,.T.);
#13124=ORIENTED_EDGE('',*,*,#9273,.T.);
#13125=ORIENTED_EDGE('',*,*,#9274,.T.);
#13126=ORIENTED_EDGE('',*,*,#9275,.T.);
#13127=ORIENTED_EDGE('',*,*,#9276,.T.);
#13128=ORIENTED_EDGE('',*,*,#9277,.T.);
#13129=ORIENTED_EDGE('',*,*,#9278,.T.);
#13130=ORIENTED_EDGE('',*,*,#9279,.T.);
#13131=ORIENTED_EDGE('',*,*,#9280,.T.);
#13132=ORIENTED_EDGE('',*,*,#9281,.T.);
#13133=ORIENTED_EDGE('',*,*,#9282,.T.);
#13134=ORIENTED_EDGE('',*,*,#9277,.F.);
#13135=ORIENTED_EDGE('',*,*,#9283,.T.);
#13136=ORIENTED_EDGE('',*,*,#9284,.T.);
#13137=ORIENTED_EDGE('',*,*,#9285,.T.);
#13138=ORIENTED_EDGE('',*,*,#9286,.F.);
#13139=ORIENTED_EDGE('',*,*,#9287,.F.);
#13140=ORIENTED_EDGE('',*,*,#9278,.F.);
#13141=ORIENTED_EDGE('',*,*,#9282,.F.);
#13142=ORIENTED_EDGE('',*,*,#9288,.F.);
#13143=ORIENTED_EDGE('',*,*,#9289,.T.);
#13144=ORIENTED_EDGE('',*,*,#9290,.T.);
#13145=ORIENTED_EDGE('',*,*,#9291,.T.);
#13146=ORIENTED_EDGE('',*,*,#9292,.T.);
#13147=ORIENTED_EDGE('',*,*,#9293,.T.);
#13148=ORIENTED_EDGE('',*,*,#9294,.T.);
#13149=ORIENTED_EDGE('',*,*,#9295,.T.);
#13150=ORIENTED_EDGE('',*,*,#9296,.T.);
#13151=ORIENTED_EDGE('',*,*,#9297,.T.);
#13152=ORIENTED_EDGE('',*,*,#9290,.F.);
#13153=ORIENTED_EDGE('',*,*,#9298,.F.);
#13154=ORIENTED_EDGE('',*,*,#9299,.T.);
#13155=ORIENTED_EDGE('',*,*,#9289,.F.);
#13156=ORIENTED_EDGE('',*,*,#9299,.F.);
#13157=ORIENTED_EDGE('',*,*,#9300,.T.);
#13158=ORIENTED_EDGE('',*,*,#9301,.T.);
#13159=ORIENTED_EDGE('',*,*,#9302,.T.);
#13160=ORIENTED_EDGE('',*,*,#9303,.T.);
#13161=ORIENTED_EDGE('',*,*,#9304,.T.);
#13162=ORIENTED_EDGE('',*,*,#9305,.T.);
#13163=ORIENTED_EDGE('',*,*,#9306,.T.);
#13164=ORIENTED_EDGE('',*,*,#9307,.T.);
#13165=ORIENTED_EDGE('',*,*,#9308,.T.);
#13166=ORIENTED_EDGE('',*,*,#9309,.T.);
#13167=ORIENTED_EDGE('',*,*,#9310,.F.);
#13168=ORIENTED_EDGE('',*,*,#9311,.F.);
#13169=ORIENTED_EDGE('',*,*,#9312,.T.);
#13170=ORIENTED_EDGE('',*,*,#9313,.T.);
#13171=ORIENTED_EDGE('',*,*,#9314,.T.);
#13172=ORIENTED_EDGE('',*,*,#9315,.T.);
#13173=ORIENTED_EDGE('',*,*,#9316,.T.);
#13174=ORIENTED_EDGE('',*,*,#9317,.T.);
#13175=ORIENTED_EDGE('',*,*,#9318,.T.);
#13176=ORIENTED_EDGE('',*,*,#9301,.F.);
#13177=ORIENTED_EDGE('',*,*,#9319,.T.);
#13178=ORIENTED_EDGE('',*,*,#9320,.T.);
#13179=ORIENTED_EDGE('',*,*,#9321,.T.);
#13180=ORIENTED_EDGE('',*,*,#9322,.T.);
#13181=ORIENTED_EDGE('',*,*,#9323,.T.);
#13182=ORIENTED_EDGE('',*,*,#9324,.T.);
#13183=ORIENTED_EDGE('',*,*,#9325,.T.);
#13184=ORIENTED_EDGE('',*,*,#9326,.T.);
#13185=ORIENTED_EDGE('',*,*,#9327,.T.);
#13186=ORIENTED_EDGE('',*,*,#9328,.T.);
#13187=ORIENTED_EDGE('',*,*,#9329,.T.);
#13188=ORIENTED_EDGE('',*,*,#9330,.T.);
#13189=ORIENTED_EDGE('',*,*,#9331,.T.);
#13190=ORIENTED_EDGE('',*,*,#9271,.F.);
#13191=ORIENTED_EDGE('',*,*,#9331,.F.);
#13192=ORIENTED_EDGE('',*,*,#9332,.T.);
#13193=ORIENTED_EDGE('',*,*,#9333,.T.);
#13194=ORIENTED_EDGE('',*,*,#9334,.T.);
#13195=ORIENTED_EDGE('',*,*,#9335,.T.);
#13196=ORIENTED_EDGE('',*,*,#9336,.T.);
#13197=ORIENTED_EDGE('',*,*,#9337,.T.);
#13198=ORIENTED_EDGE('',*,*,#9338,.T.);
#13199=ORIENTED_EDGE('',*,*,#9339,.T.);
#13200=ORIENTED_EDGE('',*,*,#9340,.F.);
#13201=ORIENTED_EDGE('',*,*,#9341,.F.);
#13202=ORIENTED_EDGE('',*,*,#9342,.F.);
#13203=ORIENTED_EDGE('',*,*,#9343,.F.);
#13204=ORIENTED_EDGE('',*,*,#9269,.F.);
#13205=ORIENTED_EDGE('',*,*,#9344,.T.);
#13206=ORIENTED_EDGE('',*,*,#9345,.F.);
#13207=ORIENTED_EDGE('',*,*,#9344,.F.);
#13208=ORIENTED_EDGE('',*,*,#9329,.F.);
#13209=ORIENTED_EDGE('',*,*,#9346,.T.);
#13210=ORIENTED_EDGE('',*,*,#9347,.F.);
#13211=ORIENTED_EDGE('',*,*,#9348,.F.);
#13212=ORIENTED_EDGE('',*,*,#9349,.F.);
#13213=ORIENTED_EDGE('',*,*,#9300,.F.);
#13214=ORIENTED_EDGE('',*,*,#9350,.F.);
#13215=ORIENTED_EDGE('',*,*,#9351,.F.);
#13216=ORIENTED_EDGE('',*,*,#9352,.T.);
#13217=ORIENTED_EDGE('',*,*,#9319,.F.);
#13218=ORIENTED_EDGE('',*,*,#9353,.F.);
#13219=ORIENTED_EDGE('',*,*,#9354,.T.);
#13220=ORIENTED_EDGE('',*,*,#9347,.T.);
#13221=ORIENTED_EDGE('',*,*,#9355,.T.);
#13222=ORIENTED_EDGE('',*,*,#9356,.T.);
#13223=ORIENTED_EDGE('',*,*,#9348,.T.);
#13224=ORIENTED_EDGE('',*,*,#9354,.F.);
#13225=ORIENTED_EDGE('',*,*,#9357,.T.);
#13226=ORIENTED_EDGE('',*,*,#9358,.T.);
#13227=ORIENTED_EDGE('',*,*,#9359,.T.);
#13228=ORIENTED_EDGE('',*,*,#9360,.T.);
#13229=ORIENTED_EDGE('',*,*,#9361,.T.);
#13230=ORIENTED_EDGE('',*,*,#9362,.T.);
#13231=ORIENTED_EDGE('',*,*,#9363,.F.);
#13232=ORIENTED_EDGE('',*,*,#9364,.F.);
#13233=ORIENTED_EDGE('',*,*,#9365,.T.);
#13234=ORIENTED_EDGE('',*,*,#9366,.F.);
#13235=ORIENTED_EDGE('',*,*,#9367,.T.);
#13236=ORIENTED_EDGE('',*,*,#9368,.T.);
#13237=ORIENTED_EDGE('',*,*,#9369,.F.);
#13238=ORIENTED_EDGE('',*,*,#9368,.F.);
#13239=ORIENTED_EDGE('',*,*,#9370,.T.);
#13240=ORIENTED_EDGE('',*,*,#9371,.T.);
#13241=ORIENTED_EDGE('',*,*,#9372,.T.);
#13242=ORIENTED_EDGE('',*,*,#9373,.T.);
#13243=ORIENTED_EDGE('',*,*,#9325,.F.);
#13244=ORIENTED_EDGE('',*,*,#9374,.T.);
#13245=ORIENTED_EDGE('',*,*,#9375,.F.);
#13246=ORIENTED_EDGE('',*,*,#9376,.F.);
#13247=ORIENTED_EDGE('',*,*,#9377,.F.);
#13248=ORIENTED_EDGE('',*,*,#9378,.F.);
#13249=ORIENTED_EDGE('',*,*,#9379,.T.);
#13250=ORIENTED_EDGE('',*,*,#9380,.F.);
#13251=ORIENTED_EDGE('',*,*,#9381,.F.);
#13252=ORIENTED_EDGE('',*,*,#9382,.F.);
#13253=ORIENTED_EDGE('',*,*,#9383,.T.);
#13254=ORIENTED_EDGE('',*,*,#9384,.F.);
#13255=ORIENTED_EDGE('',*,*,#9385,.T.);
#13256=ORIENTED_EDGE('',*,*,#9386,.T.);
#13257=ORIENTED_EDGE('',*,*,#9387,.T.);
#13258=ORIENTED_EDGE('',*,*,#9388,.T.);
#13259=ORIENTED_EDGE('',*,*,#9389,.T.);
#13260=ORIENTED_EDGE('',*,*,#9389,.F.);
#13261=ORIENTED_EDGE('',*,*,#9390,.F.);
#13262=ORIENTED_EDGE('',*,*,#9391,.F.);
#13263=ORIENTED_EDGE('',*,*,#9392,.F.);
#13264=ORIENTED_EDGE('',*,*,#9298,.T.);
#13265=ORIENTED_EDGE('',*,*,#9393,.T.);
#13266=ORIENTED_EDGE('',*,*,#9345,.T.);
#13267=ORIENTED_EDGE('',*,*,#9393,.F.);
#13268=ORIENTED_EDGE('',*,*,#9318,.F.);
#13269=ORIENTED_EDGE('',*,*,#9394,.T.);
#13270=ORIENTED_EDGE('',*,*,#9291,.F.);
#13271=ORIENTED_EDGE('',*,*,#9297,.F.);
#13272=ORIENTED_EDGE('',*,*,#9395,.T.);
#13273=ORIENTED_EDGE('',*,*,#9396,.T.);
#13274=ORIENTED_EDGE('',*,*,#9302,.F.);
#13275=ORIENTED_EDGE('',*,*,#9397,.T.);
#13276=ORIENTED_EDGE('',*,*,#9398,.T.);
#13277=ORIENTED_EDGE('',*,*,#9399,.F.);
#13278=ORIENTED_EDGE('',*,*,#9400,.F.);
#13279=ORIENTED_EDGE('',*,*,#9401,.T.);
#13280=ORIENTED_EDGE('',*,*,#9402,.F.);
#13281=ORIENTED_EDGE('',*,*,#9403,.F.);
#13282=ORIENTED_EDGE('',*,*,#9404,.T.);
#13283=ORIENTED_EDGE('',*,*,#9405,.T.);
#13284=ORIENTED_EDGE('',*,*,#9406,.T.);
#13285=ORIENTED_EDGE('',*,*,#9407,.F.);
#13286=ORIENTED_EDGE('',*,*,#9378,.T.);
#13287=ORIENTED_EDGE('',*,*,#9408,.F.);
#13288=ORIENTED_EDGE('',*,*,#9409,.F.);
#13289=ORIENTED_EDGE('',*,*,#9410,.T.);
#13290=ORIENTED_EDGE('',*,*,#9408,.T.);
#13291=ORIENTED_EDGE('',*,*,#9411,.T.);
#13292=ORIENTED_EDGE('',*,*,#9412,.T.);
#13293=ORIENTED_EDGE('',*,*,#9400,.T.);
#13294=ORIENTED_EDGE('',*,*,#9413,.T.);
#13295=ORIENTED_EDGE('',*,*,#9375,.T.);
#13296=ORIENTED_EDGE('',*,*,#9414,.T.);
#13297=ORIENTED_EDGE('',*,*,#9415,.T.);
#13298=ORIENTED_EDGE('',*,*,#9416,.F.);
#13299=ORIENTED_EDGE('',*,*,#9406,.F.);
#13300=ORIENTED_EDGE('',*,*,#9417,.F.);
#13301=ORIENTED_EDGE('',*,*,#9418,.F.);
#13302=ORIENTED_EDGE('',*,*,#9415,.F.);
#13303=ORIENTED_EDGE('',*,*,#9419,.T.);
#13304=ORIENTED_EDGE('',*,*,#9376,.T.);
#13305=ORIENTED_EDGE('',*,*,#9420,.F.);
#13306=ORIENTED_EDGE('',*,*,#9421,.T.);
#13307=ORIENTED_EDGE('',*,*,#9422,.F.);
#13308=ORIENTED_EDGE('',*,*,#9423,.T.);
#13309=ORIENTED_EDGE('',*,*,#9424,.T.);
#13310=ORIENTED_EDGE('',*,*,#9423,.F.);
#13311=ORIENTED_EDGE('',*,*,#9425,.T.);
#13312=ORIENTED_EDGE('',*,*,#9426,.T.);
#13313=ORIENTED_EDGE('',*,*,#9427,.F.);
#13314=ORIENTED_EDGE('',*,*,#9426,.F.);
#13315=ORIENTED_EDGE('',*,*,#9428,.T.);
#13316=ORIENTED_EDGE('',*,*,#9429,.T.);
#13317=ORIENTED_EDGE('',*,*,#9430,.F.);
#13318=ORIENTED_EDGE('',*,*,#9429,.F.);
#13319=ORIENTED_EDGE('',*,*,#9431,.T.);
#13320=ORIENTED_EDGE('',*,*,#9432,.F.);
#13321=ORIENTED_EDGE('',*,*,#9433,.T.);
#13322=ORIENTED_EDGE('',*,*,#9434,.T.);
#13323=ORIENTED_EDGE('',*,*,#9435,.F.);
#13324=ORIENTED_EDGE('',*,*,#9436,.F.);
#13325=ORIENTED_EDGE('',*,*,#9437,.F.);
#13326=ORIENTED_EDGE('',*,*,#9438,.T.);
#13327=ORIENTED_EDGE('',*,*,#9439,.F.);
#13328=ORIENTED_EDGE('',*,*,#9440,.F.);
#13329=ORIENTED_EDGE('',*,*,#9441,.F.);
#13330=ORIENTED_EDGE('',*,*,#9440,.T.);
#13331=ORIENTED_EDGE('',*,*,#9442,.T.);
#13332=ORIENTED_EDGE('',*,*,#9443,.F.);
#13333=ORIENTED_EDGE('',*,*,#9444,.F.);
#13334=ORIENTED_EDGE('',*,*,#9445,.F.);
#13335=ORIENTED_EDGE('',*,*,#9385,.F.);
#13336=ORIENTED_EDGE('',*,*,#9446,.F.);
#13337=ORIENTED_EDGE('',*,*,#9434,.F.);
#13338=ORIENTED_EDGE('',*,*,#9447,.T.);
#13339=ORIENTED_EDGE('',*,*,#9448,.T.);
#13340=ORIENTED_EDGE('',*,*,#9449,.F.);
#13341=ORIENTED_EDGE('',*,*,#9450,.T.);
#13342=ORIENTED_EDGE('',*,*,#9451,.F.);
#13343=ORIENTED_EDGE('',*,*,#9450,.F.);
#13344=ORIENTED_EDGE('',*,*,#9452,.T.);
#13345=ORIENTED_EDGE('',*,*,#9453,.T.);
#13346=ORIENTED_EDGE('',*,*,#9454,.T.);
#13347=ORIENTED_EDGE('',*,*,#9455,.F.);
#13348=ORIENTED_EDGE('',*,*,#9456,.T.);
#13349=ORIENTED_EDGE('',*,*,#9457,.F.);
#13350=ORIENTED_EDGE('',*,*,#9458,.F.);
#13351=ORIENTED_EDGE('',*,*,#9459,.F.);
#13352=ORIENTED_EDGE('',*,*,#9460,.T.);
#13353=ORIENTED_EDGE('',*,*,#9461,.T.);
#13354=ORIENTED_EDGE('',*,*,#9462,.F.);
#13355=ORIENTED_EDGE('',*,*,#9463,.F.);
#13356=ORIENTED_EDGE('',*,*,#9464,.T.);
#13357=ORIENTED_EDGE('',*,*,#9372,.F.);
#13358=ORIENTED_EDGE('',*,*,#9373,.F.);
#13359=ORIENTED_EDGE('',*,*,#9464,.F.);
#13360=ORIENTED_EDGE('',*,*,#9370,.F.);
#13361=ORIENTED_EDGE('',*,*,#9371,.F.);
#13362=ORIENTED_EDGE('',*,*,#9465,.T.);
#13363=ORIENTED_EDGE('',*,*,#9466,.T.);
#13364=ORIENTED_EDGE('',*,*,#9465,.F.);
#13365=ORIENTED_EDGE('',*,*,#9340,.T.);
#13366=ORIENTED_EDGE('',*,*,#9467,.F.);
#13367=ORIENTED_EDGE('',*,*,#9468,.T.);
#13368=ORIENTED_EDGE('',*,*,#9469,.T.);
#13369=ORIENTED_EDGE('',*,*,#9470,.T.);
#13370=ORIENTED_EDGE('',*,*,#9471,.T.);
#13371=ORIENTED_EDGE('',*,*,#9472,.F.);
#13372=ORIENTED_EDGE('',*,*,#9471,.F.);
#13373=ORIENTED_EDGE('',*,*,#9473,.T.);
#13374=ORIENTED_EDGE('',*,*,#9474,.F.);
#13375=ORIENTED_EDGE('',*,*,#9475,.F.);
#13376=ORIENTED_EDGE('',*,*,#9334,.F.);
#13377=ORIENTED_EDGE('',*,*,#9476,.F.);
#13378=ORIENTED_EDGE('',*,*,#9477,.T.);
#13379=ORIENTED_EDGE('',*,*,#9478,.F.);
#13380=ORIENTED_EDGE('',*,*,#9477,.F.);
#13381=ORIENTED_EDGE('',*,*,#9367,.F.);
#13382=ORIENTED_EDGE('',*,*,#9479,.T.);
#13383=ORIENTED_EDGE('',*,*,#9480,.T.);
#13384=ORIENTED_EDGE('',*,*,#9479,.F.);
#13385=ORIENTED_EDGE('',*,*,#9480,.F.);
#13386=ORIENTED_EDGE('',*,*,#9481,.T.);
#13387=ORIENTED_EDGE('',*,*,#9482,.T.);
#13388=ORIENTED_EDGE('',*,*,#9481,.F.);
#13389=ORIENTED_EDGE('',*,*,#9482,.F.);
#13390=ORIENTED_EDGE('',*,*,#9483,.T.);
#13391=ORIENTED_EDGE('',*,*,#9430,.T.);
#13392=ORIENTED_EDGE('',*,*,#9483,.F.);
#13393=ORIENTED_EDGE('',*,*,#9484,.T.);
#13394=ORIENTED_EDGE('',*,*,#9485,.T.);
#13395=ORIENTED_EDGE('',*,*,#9486,.F.);
#13396=ORIENTED_EDGE('',*,*,#9485,.F.);
#13397=ORIENTED_EDGE('',*,*,#9487,.F.);
#13398=ORIENTED_EDGE('',*,*,#9488,.T.);
#13399=ORIENTED_EDGE('',*,*,#9489,.T.);
#13400=ORIENTED_EDGE('',*,*,#9488,.F.);
#13401=ORIENTED_EDGE('',*,*,#9424,.F.);
#13402=ORIENTED_EDGE('',*,*,#9489,.F.);
#13403=ORIENTED_EDGE('',*,*,#9476,.T.);
#13404=ORIENTED_EDGE('',*,*,#9360,.F.);
#13405=ORIENTED_EDGE('',*,*,#9490,.T.);
#13406=ORIENTED_EDGE('',*,*,#9491,.F.);
#13407=ORIENTED_EDGE('',*,*,#9492,.F.);
#13408=ORIENTED_EDGE('',*,*,#9493,.F.);
#13409=ORIENTED_EDGE('',*,*,#9494,.T.);
#13410=ORIENTED_EDGE('',*,*,#9362,.F.);
#13411=ORIENTED_EDGE('',*,*,#9495,.F.);
#13412=ORIENTED_EDGE('',*,*,#9496,.T.);
#13413=ORIENTED_EDGE('',*,*,#9497,.T.);
#13414=ORIENTED_EDGE('',*,*,#9469,.F.);
#13415=ORIENTED_EDGE('',*,*,#9498,.T.);
#13416=ORIENTED_EDGE('',*,*,#9499,.T.);
#13417=ORIENTED_EDGE('',*,*,#9500,.T.);
#13418=ORIENTED_EDGE('',*,*,#9496,.F.);
#13419=ORIENTED_EDGE('',*,*,#9501,.T.);
#13420=ORIENTED_EDGE('',*,*,#9502,.F.);
#13421=ORIENTED_EDGE('',*,*,#9503,.F.);
#13422=ORIENTED_EDGE('',*,*,#9501,.F.);
#13423=ORIENTED_EDGE('',*,*,#9498,.F.);
#13424=ORIENTED_EDGE('',*,*,#9468,.F.);
#13425=ORIENTED_EDGE('',*,*,#9504,.F.);
#13426=ORIENTED_EDGE('',*,*,#9505,.F.);
#13427=ORIENTED_EDGE('',*,*,#9506,.F.);
#13428=ORIENTED_EDGE('',*,*,#9486,.T.);
#13429=ORIENTED_EDGE('',*,*,#9472,.T.);
#13430=ORIENTED_EDGE('',*,*,#9369,.T.);
#13431=ORIENTED_EDGE('',*,*,#9507,.T.);
#13432=ORIENTED_EDGE('',*,*,#9508,.T.);
#13433=ORIENTED_EDGE('',*,*,#9499,.F.);
#13434=ORIENTED_EDGE('',*,*,#9503,.T.);
#13435=ORIENTED_EDGE('',*,*,#9509,.T.);
#13436=ORIENTED_EDGE('',*,*,#9510,.T.);
#13437=ORIENTED_EDGE('',*,*,#9507,.F.);
#13438=ORIENTED_EDGE('',*,*,#9502,.T.);
#13439=ORIENTED_EDGE('',*,*,#9511,.T.);
#13440=ORIENTED_EDGE('',*,*,#9512,.T.);
#13441=ORIENTED_EDGE('',*,*,#9509,.F.);
#13442=ORIENTED_EDGE('',*,*,#9506,.T.);
#13443=ORIENTED_EDGE('',*,*,#9513,.T.);
#13444=ORIENTED_EDGE('',*,*,#9514,.T.);
#13445=ORIENTED_EDGE('',*,*,#9511,.F.);
#13446=ORIENTED_EDGE('',*,*,#9505,.T.);
#13447=ORIENTED_EDGE('',*,*,#9515,.T.);
#13448=ORIENTED_EDGE('',*,*,#9286,.T.);
#13449=ORIENTED_EDGE('',*,*,#9516,.F.);
#13450=ORIENTED_EDGE('',*,*,#9517,.F.);
#13451=ORIENTED_EDGE('',*,*,#9267,.T.);
#13452=ORIENTED_EDGE('',*,*,#9266,.T.);
#13453=ORIENTED_EDGE('',*,*,#9454,.F.);
#13454=ORIENTED_EDGE('',*,*,#9518,.F.);
#13455=ORIENTED_EDGE('',*,*,#9264,.T.);
#13456=ORIENTED_EDGE('',*,*,#9519,.F.);
#13457=ORIENTED_EDGE('',*,*,#9275,.F.);
#13458=ORIENTED_EDGE('',*,*,#9520,.F.);
#13459=ORIENTED_EDGE('',*,*,#9460,.F.);
#13460=ORIENTED_EDGE('',*,*,#9520,.T.);
#13461=ORIENTED_EDGE('',*,*,#9274,.F.);
#13462=ORIENTED_EDGE('',*,*,#9521,.T.);
#13463=ORIENTED_EDGE('',*,*,#9461,.F.);
#13464=ORIENTED_EDGE('',*,*,#9522,.T.);
#13465=ORIENTED_EDGE('',*,*,#9523,.F.);
#13466=ORIENTED_EDGE('',*,*,#9521,.F.);
#13467=ORIENTED_EDGE('',*,*,#9273,.F.);
#13468=ORIENTED_EDGE('',*,*,#9524,.T.);
#13469=ORIENTED_EDGE('',*,*,#9525,.F.);
#13470=ORIENTED_EDGE('',*,*,#9522,.F.);
#13471=ORIENTED_EDGE('',*,*,#9526,.F.);
#13472=ORIENTED_EDGE('',*,*,#9527,.T.);
#13473=ORIENTED_EDGE('',*,*,#9528,.F.);
#13474=ORIENTED_EDGE('',*,*,#9524,.F.);
#13475=ORIENTED_EDGE('',*,*,#9316,.F.);
#13476=ORIENTED_EDGE('',*,*,#9315,.F.);
#13477=ORIENTED_EDGE('',*,*,#9516,.T.);
#13478=ORIENTED_EDGE('',*,*,#9453,.F.);
#13479=ORIENTED_EDGE('',*,*,#9452,.F.);
#13480=ORIENTED_EDGE('',*,*,#9527,.F.);
#13481=ORIENTED_EDGE('',*,*,#9456,.F.);
#13482=ORIENTED_EDGE('',*,*,#9458,.T.);
#13483=ORIENTED_EDGE('',*,*,#9449,.T.);
#13484=ORIENTED_EDGE('',*,*,#9529,.F.);
#13485=ORIENTED_EDGE('',*,*,#9514,.F.);
#13486=ORIENTED_EDGE('',*,*,#9530,.F.);
#13487=ORIENTED_EDGE('',*,*,#9531,.F.);
#13488=ORIENTED_EDGE('',*,*,#9532,.T.);
#13489=ORIENTED_EDGE('',*,*,#9533,.T.);
#13490=ORIENTED_EDGE('',*,*,#9534,.F.);
#13491=ORIENTED_EDGE('',*,*,#9366,.T.);
#13492=ORIENTED_EDGE('',*,*,#9535,.F.);
#13493=ORIENTED_EDGE('',*,*,#9532,.F.);
#13494=ORIENTED_EDGE('',*,*,#9536,.F.);
#13495=ORIENTED_EDGE('',*,*,#9537,.T.);
#13496=ORIENTED_EDGE('',*,*,#9538,.F.);
#13497=ORIENTED_EDGE('',*,*,#9533,.F.);
#13498=ORIENTED_EDGE('',*,*,#9539,.F.);
#13499=ORIENTED_EDGE('',*,*,#9540,.T.);
#13500=ORIENTED_EDGE('',*,*,#9541,.T.);
#13501=ORIENTED_EDGE('',*,*,#9542,.F.);
#13502=ORIENTED_EDGE('',*,*,#9543,.T.);
#13503=ORIENTED_EDGE('',*,*,#9544,.F.);
#13504=ORIENTED_EDGE('',*,*,#9540,.F.);
#13505=ORIENTED_EDGE('',*,*,#9545,.F.);
#13506=ORIENTED_EDGE('',*,*,#9546,.F.);
#13507=ORIENTED_EDGE('',*,*,#9547,.F.);
#13508=ORIENTED_EDGE('',*,*,#9541,.F.);
#13509=ORIENTED_EDGE('',*,*,#9548,.F.);
#13510=ORIENTED_EDGE('',*,*,#9549,.T.);
#13511=ORIENTED_EDGE('',*,*,#9550,.T.);
#13512=ORIENTED_EDGE('',*,*,#9543,.F.);
#13513=ORIENTED_EDGE('',*,*,#9551,.T.);
#13514=ORIENTED_EDGE('',*,*,#9552,.F.);
#13515=ORIENTED_EDGE('',*,*,#9549,.F.);
#13516=ORIENTED_EDGE('',*,*,#9553,.F.);
#13517=ORIENTED_EDGE('',*,*,#9554,.F.);
#13518=ORIENTED_EDGE('',*,*,#9555,.F.);
#13519=ORIENTED_EDGE('',*,*,#9550,.F.);
#13520=ORIENTED_EDGE('',*,*,#9556,.F.);
#13521=ORIENTED_EDGE('',*,*,#9557,.T.);
#13522=ORIENTED_EDGE('',*,*,#9558,.T.);
#13523=ORIENTED_EDGE('',*,*,#9551,.F.);
#13524=ORIENTED_EDGE('',*,*,#9559,.F.);
#13525=ORIENTED_EDGE('',*,*,#9560,.F.);
#13526=ORIENTED_EDGE('',*,*,#9557,.F.);
#13527=ORIENTED_EDGE('',*,*,#9561,.F.);
#13528=ORIENTED_EDGE('',*,*,#9562,.F.);
#13529=ORIENTED_EDGE('',*,*,#9563,.T.);
#13530=ORIENTED_EDGE('',*,*,#9564,.F.);
#13531=ORIENTED_EDGE('',*,*,#9447,.F.);
#13532=ORIENTED_EDGE('',*,*,#9565,.F.);
#13533=ORIENTED_EDGE('',*,*,#9566,.T.);
#13534=ORIENTED_EDGE('',*,*,#9567,.F.);
#13535=ORIENTED_EDGE('',*,*,#9565,.T.);
#13536=ORIENTED_EDGE('',*,*,#9568,.F.);
#13537=ORIENTED_EDGE('',*,*,#9448,.F.);
#13538=ORIENTED_EDGE('',*,*,#9569,.F.);
#13539=ORIENTED_EDGE('',*,*,#9570,.T.);
#13540=ORIENTED_EDGE('',*,*,#9571,.F.);
#13541=ORIENTED_EDGE('',*,*,#9572,.F.);
#13542=ORIENTED_EDGE('',*,*,#9573,.F.);
#13543=ORIENTED_EDGE('',*,*,#9570,.F.);
#13544=ORIENTED_EDGE('',*,*,#9574,.T.);
#13545=ORIENTED_EDGE('',*,*,#9575,.F.);
#13546=ORIENTED_EDGE('',*,*,#9567,.T.);
#13547=ORIENTED_EDGE('',*,*,#9576,.F.);
#13548=ORIENTED_EDGE('',*,*,#9574,.F.);
#13549=ORIENTED_EDGE('',*,*,#9577,.F.);
#13550=ORIENTED_EDGE('',*,*,#9575,.T.);
#13551=ORIENTED_EDGE('',*,*,#9578,.F.);
#13552=ORIENTED_EDGE('',*,*,#9579,.F.);
#13553=ORIENTED_EDGE('',*,*,#9580,.F.);
#13554=ORIENTED_EDGE('',*,*,#9581,.T.);
#13555=ORIENTED_EDGE('',*,*,#9582,.F.);
#13556=ORIENTED_EDGE('',*,*,#9442,.F.);
#13557=ORIENTED_EDGE('',*,*,#9583,.F.);
#13558=ORIENTED_EDGE('',*,*,#9579,.T.);
#13559=ORIENTED_EDGE('',*,*,#9584,.T.);
#13560=ORIENTED_EDGE('',*,*,#9581,.F.);
#13561=ORIENTED_EDGE('',*,*,#9444,.T.);
#13562=ORIENTED_EDGE('',*,*,#9585,.F.);
#13563=ORIENTED_EDGE('',*,*,#9584,.F.);
#13564=ORIENTED_EDGE('',*,*,#9586,.F.);
#13565=ORIENTED_EDGE('',*,*,#9566,.F.);
#13566=ORIENTED_EDGE('',*,*,#9587,.F.);
#13567=ORIENTED_EDGE('',*,*,#9588,.T.);
#13568=ORIENTED_EDGE('',*,*,#9589,.F.);
#13569=ORIENTED_EDGE('',*,*,#9436,.T.);
#13570=ORIENTED_EDGE('',*,*,#9572,.T.);
#13571=ORIENTED_EDGE('',*,*,#9438,.F.);
#13572=ORIENTED_EDGE('',*,*,#9391,.T.);
#13573=ORIENTED_EDGE('',*,*,#9590,.F.);
#13574=ORIENTED_EDGE('',*,*,#9591,.F.);
#13575=ORIENTED_EDGE('',*,*,#9592,.F.);
#13576=ORIENTED_EDGE('',*,*,#9593,.T.);
#13577=ORIENTED_EDGE('',*,*,#9591,.T.);
#13578=ORIENTED_EDGE('',*,*,#9594,.F.);
#13579=ORIENTED_EDGE('',*,*,#9595,.T.);
#13580=ORIENTED_EDGE('',*,*,#9596,.F.);
#13581=ORIENTED_EDGE('',*,*,#9593,.F.);
#13582=ORIENTED_EDGE('',*,*,#9597,.F.);
#13583=ORIENTED_EDGE('',*,*,#9534,.T.);
#13584=ORIENTED_EDGE('',*,*,#9598,.F.);
#13585=ORIENTED_EDGE('',*,*,#9433,.F.);
#13586=ORIENTED_EDGE('',*,*,#9599,.F.);
#13587=ORIENTED_EDGE('',*,*,#9594,.T.);
#13588=ORIENTED_EDGE('',*,*,#9600,.F.);
#13589=ORIENTED_EDGE('',*,*,#9431,.F.);
#13590=ORIENTED_EDGE('',*,*,#9601,.F.);
#13591=ORIENTED_EDGE('',*,*,#9432,.T.);
#13592=ORIENTED_EDGE('',*,*,#9602,.F.);
#13593=ORIENTED_EDGE('',*,*,#9603,.F.);
#13594=ORIENTED_EDGE('',*,*,#9604,.F.);
#13595=ORIENTED_EDGE('',*,*,#9544,.T.);
#13596=ORIENTED_EDGE('',*,*,#9555,.T.);
#13597=ORIENTED_EDGE('',*,*,#9605,.F.);
#13598=ORIENTED_EDGE('',*,*,#9548,.T.);
#13599=ORIENTED_EDGE('',*,*,#9606,.T.);
#13600=ORIENTED_EDGE('',*,*,#9364,.T.);
#13601=ORIENTED_EDGE('',*,*,#9607,.F.);
#13602=ORIENTED_EDGE('',*,*,#9561,.T.);
#13603=ORIENTED_EDGE('',*,*,#9553,.T.);
#13604=ORIENTED_EDGE('',*,*,#9545,.T.);
#13605=ORIENTED_EDGE('',*,*,#9608,.T.);
#13606=ORIENTED_EDGE('',*,*,#9609,.T.);
#13607=ORIENTED_EDGE('',*,*,#9610,.F.);
#13608=ORIENTED_EDGE('',*,*,#9611,.T.);
#13609=ORIENTED_EDGE('',*,*,#9612,.T.);
#13610=ORIENTED_EDGE('',*,*,#9560,.T.);
#13611=ORIENTED_EDGE('',*,*,#9613,.T.);
#13612=ORIENTED_EDGE('',*,*,#9614,.T.);
#13613=ORIENTED_EDGE('',*,*,#9615,.T.);
#13614=ORIENTED_EDGE('',*,*,#9616,.F.);
#13615=ORIENTED_EDGE('',*,*,#9617,.T.);
#13616=ORIENTED_EDGE('',*,*,#9618,.F.);
#13617=ORIENTED_EDGE('',*,*,#9556,.T.);
#13618=ORIENTED_EDGE('',*,*,#9552,.T.);
#13619=ORIENTED_EDGE('',*,*,#9619,.T.);
#13620=ORIENTED_EDGE('',*,*,#9427,.T.);
#13621=ORIENTED_EDGE('',*,*,#9491,.T.);
#13622=ORIENTED_EDGE('',*,*,#9620,.T.);
#13623=ORIENTED_EDGE('',*,*,#9621,.T.);
#13624=ORIENTED_EDGE('',*,*,#9622,.T.);
#13625=ORIENTED_EDGE('',*,*,#9623,.T.);
#13626=ORIENTED_EDGE('',*,*,#9624,.F.);
#13627=ORIENTED_EDGE('',*,*,#9398,.F.);
#13628=ORIENTED_EDGE('',*,*,#9625,.T.);
#13629=ORIENTED_EDGE('',*,*,#9404,.F.);
#13630=ORIENTED_EDGE('',*,*,#9626,.T.);
#13631=ORIENTED_EDGE('',*,*,#9627,.T.);
#13632=ORIENTED_EDGE('',*,*,#9628,.F.);
#13633=ORIENTED_EDGE('',*,*,#9451,.T.);
#13634=ORIENTED_EDGE('',*,*,#9629,.F.);
#13635=ORIENTED_EDGE('',*,*,#9420,.T.);
#13636=ORIENTED_EDGE('',*,*,#9422,.T.);
#13637=ORIENTED_EDGE('',*,*,#9630,.F.);
#13638=ORIENTED_EDGE('',*,*,#9631,.F.);
#13639=ORIENTED_EDGE('',*,*,#9409,.T.);
#13640=ORIENTED_EDGE('',*,*,#9624,.T.);
#13641=ORIENTED_EDGE('',*,*,#9632,.T.);
#13642=ORIENTED_EDGE('',*,*,#9399,.T.);
#13643=ORIENTED_EDGE('',*,*,#9421,.F.);
#13644=ORIENTED_EDGE('',*,*,#9629,.T.);
#13645=ORIENTED_EDGE('',*,*,#9413,.F.);
#13646=ORIENTED_EDGE('',*,*,#9632,.F.);
#13647=ORIENTED_EDGE('',*,*,#9625,.F.);
#13648=ORIENTED_EDGE('',*,*,#9633,.F.);
#13649=ORIENTED_EDGE('',*,*,#9630,.T.);
#13650=ORIENTED_EDGE('',*,*,#9487,.T.);
#13651=ORIENTED_EDGE('',*,*,#9634,.T.);
#13652=ORIENTED_EDGE('',*,*,#9635,.F.);
#13653=ORIENTED_EDGE('',*,*,#9636,.F.);
#13654=ORIENTED_EDGE('',*,*,#9401,.F.);
#13655=ORIENTED_EDGE('',*,*,#9637,.F.);
#13656=ORIENTED_EDGE('',*,*,#9411,.F.);
#13657=ORIENTED_EDGE('',*,*,#9381,.T.);
#13658=ORIENTED_EDGE('',*,*,#9638,.T.);
#13659=ORIENTED_EDGE('',*,*,#9639,.T.);
#13660=ORIENTED_EDGE('',*,*,#9493,.T.);
#13661=ORIENTED_EDGE('',*,*,#9640,.T.);
#13662=ORIENTED_EDGE('',*,*,#9474,.T.);
#13663=ORIENTED_EDGE('',*,*,#9641,.T.);
#13664=ORIENTED_EDGE('',*,*,#9268,.T.);
#13665=ORIENTED_EDGE('',*,*,#9517,.T.);
#13666=ORIENTED_EDGE('',*,*,#9314,.F.);
#13667=ORIENTED_EDGE('',*,*,#9642,.T.);
#13668=ORIENTED_EDGE('',*,*,#9293,.F.);
#13669=ORIENTED_EDGE('',*,*,#9353,.T.);
#13670=ORIENTED_EDGE('',*,*,#9466,.F.);
#13671=ORIENTED_EDGE('',*,*,#9361,.F.);
#13672=ORIENTED_EDGE('',*,*,#9492,.T.);
#13673=ORIENTED_EDGE('',*,*,#9623,.F.);
#13674=ORIENTED_EDGE('',*,*,#9643,.T.);
#13675=ORIENTED_EDGE('',*,*,#9335,.F.);
#13676=ORIENTED_EDGE('',*,*,#9475,.T.);
#13677=ORIENTED_EDGE('',*,*,#9640,.F.);
#13678=ORIENTED_EDGE('',*,*,#9495,.T.);
#13679=ORIENTED_EDGE('',*,*,#9478,.T.);
#13680=ORIENTED_EDGE('',*,*,#9463,.T.);
#13681=ORIENTED_EDGE('',*,*,#9610,.T.);
#13682=ORIENTED_EDGE('',*,*,#9644,.T.);
#13683=ORIENTED_EDGE('',*,*,#9645,.F.);
#13684=ORIENTED_EDGE('',*,*,#9646,.F.);
#13685=ORIENTED_EDGE('',*,*,#9645,.T.);
#13686=ORIENTED_EDGE('',*,*,#9647,.F.);
#13687=ORIENTED_EDGE('',*,*,#9648,.F.);
#13688=ORIENTED_EDGE('',*,*,#9649,.F.);
#13689=ORIENTED_EDGE('',*,*,#9646,.T.);
#13690=ORIENTED_EDGE('',*,*,#9650,.F.);
#13691=ORIENTED_EDGE('',*,*,#9365,.F.);
#13692=ORIENTED_EDGE('',*,*,#9606,.F.);
#13693=ORIENTED_EDGE('',*,*,#9537,.F.);
#13694=ORIENTED_EDGE('',*,*,#9648,.T.);
#13695=ORIENTED_EDGE('',*,*,#9595,.F.);
#13696=ORIENTED_EDGE('',*,*,#9388,.F.);
#13697=ORIENTED_EDGE('',*,*,#9651,.T.);
#13698=ORIENTED_EDGE('',*,*,#9652,.T.);
#13699=ORIENTED_EDGE('',*,*,#9390,.T.);
#13700=ORIENTED_EDGE('',*,*,#9597,.T.);
#13701=ORIENTED_EDGE('',*,*,#9601,.T.);
#13702=ORIENTED_EDGE('',*,*,#9598,.T.);
#13703=ORIENTED_EDGE('',*,*,#9538,.T.);
#13704=ORIENTED_EDGE('',*,*,#9443,.T.);
#13705=ORIENTED_EDGE('',*,*,#9653,.F.);
#13706=ORIENTED_EDGE('',*,*,#9654,.F.);
#13707=ORIENTED_EDGE('',*,*,#9655,.F.);
#13708=ORIENTED_EDGE('',*,*,#9654,.T.);
#13709=ORIENTED_EDGE('',*,*,#9656,.F.);
#13710=ORIENTED_EDGE('',*,*,#9383,.F.);
#13711=ORIENTED_EDGE('',*,*,#9657,.F.);
#13712=ORIENTED_EDGE('',*,*,#9658,.T.);
#13713=ORIENTED_EDGE('',*,*,#9659,.T.);
#13714=ORIENTED_EDGE('',*,*,#9635,.T.);
#13715=ORIENTED_EDGE('',*,*,#9660,.T.);
#13716=ORIENTED_EDGE('',*,*,#9637,.T.);
#13717=ORIENTED_EDGE('',*,*,#9380,.T.);
#13718=ORIENTED_EDGE('',*,*,#9659,.F.);
#13719=ORIENTED_EDGE('',*,*,#9661,.F.);
#13720=ORIENTED_EDGE('',*,*,#9636,.T.);
#13721=ORIENTED_EDGE('',*,*,#9662,.F.);
#13722=ORIENTED_EDGE('',*,*,#9658,.F.);
#13723=ORIENTED_EDGE('',*,*,#9379,.F.);
#13724=ORIENTED_EDGE('',*,*,#9410,.F.);
#13725=ORIENTED_EDGE('',*,*,#9631,.T.);
#13726=ORIENTED_EDGE('',*,*,#9633,.T.);
#13727=ORIENTED_EDGE('',*,*,#9397,.F.);
#13728=ORIENTED_EDGE('',*,*,#9412,.F.);
#13729=ORIENTED_EDGE('',*,*,#9660,.F.);
#13730=ORIENTED_EDGE('',*,*,#9634,.F.);
#13731=ORIENTED_EDGE('',*,*,#9663,.T.);
#13732=ORIENTED_EDGE('',*,*,#9664,.T.);
#13733=ORIENTED_EDGE('',*,*,#9665,.F.);
#13734=ORIENTED_EDGE('',*,*,#9402,.T.);
#13735=ORIENTED_EDGE('',*,*,#9661,.T.);
#13736=ORIENTED_EDGE('',*,*,#9662,.T.);
#13737=ORIENTED_EDGE('',*,*,#9407,.T.);
#13738=ORIENTED_EDGE('',*,*,#9416,.T.);
#13739=ORIENTED_EDGE('',*,*,#9418,.T.);
#13740=ORIENTED_EDGE('',*,*,#9622,.F.);
#13741=ORIENTED_EDGE('',*,*,#9666,.T.);
#13742=ORIENTED_EDGE('',*,*,#9336,.F.);
#13743=ORIENTED_EDGE('',*,*,#9643,.F.);
#13744=ORIENTED_EDGE('',*,*,#9374,.F.);
#13745=ORIENTED_EDGE('',*,*,#9324,.F.);
#13746=ORIENTED_EDGE('',*,*,#9327,.F.);
#13747=ORIENTED_EDGE('',*,*,#9326,.F.);
#13748=ORIENTED_EDGE('',*,*,#9377,.T.);
#13749=ORIENTED_EDGE('',*,*,#9419,.F.);
#13750=ORIENTED_EDGE('',*,*,#9414,.F.);
#13751=ORIENTED_EDGE('',*,*,#9667,.F.);
#13752=ORIENTED_EDGE('',*,*,#9308,.F.);
#13753=ORIENTED_EDGE('',*,*,#9307,.F.);
#13754=ORIENTED_EDGE('',*,*,#9668,.F.);
#13755=ORIENTED_EDGE('',*,*,#9294,.F.);
#13756=ORIENTED_EDGE('',*,*,#9642,.F.);
#13757=ORIENTED_EDGE('',*,*,#9313,.F.);
#13758=ORIENTED_EDGE('',*,*,#9312,.F.);
#13759=ORIENTED_EDGE('',*,*,#9669,.F.);
#13760=ORIENTED_EDGE('',*,*,#9664,.F.);
#13761=ORIENTED_EDGE('',*,*,#9670,.T.);
#13762=ORIENTED_EDGE('',*,*,#9310,.T.);
#13763=ORIENTED_EDGE('',*,*,#9671,.F.);
#13764=ORIENTED_EDGE('',*,*,#9627,.F.);
#13765=ORIENTED_EDGE('',*,*,#9665,.T.);
#13766=ORIENTED_EDGE('',*,*,#9669,.T.);
#13767=ORIENTED_EDGE('',*,*,#9311,.T.);
#13768=ORIENTED_EDGE('',*,*,#9670,.F.);
#13769=ORIENTED_EDGE('',*,*,#9626,.F.);
#13770=ORIENTED_EDGE('',*,*,#9403,.T.);
#13771=ORIENTED_EDGE('',*,*,#9542,.T.);
#13772=ORIENTED_EDGE('',*,*,#9672,.F.);
#13773=ORIENTED_EDGE('',*,*,#9673,.F.);
#13774=ORIENTED_EDGE('',*,*,#9608,.F.);
#13775=ORIENTED_EDGE('',*,*,#9644,.F.);
#13776=ORIENTED_EDGE('',*,*,#9609,.F.);
#13777=ORIENTED_EDGE('',*,*,#9674,.T.);
#13778=ORIENTED_EDGE('',*,*,#9675,.F.);
#13779=ORIENTED_EDGE('',*,*,#9676,.F.);
#13780=ORIENTED_EDGE('',*,*,#9677,.F.);
#13781=ORIENTED_EDGE('',*,*,#9674,.F.);
#13782=ORIENTED_EDGE('',*,*,#9673,.T.);
#13783=ORIENTED_EDGE('',*,*,#9604,.T.);
#13784=ORIENTED_EDGE('',*,*,#9678,.T.);
#13785=ORIENTED_EDGE('',*,*,#9386,.F.);
#13786=ORIENTED_EDGE('',*,*,#9445,.T.);
#13787=ORIENTED_EDGE('',*,*,#9586,.T.);
#13788=ORIENTED_EDGE('',*,*,#9578,.T.);
#13789=ORIENTED_EDGE('',*,*,#9576,.T.);
#13790=ORIENTED_EDGE('',*,*,#9589,.T.);
#13791=ORIENTED_EDGE('',*,*,#9679,.F.);
#13792=ORIENTED_EDGE('',*,*,#9680,.F.);
#13793=ORIENTED_EDGE('',*,*,#9613,.F.);
#13794=ORIENTED_EDGE('',*,*,#9559,.T.);
#13795=ORIENTED_EDGE('',*,*,#9607,.T.);
#13796=ORIENTED_EDGE('',*,*,#9363,.T.);
#13797=ORIENTED_EDGE('',*,*,#9536,.T.);
#13798=ORIENTED_EDGE('',*,*,#9599,.T.);
#13799=ORIENTED_EDGE('',*,*,#9681,.T.);
#13800=ORIENTED_EDGE('',*,*,#9531,.T.);
#13801=ORIENTED_EDGE('',*,*,#9682,.T.);
#13802=ORIENTED_EDGE('',*,*,#9616,.T.);
#13803=ORIENTED_EDGE('',*,*,#9683,.T.);
#13804=ORIENTED_EDGE('',*,*,#9351,.T.);
#13805=ORIENTED_EDGE('',*,*,#9684,.T.);
#13806=ORIENTED_EDGE('',*,*,#9685,.T.);
#13807=ORIENTED_EDGE('',*,*,#9686,.T.);
#13808=ORIENTED_EDGE('',*,*,#9342,.T.);
#13809=ORIENTED_EDGE('',*,*,#9687,.T.);
#13810=ORIENTED_EDGE('',*,*,#9688,.T.);
#13811=ORIENTED_EDGE('',*,*,#9689,.T.);
#13812=ORIENTED_EDGE('',*,*,#9690,.T.);
#13813=ORIENTED_EDGE('',*,*,#9484,.F.);
#13814=ORIENTED_EDGE('',*,*,#9470,.F.);
#13815=ORIENTED_EDGE('',*,*,#9573,.T.);
#13816=ORIENTED_EDGE('',*,*,#9435,.T.);
#13817=ORIENTED_EDGE('',*,*,#9568,.T.);
#13818=ORIENTED_EDGE('',*,*,#9577,.T.);
#13819=ORIENTED_EDGE('',*,*,#9583,.T.);
#13820=ORIENTED_EDGE('',*,*,#9439,.T.);
#13821=ORIENTED_EDGE('',*,*,#9571,.T.);
#13822=ORIENTED_EDGE('',*,*,#9580,.T.);
#13823=ORIENTED_EDGE('',*,*,#9685,.F.);
#13824=ORIENTED_EDGE('',*,*,#9691,.T.);
#13825=ORIENTED_EDGE('',*,*,#9692,.T.);
#13826=ORIENTED_EDGE('',*,*,#9587,.T.);
#13827=ORIENTED_EDGE('',*,*,#9569,.T.);
#13828=ORIENTED_EDGE('',*,*,#9564,.T.);
#13829=ORIENTED_EDGE('',*,*,#9693,.T.);
#13830=ORIENTED_EDGE('',*,*,#9694,.T.);
#13831=ORIENTED_EDGE('',*,*,#9652,.F.);
#13832=ORIENTED_EDGE('',*,*,#9602,.T.);
#13833=ORIENTED_EDGE('',*,*,#9600,.T.);
#13834=ORIENTED_EDGE('',*,*,#9590,.T.);
#13835=ORIENTED_EDGE('',*,*,#9695,.T.);
#13836=ORIENTED_EDGE('',*,*,#9653,.T.);
#13837=ORIENTED_EDGE('',*,*,#9582,.T.);
#13838=ORIENTED_EDGE('',*,*,#9585,.T.);
#13839=ORIENTED_EDGE('',*,*,#9309,.F.);
#13840=ORIENTED_EDGE('',*,*,#9667,.T.);
#13841=ORIENTED_EDGE('',*,*,#9663,.F.);
#13842=ORIENTED_EDGE('',*,*,#9417,.T.);
#13843=ORIENTED_EDGE('',*,*,#9405,.F.);
#13844=ORIENTED_EDGE('',*,*,#9628,.T.);
#13845=ORIENTED_EDGE('',*,*,#9671,.T.);
#13846=ORIENTED_EDGE('',*,*,#9649,.T.);
#13847=ORIENTED_EDGE('',*,*,#9539,.T.);
#13848=ORIENTED_EDGE('',*,*,#9535,.T.);
#13849=ORIENTED_EDGE('',*,*,#9650,.T.);
#13850=ORIENTED_EDGE('',*,*,#9696,.T.);
#13851=ORIENTED_EDGE('',*,*,#9697,.T.);
#13852=ORIENTED_EDGE('',*,*,#9698,.F.);
#13853=ORIENTED_EDGE('',*,*,#9679,.T.);
#13854=ORIENTED_EDGE('',*,*,#9384,.T.);
#13855=ORIENTED_EDGE('',*,*,#9656,.T.);
#13856=ORIENTED_EDGE('',*,*,#9695,.F.);
#13857=ORIENTED_EDGE('',*,*,#9446,.T.);
#13858=ORIENTED_EDGE('',*,*,#9618,.T.);
#13859=ORIENTED_EDGE('',*,*,#9699,.T.);
#13860=ORIENTED_EDGE('',*,*,#9513,.F.);
#13861=ORIENTED_EDGE('',*,*,#9504,.T.);
#13862=ORIENTED_EDGE('',*,*,#9467,.T.);
#13863=ORIENTED_EDGE('',*,*,#9700,.T.);
#13864=ORIENTED_EDGE('',*,*,#9701,.T.);
#13865=ORIENTED_EDGE('',*,*,#9546,.T.);
#13866=ORIENTED_EDGE('',*,*,#9605,.T.);
#13867=ORIENTED_EDGE('',*,*,#9554,.T.);
#13868=ORIENTED_EDGE('',*,*,#9702,.T.);
#13869=ORIENTED_EDGE('',*,*,#9703,.T.);
#13870=ORIENTED_EDGE('',*,*,#9704,.T.);
#13871=ORIENTED_EDGE('',*,*,#9614,.F.);
#13872=ORIENTED_EDGE('',*,*,#9705,.T.);
#13873=ORIENTED_EDGE('',*,*,#9611,.F.);
#13874=ORIENTED_EDGE('',*,*,#9680,.T.);
#13875=ORIENTED_EDGE('',*,*,#9698,.T.);
#13876=ORIENTED_EDGE('',*,*,#9332,.F.);
#13877=ORIENTED_EDGE('',*,*,#9706,.T.);
#13878=ORIENTED_EDGE('',*,*,#9707,.F.);
#13879=ORIENTED_EDGE('',*,*,#9305,.F.);
#13880=ORIENTED_EDGE('',*,*,#9708,.T.);
#13881=ORIENTED_EDGE('',*,*,#9638,.F.);
#13882=ORIENTED_EDGE('',*,*,#9473,.F.);
#13883=ORIENTED_EDGE('',*,*,#9333,.F.);
#13884=ORIENTED_EDGE('',*,*,#9396,.F.);
#13885=ORIENTED_EDGE('',*,*,#9709,.T.);
#13886=ORIENTED_EDGE('',*,*,#9338,.F.);
#13887=ORIENTED_EDGE('',*,*,#9337,.F.);
#13888=ORIENTED_EDGE('',*,*,#9666,.F.);
#13889=ORIENTED_EDGE('',*,*,#9621,.F.);
#13890=ORIENTED_EDGE('',*,*,#9710,.T.);
#13891=ORIENTED_EDGE('',*,*,#9303,.F.);
#13892=ORIENTED_EDGE('',*,*,#9352,.F.);
#13893=ORIENTED_EDGE('',*,*,#9711,.T.);
#13894=ORIENTED_EDGE('',*,*,#9712,.F.);
#13895=ORIENTED_EDGE('',*,*,#9703,.F.);
#13896=ORIENTED_EDGE('',*,*,#9713,.F.);
#13897=ORIENTED_EDGE('',*,*,#9320,.F.);
#13898=ORIENTED_EDGE('',*,*,#9712,.T.);
#13899=ORIENTED_EDGE('',*,*,#9702,.F.);
#13900=ORIENTED_EDGE('',*,*,#9697,.F.);
#13901=ORIENTED_EDGE('',*,*,#9714,.F.);
#13902=ORIENTED_EDGE('',*,*,#9321,.F.);
#13903=ORIENTED_EDGE('',*,*,#9713,.T.);
#13904=ORIENTED_EDGE('',*,*,#9692,.F.);
#13905=ORIENTED_EDGE('',*,*,#9715,.T.);
#13906=ORIENTED_EDGE('',*,*,#9696,.F.);
#13907=ORIENTED_EDGE('',*,*,#9588,.F.);
#13908=ORIENTED_EDGE('',*,*,#9350,.T.);
#13909=ORIENTED_EDGE('',*,*,#9323,.F.);
#13910=ORIENTED_EDGE('',*,*,#9716,.F.);
#13911=ORIENTED_EDGE('',*,*,#9691,.F.);
#13912=ORIENTED_EDGE('',*,*,#9684,.F.);
#13913=ORIENTED_EDGE('',*,*,#9346,.F.);
#13914=ORIENTED_EDGE('',*,*,#9328,.F.);
#13915=ORIENTED_EDGE('',*,*,#9349,.T.);
#13916=ORIENTED_EDGE('',*,*,#9356,.F.);
#13917=ORIENTED_EDGE('',*,*,#9355,.F.);
#13918=ORIENTED_EDGE('',*,*,#9714,.T.);
#13919=ORIENTED_EDGE('',*,*,#9715,.F.);
#13920=ORIENTED_EDGE('',*,*,#9716,.T.);
#13921=ORIENTED_EDGE('',*,*,#9322,.F.);
#13922=ORIENTED_EDGE('',*,*,#9705,.F.);
#13923=ORIENTED_EDGE('',*,*,#9619,.F.);
#13924=ORIENTED_EDGE('',*,*,#9558,.F.);
#13925=ORIENTED_EDGE('',*,*,#9612,.F.);
#13926=ORIENTED_EDGE('',*,*,#9387,.F.);
#13927=ORIENTED_EDGE('',*,*,#9678,.F.);
#13928=ORIENTED_EDGE('',*,*,#9603,.T.);
#13929=ORIENTED_EDGE('',*,*,#9651,.F.);
#13930=ORIENTED_EDGE('',*,*,#9711,.F.);
#13931=ORIENTED_EDGE('',*,*,#9683,.F.);
#13932=ORIENTED_EDGE('',*,*,#9615,.F.);
#13933=ORIENTED_EDGE('',*,*,#9704,.F.);
#13934=ORIENTED_EDGE('',*,*,#9717,.F.);
#13935=ORIENTED_EDGE('',*,*,#9718,.T.);
#13936=ORIENTED_EDGE('',*,*,#9693,.F.);
#13937=ORIENTED_EDGE('',*,*,#9563,.F.);
#13938=ORIENTED_EDGE('',*,*,#9682,.F.);
#13939=ORIENTED_EDGE('',*,*,#9530,.T.);
#13940=ORIENTED_EDGE('',*,*,#9699,.F.);
#13941=ORIENTED_EDGE('',*,*,#9617,.F.);
#13942=ORIENTED_EDGE('',*,*,#9719,.F.);
#13943=ORIENTED_EDGE('',*,*,#9700,.F.);
#13944=ORIENTED_EDGE('',*,*,#9343,.T.);
#13945=ORIENTED_EDGE('',*,*,#9686,.F.);
#13946=ORIENTED_EDGE('',*,*,#9694,.F.);
#13947=ORIENTED_EDGE('',*,*,#9718,.F.);
#13948=ORIENTED_EDGE('',*,*,#9512,.F.);
#13949=ORIENTED_EDGE('',*,*,#9529,.T.);
#13950=ORIENTED_EDGE('',*,*,#9681,.F.);
#13951=ORIENTED_EDGE('',*,*,#9720,.F.);
#13952=ORIENTED_EDGE('',*,*,#9720,.T.);
#13953=ORIENTED_EDGE('',*,*,#9690,.F.);
#13954=ORIENTED_EDGE('',*,*,#9721,.F.);
#13955=ORIENTED_EDGE('',*,*,#9510,.F.);
#13956=ORIENTED_EDGE('',*,*,#9721,.T.);
#13957=ORIENTED_EDGE('',*,*,#9689,.F.);
#13958=ORIENTED_EDGE('',*,*,#9722,.F.);
#13959=ORIENTED_EDGE('',*,*,#9508,.F.);
#13960=ORIENTED_EDGE('',*,*,#9722,.T.);
#13961=ORIENTED_EDGE('',*,*,#9688,.F.);
#13962=ORIENTED_EDGE('',*,*,#9723,.F.);
#13963=ORIENTED_EDGE('',*,*,#9500,.F.);
#13964=ORIENTED_EDGE('',*,*,#9687,.F.);
#13965=ORIENTED_EDGE('',*,*,#9341,.T.);
#13966=ORIENTED_EDGE('',*,*,#9497,.F.);
#13967=ORIENTED_EDGE('',*,*,#9723,.T.);
#13968=ORIENTED_EDGE('',*,*,#9708,.F.);
#13969=ORIENTED_EDGE('',*,*,#9304,.F.);
#13970=ORIENTED_EDGE('',*,*,#9710,.F.);
#13971=ORIENTED_EDGE('',*,*,#9620,.F.);
#13972=ORIENTED_EDGE('',*,*,#9490,.F.);
#13973=ORIENTED_EDGE('',*,*,#9359,.F.);
#13974=ORIENTED_EDGE('',*,*,#9358,.F.);
#13975=ORIENTED_EDGE('',*,*,#9357,.F.);
#13976=ORIENTED_EDGE('',*,*,#9494,.F.);
#13977=ORIENTED_EDGE('',*,*,#9639,.F.);
#13978=ORIENTED_EDGE('',*,*,#9395,.F.);
#13979=ORIENTED_EDGE('',*,*,#9296,.F.);
#13980=ORIENTED_EDGE('',*,*,#9724,.F.);
#13981=ORIENTED_EDGE('',*,*,#9706,.F.);
#13982=ORIENTED_EDGE('',*,*,#9339,.F.);
#13983=ORIENTED_EDGE('',*,*,#9709,.F.);
#13984=ORIENTED_EDGE('',*,*,#9330,.F.);
#13985=ORIENTED_EDGE('',*,*,#9428,.F.);
#13986=ORIENTED_EDGE('',*,*,#9707,.T.);
#13987=ORIENTED_EDGE('',*,*,#9724,.T.);
#13988=ORIENTED_EDGE('',*,*,#9295,.F.);
#13989=ORIENTED_EDGE('',*,*,#9668,.T.);
#13990=ORIENTED_EDGE('',*,*,#9306,.F.);
#13991=ORIENTED_EDGE('',*,*,#9317,.F.);
#13992=ORIENTED_EDGE('',*,*,#9526,.T.);
#13993=ORIENTED_EDGE('',*,*,#9272,.F.);
#13994=ORIENTED_EDGE('',*,*,#9285,.F.);
#13995=ORIENTED_EDGE('',*,*,#9725,.T.);
#13996=ORIENTED_EDGE('',*,*,#9726,.T.);
#13997=ORIENTED_EDGE('',*,*,#9394,.F.);
#13998=ORIENTED_EDGE('',*,*,#9725,.F.);
#13999=ORIENTED_EDGE('',*,*,#9284,.F.);
#14000=ORIENTED_EDGE('',*,*,#9519,.T.);
#14001=ORIENTED_EDGE('',*,*,#9263,.T.);
#14002=ORIENTED_EDGE('',*,*,#9641,.F.);
#14003=ORIENTED_EDGE('',*,*,#9292,.F.);
#14004=ORIENTED_EDGE('',*,*,#9726,.F.);
#14005=ORIENTED_EDGE('',*,*,#9283,.F.);
#14006=ORIENTED_EDGE('',*,*,#9276,.F.);
#14007=ORIENTED_EDGE('',*,*,#9727,.F.);
#14008=ORIENTED_EDGE('',*,*,#9280,.F.);
#14009=ORIENTED_EDGE('',*,*,#9728,.F.);
#14010=ORIENTED_EDGE('',*,*,#9729,.F.);
#14011=ORIENTED_EDGE('',*,*,#9455,.T.);
#14012=ORIENTED_EDGE('',*,*,#9265,.T.);
#14013=ORIENTED_EDGE('',*,*,#9518,.T.);
#14014=ORIENTED_EDGE('',*,*,#9459,.T.);
#14015=ORIENTED_EDGE('',*,*,#9525,.T.);
#14016=ORIENTED_EDGE('',*,*,#9528,.T.);
#14017=ORIENTED_EDGE('',*,*,#9457,.T.);
#14018=ORIENTED_EDGE('',*,*,#9462,.T.);
#14019=ORIENTED_EDGE('',*,*,#9523,.T.);
#14020=ORIENTED_EDGE('',*,*,#9730,.F.);
#14021=ORIENTED_EDGE('',*,*,#9729,.T.);
#14022=ORIENTED_EDGE('',*,*,#9515,.F.);
#14023=ORIENTED_EDGE('',*,*,#9288,.T.);
#14024=ORIENTED_EDGE('',*,*,#9281,.F.);
#14025=ORIENTED_EDGE('',*,*,#9727,.T.);
#14026=ORIENTED_EDGE('',*,*,#9730,.T.);
#14027=ORIENTED_EDGE('',*,*,#9728,.T.);
#14028=ORIENTED_EDGE('',*,*,#9279,.F.);
#14029=ORIENTED_EDGE('',*,*,#9287,.T.);
#14030=ORIENTED_EDGE('',*,*,#9655,.T.);
#14031=ORIENTED_EDGE('',*,*,#9657,.T.);
#14032=ORIENTED_EDGE('',*,*,#9382,.T.);
#14033=ORIENTED_EDGE('',*,*,#9392,.T.);
#14034=ORIENTED_EDGE('',*,*,#9592,.T.);
#14035=ORIENTED_EDGE('',*,*,#9596,.T.);
#14036=ORIENTED_EDGE('',*,*,#9647,.T.);
#14037=ORIENTED_EDGE('',*,*,#9675,.T.);
#14038=ORIENTED_EDGE('',*,*,#9677,.T.);
#14039=ORIENTED_EDGE('',*,*,#9731,.F.);
#14040=ORIENTED_EDGE('',*,*,#9732,.T.);
#14041=ORIENTED_EDGE('',*,*,#9733,.F.);
#14042=ORIENTED_EDGE('',*,*,#9562,.T.);
#14043=ORIENTED_EDGE('',*,*,#9437,.T.);
#14044=ORIENTED_EDGE('',*,*,#9441,.T.);
#14045=ORIENTED_EDGE('',*,*,#9734,.T.);
#14046=ORIENTED_EDGE('',*,*,#9732,.F.);
#14047=ORIENTED_EDGE('',*,*,#9701,.F.);
#14048=ORIENTED_EDGE('',*,*,#9719,.T.);
#14049=ORIENTED_EDGE('',*,*,#9717,.T.);
#14050=ORIENTED_EDGE('',*,*,#9733,.T.);
#14051=ORIENTED_EDGE('',*,*,#9734,.F.);
#14052=ORIENTED_EDGE('',*,*,#9731,.T.);
#14053=ORIENTED_EDGE('',*,*,#9676,.T.);
#14054=ORIENTED_EDGE('',*,*,#9672,.T.);
#14055=ORIENTED_EDGE('',*,*,#9547,.T.);
#14056=ORIENTED_EDGE('',*,*,#9425,.F.);
#14057=ORIENTED_EDGE('',*,*,#9735,.F.);
#14058=ORIENTED_EDGE('',*,*,#9736,.T.);
#14059=ORIENTED_EDGE('',*,*,#9737,.T.);
#14060=ORIENTED_EDGE('',*,*,#9736,.F.);
#14061=ORIENTED_EDGE('',*,*,#9738,.F.);
#14062=ORIENTED_EDGE('',*,*,#9739,.T.);
#14063=ORIENTED_EDGE('',*,*,#9740,.F.);
#14064=ORIENTED_EDGE('',*,*,#9739,.F.);
#14065=ORIENTED_EDGE('',*,*,#9737,.F.);
#14066=ORIENTED_EDGE('',*,*,#9738,.T.);
#14067=ORIENTED_EDGE('',*,*,#9735,.T.);
#14068=ORIENTED_EDGE('',*,*,#9740,.T.);
#14069=ORIENTED_EDGE('',*,*,#9741,.F.);
#14070=ORIENTED_EDGE('',*,*,#9742,.F.);
#14071=ORIENTED_EDGE('',*,*,#9743,.F.);
#14072=ORIENTED_EDGE('',*,*,#9744,.F.);
#14073=ORIENTED_EDGE('',*,*,#9745,.F.);
#14074=ORIENTED_EDGE('',*,*,#9746,.F.);
#14075=ORIENTED_EDGE('',*,*,#9747,.F.);
#14076=ORIENTED_EDGE('',*,*,#9748,.F.);
#14077=ORIENTED_EDGE('',*,*,#9749,.F.);
#14078=ORIENTED_EDGE('',*,*,#9750,.F.);
#14079=ORIENTED_EDGE('',*,*,#9751,.F.);
#14080=ORIENTED_EDGE('',*,*,#9752,.F.);
#14081=ORIENTED_EDGE('',*,*,#9753,.F.);
#14082=ORIENTED_EDGE('',*,*,#9754,.F.);
#14083=ORIENTED_EDGE('',*,*,#9755,.F.);
#14084=ORIENTED_EDGE('',*,*,#9756,.F.);
#14085=ORIENTED_EDGE('',*,*,#9757,.F.);
#14086=ORIENTED_EDGE('',*,*,#9743,.T.);
#14087=ORIENTED_EDGE('',*,*,#9758,.F.);
#14088=ORIENTED_EDGE('',*,*,#9745,.T.);
#14089=ORIENTED_EDGE('',*,*,#9759,.T.);
#14090=ORIENTED_EDGE('',*,*,#9751,.T.);
#14091=ORIENTED_EDGE('',*,*,#9760,.T.);
#14092=ORIENTED_EDGE('',*,*,#9753,.T.);
#14093=ORIENTED_EDGE('',*,*,#9761,.T.);
#14094=ORIENTED_EDGE('',*,*,#9741,.T.);
#14095=ORIENTED_EDGE('',*,*,#9762,.F.);
#14096=ORIENTED_EDGE('',*,*,#9755,.T.);
#14097=ORIENTED_EDGE('',*,*,#9763,.F.);
#14098=ORIENTED_EDGE('',*,*,#9749,.T.);
#14099=ORIENTED_EDGE('',*,*,#9764,.T.);
#14100=ORIENTED_EDGE('',*,*,#9747,.T.);
#14101=ORIENTED_EDGE('',*,*,#9758,.T.);
#14102=ORIENTED_EDGE('',*,*,#9742,.T.);
#14103=ORIENTED_EDGE('',*,*,#9761,.F.);
#14104=ORIENTED_EDGE('',*,*,#9754,.T.);
#14105=ORIENTED_EDGE('',*,*,#9760,.F.);
#14106=ORIENTED_EDGE('',*,*,#9750,.T.);
#14107=ORIENTED_EDGE('',*,*,#9763,.T.);
#14108=ORIENTED_EDGE('',*,*,#9746,.T.);
#14109=ORIENTED_EDGE('',*,*,#9762,.T.);
#14110=ORIENTED_EDGE('',*,*,#9744,.T.);
#14111=ORIENTED_EDGE('',*,*,#9757,.T.);
#14112=ORIENTED_EDGE('',*,*,#9748,.T.);
#14113=ORIENTED_EDGE('',*,*,#9764,.F.);
#14114=ORIENTED_EDGE('',*,*,#9752,.T.);
#14115=ORIENTED_EDGE('',*,*,#9759,.F.);
#14116=ORIENTED_EDGE('',*,*,#9756,.T.);
#14117=ORIENTED_EDGE('',*,*,#9765,.T.);
#14118=ORIENTED_EDGE('',*,*,#9766,.F.);
#14119=ORIENTED_EDGE('',*,*,#9767,.F.);
#14120=ORIENTED_EDGE('',*,*,#9768,.F.);
#14121=ORIENTED_EDGE('',*,*,#9769,.F.);
#14122=ORIENTED_EDGE('',*,*,#9770,.F.);
#14123=ORIENTED_EDGE('',*,*,#9771,.F.);
#14124=ORIENTED_EDGE('',*,*,#9765,.F.);
#14125=ORIENTED_EDGE('',*,*,#9772,.F.);
#14126=ORIENTED_EDGE('',*,*,#9773,.T.);
#14127=ORIENTED_EDGE('',*,*,#9774,.F.);
#14128=ORIENTED_EDGE('',*,*,#9775,.T.);
#14129=ORIENTED_EDGE('',*,*,#9776,.T.);
#14130=ORIENTED_EDGE('',*,*,#9777,.T.);
#14131=ORIENTED_EDGE('',*,*,#9775,.F.);
#14132=ORIENTED_EDGE('',*,*,#9777,.F.);
#14133=ORIENTED_EDGE('',*,*,#9778,.T.);
#14134=ORIENTED_EDGE('',*,*,#9779,.F.);
#14135=ORIENTED_EDGE('',*,*,#9778,.F.);
#14136=ORIENTED_EDGE('',*,*,#9776,.F.);
#14137=ORIENTED_EDGE('',*,*,#9780,.F.);
#14138=ORIENTED_EDGE('',*,*,#9781,.T.);
#14139=ORIENTED_EDGE('',*,*,#9782,.T.);
#14140=ORIENTED_EDGE('',*,*,#9783,.T.);
#14141=ORIENTED_EDGE('',*,*,#9781,.F.);
#14142=ORIENTED_EDGE('',*,*,#9783,.F.);
#14143=ORIENTED_EDGE('',*,*,#9784,.T.);
#14144=ORIENTED_EDGE('',*,*,#9785,.F.);
#14145=ORIENTED_EDGE('',*,*,#9786,.F.);
#14146=ORIENTED_EDGE('',*,*,#9784,.F.);
#14147=ORIENTED_EDGE('',*,*,#9782,.F.);
#14148=ORIENTED_EDGE('',*,*,#9787,.F.);
#14149=ORIENTED_EDGE('',*,*,#9788,.T.);
#14150=ORIENTED_EDGE('',*,*,#9789,.T.);
#14151=ORIENTED_EDGE('',*,*,#9788,.F.);
#14152=ORIENTED_EDGE('',*,*,#9785,.T.);
#14153=ORIENTED_EDGE('',*,*,#9786,.T.);
#14154=ORIENTED_EDGE('',*,*,#9790,.T.);
#14155=ORIENTED_EDGE('',*,*,#9791,.F.);
#14156=ORIENTED_EDGE('',*,*,#9790,.F.);
#14157=ORIENTED_EDGE('',*,*,#9789,.F.);
#14158=ORIENTED_EDGE('',*,*,#9792,.T.);
#14159=ORIENTED_EDGE('',*,*,#9780,.T.);
#14160=ORIENTED_EDGE('',*,*,#9792,.F.);
#14161=ORIENTED_EDGE('',*,*,#9791,.T.);
#14162=ORIENTED_EDGE('',*,*,#9793,.F.);
#14163=ORIENTED_EDGE('',*,*,#9794,.T.);
#14164=ORIENTED_EDGE('',*,*,#9795,.F.);
#14165=ORIENTED_EDGE('',*,*,#9796,.T.);
#14166=ORIENTED_EDGE('',*,*,#9797,.F.);
#14167=ORIENTED_EDGE('',*,*,#9798,.T.);
#14168=ORIENTED_EDGE('',*,*,#9799,.F.);
#14169=ORIENTED_EDGE('',*,*,#9769,.T.);
#14170=ORIENTED_EDGE('',*,*,#9800,.F.);
#14171=ORIENTED_EDGE('',*,*,#9801,.F.);
#14172=ORIENTED_EDGE('',*,*,#9802,.T.);
#14173=ORIENTED_EDGE('',*,*,#9803,.F.);
#14174=ORIENTED_EDGE('',*,*,#9804,.T.);
#14175=ORIENTED_EDGE('',*,*,#9805,.F.);
#14176=ORIENTED_EDGE('',*,*,#9768,.T.);
#14177=ORIENTED_EDGE('',*,*,#9806,.F.);
#14178=ORIENTED_EDGE('',*,*,#9807,.F.);
#14179=ORIENTED_EDGE('',*,*,#9767,.T.);
#14180=ORIENTED_EDGE('',*,*,#9808,.F.);
#14181=ORIENTED_EDGE('',*,*,#9779,.T.);
#14182=ORIENTED_EDGE('',*,*,#9787,.T.);
#14183=ORIENTED_EDGE('',*,*,#9772,.T.);
#14184=ORIENTED_EDGE('',*,*,#9809,.F.);
#14185=ORIENTED_EDGE('',*,*,#9810,.F.);
#14186=ORIENTED_EDGE('',*,*,#9800,.T.);
#14187=ORIENTED_EDGE('',*,*,#9805,.T.);
#14188=ORIENTED_EDGE('',*,*,#9811,.T.);
#14189=ORIENTED_EDGE('',*,*,#9812,.T.);
#14190=ORIENTED_EDGE('',*,*,#9803,.T.);
#14191=ORIENTED_EDGE('',*,*,#9813,.F.);
#14192=ORIENTED_EDGE('',*,*,#9811,.F.);
#14193=ORIENTED_EDGE('',*,*,#9806,.T.);
#14194=ORIENTED_EDGE('',*,*,#9807,.T.);
#14195=ORIENTED_EDGE('',*,*,#9814,.T.);
#14196=ORIENTED_EDGE('',*,*,#9815,.T.);
#14197=ORIENTED_EDGE('',*,*,#9797,.T.);
#14198=ORIENTED_EDGE('',*,*,#9816,.F.);
#14199=ORIENTED_EDGE('',*,*,#9814,.F.);
#14200=ORIENTED_EDGE('',*,*,#9808,.T.);
#14201=ORIENTED_EDGE('',*,*,#9817,.T.);
#14202=ORIENTED_EDGE('',*,*,#9818,.T.);
#14203=ORIENTED_EDGE('',*,*,#9819,.T.);
#14204=ORIENTED_EDGE('',*,*,#9793,.T.);
#14205=ORIENTED_EDGE('',*,*,#9820,.F.);
#14206=ORIENTED_EDGE('',*,*,#9818,.F.);
#14207=ORIENTED_EDGE('',*,*,#9821,.T.);
#14208=ORIENTED_EDGE('',*,*,#9822,.T.);
#14209=ORIENTED_EDGE('',*,*,#9823,.T.);
#14210=ORIENTED_EDGE('',*,*,#9824,.T.);
#14211=ORIENTED_EDGE('',*,*,#9801,.T.);
#14212=ORIENTED_EDGE('',*,*,#9825,.F.);
#14213=ORIENTED_EDGE('',*,*,#9826,.F.);
#14214=ORIENTED_EDGE('',*,*,#9827,.T.);
#14215=ORIENTED_EDGE('',*,*,#9799,.T.);
#14216=ORIENTED_EDGE('',*,*,#9810,.T.);
#14217=ORIENTED_EDGE('',*,*,#9828,.T.);
#14218=ORIENTED_EDGE('',*,*,#9795,.T.);
#14219=ORIENTED_EDGE('',*,*,#9829,.F.);
#14220=ORIENTED_EDGE('',*,*,#9823,.F.);
#14221=ORIENTED_EDGE('',*,*,#9830,.T.);
#14222=ORIENTED_EDGE('',*,*,#9831,.T.);
#14223=ORIENTED_EDGE('',*,*,#9826,.T.);
#14224=ORIENTED_EDGE('',*,*,#9832,.T.);
#14225=ORIENTED_EDGE('',*,*,#9822,.F.);
#14226=ORIENTED_EDGE('',*,*,#9771,.T.);
#14227=ORIENTED_EDGE('',*,*,#9830,.F.);
#14228=ORIENTED_EDGE('',*,*,#9817,.F.);
#14229=ORIENTED_EDGE('',*,*,#9766,.T.);
#14230=ORIENTED_EDGE('',*,*,#9821,.F.);
#14231=ORIENTED_EDGE('',*,*,#9774,.T.);
#14232=ORIENTED_EDGE('',*,*,#9812,.F.);
#14233=ORIENTED_EDGE('',*,*,#9813,.T.);
#14234=ORIENTED_EDGE('',*,*,#9804,.F.);
#14235=ORIENTED_EDGE('',*,*,#9815,.F.);
#14236=ORIENTED_EDGE('',*,*,#9816,.T.);
#14237=ORIENTED_EDGE('',*,*,#9798,.F.);
#14238=ORIENTED_EDGE('',*,*,#9819,.F.);
#14239=ORIENTED_EDGE('',*,*,#9820,.T.);
#14240=ORIENTED_EDGE('',*,*,#9794,.F.);
#14241=ORIENTED_EDGE('',*,*,#9824,.F.);
#14242=ORIENTED_EDGE('',*,*,#9829,.T.);
#14243=ORIENTED_EDGE('',*,*,#9796,.F.);
#14244=ORIENTED_EDGE('',*,*,#9832,.F.);
#14245=ORIENTED_EDGE('',*,*,#9825,.T.);
#14246=ORIENTED_EDGE('',*,*,#9802,.F.);
#14247=ORIENTED_EDGE('',*,*,#9828,.F.);
#14248=ORIENTED_EDGE('',*,*,#9809,.T.);
#14249=ORIENTED_EDGE('',*,*,#9773,.F.);
#14250=ORIENTED_EDGE('',*,*,#9831,.F.);
#14251=ORIENTED_EDGE('',*,*,#9770,.T.);
#14252=ORIENTED_EDGE('',*,*,#9827,.F.);
#14253=TOROIDAL_SURFACE('',#15339,6.25,1.);
#14254=TOROIDAL_SURFACE('',#15387,4.5,0.75);
#14255=TOROIDAL_SURFACE('',#15496,2.2,0.40000000000004);
#14256=TOROIDAL_SURFACE('',#15859,9.,0.8);
#14257=TOROIDAL_SURFACE('',#15867,9.,0.8);
#14258=TOROIDAL_SURFACE('',#15875,3.5,0.8);
#14259=TOROIDAL_SURFACE('',#15878,4.,0.8);
#14260=TOROIDAL_SURFACE('',#15881,2.,0.8);
#14261=TOROIDAL_SURFACE('',#15884,15.,0.8);
#14262=TOROIDAL_SURFACE('',#15911,4.5,0.5);
#14263=TOROIDAL_SURFACE('',#15914,10.,0.5);
#14264=TOROIDAL_SURFACE('',#15917,6.5,0.5);
#14265=TOROIDAL_SURFACE('',#15930,3.3,0.5);
#14266=TOROIDAL_SURFACE('',#15934,4.,0.5);
#14267=TOROIDAL_SURFACE('',#15939,1.5,1.);
#14268=TOROIDAL_SURFACE('',#15956,16.5,0.5);
#14269=TOROIDAL_SURFACE('',#15959,3.,0.5);
#14270=TOROIDAL_SURFACE('',#15971,3.,0.5);
#14271=TOROIDAL_SURFACE('',#15974,5.5,0.5);
#14272=TOROIDAL_SURFACE('',#15977,11.,0.5);
#14273=TOROIDAL_SURFACE('',#15998,11.,0.5);
#14274=TOROIDAL_SURFACE('',#16005,6.5,0.5);
#14275=TOROIDAL_SURFACE('',#16008,1.5,0.5);
#14276=TOROIDAL_SURFACE('',#16025,3.,0.5);
#14277=TOROIDAL_SURFACE('',#16033,3.,0.5);
#14278=TOROIDAL_SURFACE('',#16048,16.5,0.5);
#14279=TOROIDAL_SURFACE('',#16051,16.5,0.5);
#14280=TOROIDAL_SURFACE('',#16054,3.,0.5);
#14281=TOROIDAL_SURFACE('',#16059,14.5,1.);
#14282=TOROIDAL_SURFACE('',#16066,10.,0.5);
#14283=TOROIDAL_SURFACE('',#16086,1.5,0.5);
#14284=TOROIDAL_SURFACE('',#16089,4.3,0.5);
#14285=TOROIDAL_SURFACE('',#16096,1.5,0.5);
#14286=TOROIDAL_SURFACE('',#16133,5.5,0.5);
#14287=TOROIDAL_SURFACE('',#16134,11.,0.5);
#14288=TOROIDAL_SURFACE('',#16138,5.5,0.5);
#14289=TOROIDAL_SURFACE('',#16142,1.5,1.);
#14290=TOROIDAL_SURFACE('',#16146,18.,1.);
#14291=TOROIDAL_SURFACE('',#16158,6.5,0.5);
#14292=TOROIDAL_SURFACE('',#16159,10.,0.5);
#14293=TOROIDAL_SURFACE('',#16160,10.,0.5);
#14294=TOROIDAL_SURFACE('',#16163,6.5,0.5);
#14295=TOROIDAL_SURFACE('',#16167,14.5,1.);
#14296=TOROIDAL_SURFACE('',#16489,17.0599057548774,0.5);
#14297=TOROIDAL_SURFACE('',#16502,2.20465088114115,0.3);
#14298=TOROIDAL_SURFACE('',#16510,16.5,3.);
#14299=TOROIDAL_SURFACE('',#16527,19.5,0.5);
#14300=TOROIDAL_SURFACE('',#16532,4.5,1.);
#14301=TOROIDAL_SURFACE('',#16537,19.5,0.5);
#14302=TOROIDAL_SURFACE('',#16543,17.5,1.);
#14303=TOROIDAL_SURFACE('',#16551,1.,0.5);
#14304=TOROIDAL_SURFACE('',#16561,6.,0.5);
#14305=TOROIDAL_SURFACE('',#16572,19.5,3.);
#14306=TOROIDAL_SURFACE('',#16632,19.5,5.);
#14307=TOROIDAL_SURFACE('',#16637,16.5,1.);
#14308=TOROIDAL_SURFACE('',#16671,17.,0.5);
#14309=TOROIDAL_SURFACE('',#16676,20.,1.);
#14310=TOROIDAL_SURFACE('',#16761,6.,0.5);
#14311=TOROIDAL_SURFACE('',#16767,19.5,3.);
#14312=TOROIDAL_SURFACE('',#16771,1.,0.5);
#14313=TOROIDAL_SURFACE('',#16820,17.5,1.);
#14314=TOROIDAL_SURFACE('',#16834,4.5,1.);
#14315=TOROIDAL_SURFACE('',#16838,20.,1.);
#14316=TOROIDAL_SURFACE('',#16842,19.5,3.);
#14317=TOROIDAL_SURFACE('',#16845,2.30308838114115,0.3);
#14318=TOROIDAL_SURFACE('',#16866,3.35,0.2);
#14319=TOROIDAL_SURFACE('',#16869,5.6,0.2);
#14320=TOROIDAL_SURFACE('',#16872,5.6,0.2);
#14321=TOROIDAL_SURFACE('',#16875,3.35,0.2);
#14322=TOROIDAL_SURFACE('',#16894,4.39999999999991,0.600000000000098);
#14323=TOROIDAL_SURFACE('',#16901,3.24999999999819,0.249999999998187);
#14324=TOROIDAL_SURFACE('',#16909,3.39999999999989,0.249999999999786);
#14325=ADVANCED_FACE('',(#3690),#14253,.F.);
#14326=ADVANCED_FACE('',(#3691),#3443,.T.);
#14327=ADVANCED_FACE('',(#3692),#3444,.T.);
#14328=ADVANCED_FACE('',(#3693),#3445,.F.);
#14329=ADVANCED_FACE('',(#3694),#3446,.F.);
#14330=ADVANCED_FACE('',(#3695),#1032,.T.);
#14331=ADVANCED_FACE('',(#3696),#3447,.T.);
#14332=ADVANCED_FACE('',(#3697),#3448,.T.);
#14333=ADVANCED_FACE('',(#3698),#3449,.T.);
#14334=ADVANCED_FACE('',(#3699),#3450,.T.);
#14335=ADVANCED_FACE('',(#3700),#3451,.T.);
#14336=ADVANCED_FACE('',(#3701),#1033,.T.);
#14337=ADVANCED_FACE('',(#3702),#3452,.F.);
#14338=ADVANCED_FACE('',(#3703),#3453,.F.);
#14339=ADVANCED_FACE('',(#3704),#3454,.F.);
#14340=ADVANCED_FACE('',(#3705),#14254,.T.);
#14341=ADVANCED_FACE('',(#3706),#3455,.T.);
#14342=ADVANCED_FACE('',(#3707),#1034,.T.);
#14343=ADVANCED_FACE('',(#3708),#3456,.F.);
#14344=ADVANCED_FACE('',(#3709,#194),#279,.F.);
#14345=ADVANCED_FACE('',(#3710,#195),#280,.F.);
#14346=ADVANCED_FACE('',(#3711,#196),#281,.F.);
#14347=ADVANCED_FACE('',(#3712),#282,.T.);
#14348=ADVANCED_FACE('',(#3713),#283,.F.);
#14349=ADVANCED_FACE('',(#3714),#284,.F.);
#14350=ADVANCED_FACE('',(#3715),#285,.T.);
#14351=ADVANCED_FACE('',(#3716),#286,.T.);
#14352=ADVANCED_FACE('',(#3717),#287,.T.);
#14353=ADVANCED_FACE('',(#3718),#288,.F.);
#14354=ADVANCED_FACE('',(#3719),#289,.T.);
#14355=ADVANCED_FACE('',(#3720),#290,.T.);
#14356=ADVANCED_FACE('',(#3721),#291,.T.);
#14357=ADVANCED_FACE('',(#3722),#292,.T.);
#14358=ADVANCED_FACE('',(#3723),#293,.T.);
#14359=ADVANCED_FACE('',(#3724),#294,.T.);
#14360=ADVANCED_FACE('',(#3725),#295,.T.);
#14361=ADVANCED_FACE('',(#3726),#296,.T.);
#14362=ADVANCED_FACE('',(#3727),#297,.T.);
#14363=ADVANCED_FACE('',(#3728),#298,.T.);
#14364=ADVANCED_FACE('',(#3729),#299,.F.);
#14365=ADVANCED_FACE('',(#3730),#300,.F.);
#14366=ADVANCED_FACE('',(#3731),#301,.F.);
#14367=ADVANCED_FACE('',(#3732),#302,.F.);
#14368=ADVANCED_FACE('',(#3733,#197),#303,.T.);
#14369=ADVANCED_FACE('',(#3734),#304,.F.);
#14370=ADVANCED_FACE('',(#3735),#305,.F.);
#14371=ADVANCED_FACE('',(#3736),#306,.F.);
#14372=ADVANCED_FACE('',(#3737),#307,.T.);
#14373=ADVANCED_FACE('',(#3738),#308,.F.);
#14374=ADVANCED_FACE('',(#3739),#309,.F.);
#14375=ADVANCED_FACE('',(#3740),#310,.F.);
#14376=ADVANCED_FACE('',(#3741),#311,.F.);
#14377=ADVANCED_FACE('',(#3742),#312,.T.);
#14378=ADVANCED_FACE('',(#3743),#313,.F.);
#14379=ADVANCED_FACE('',(#3744),#314,.F.);
#14380=ADVANCED_FACE('',(#3745),#315,.F.);
#14381=ADVANCED_FACE('',(#3746),#316,.T.);
#14382=ADVANCED_FACE('',(#3747),#317,.T.);
#14383=ADVANCED_FACE('',(#3748),#318,.T.);
#14384=ADVANCED_FACE('',(#3749),#319,.T.);
#14385=ADVANCED_FACE('',(#3750),#320,.T.);
#14386=ADVANCED_FACE('',(#3751,#198),#321,.T.);
#14387=ADVANCED_FACE('',(#3752),#192,.T.);
#14388=ADVANCED_FACE('',(#3753),#146,.F.);
#14389=ADVANCED_FACE('',(#3754),#193,.T.);
#14390=ADVANCED_FACE('',(#3755),#3457,.T.);
#14391=ADVANCED_FACE('',(#3756),#322,.T.);
#14392=ADVANCED_FACE('',(#3757),#3458,.T.);
#14393=ADVANCED_FACE('',(#3758),#323,.T.);
#14394=ADVANCED_FACE('',(#3759,#199),#324,.T.);
#14395=ADVANCED_FACE('',(#3760),#325,.T.);
#14396=ADVANCED_FACE('',(#3761),#326,.T.);
#14397=ADVANCED_FACE('',(#3762),#327,.F.);
#14398=ADVANCED_FACE('',(#3763),#328,.T.);
#14399=ADVANCED_FACE('',(#3764,#200,#201),#329,.T.);
#14400=ADVANCED_FACE('',(#3765),#330,.F.);
#14401=ADVANCED_FACE('',(#3766,#202,#203),#331,.F.);
#14402=ADVANCED_FACE('',(#3767,#204,#205),#332,.F.);
#14403=ADVANCED_FACE('',(#3768,#206),#333,.T.);
#14404=ADVANCED_FACE('',(#3769),#334,.F.);
#14405=ADVANCED_FACE('',(#3770),#335,.F.);
#14406=ADVANCED_FACE('',(#3771,#207,#208),#336,.T.);
#14407=ADVANCED_FACE('',(#3772,#209),#337,.F.);
#14408=ADVANCED_FACE('',(#3773),#338,.F.);
#14409=ADVANCED_FACE('',(#3774),#339,.T.);
#14410=ADVANCED_FACE('',(#3775),#340,.F.);
#14411=ADVANCED_FACE('',(#3776),#341,.F.);
#14412=ADVANCED_FACE('',(#3777),#3459,.T.);
#14413=ADVANCED_FACE('',(#3778,#210),#79,.T.);
#14414=ADVANCED_FACE('',(#3779),#14255,.F.);
#14415=ADVANCED_FACE('',(#3780),#1035,.T.);
#14416=ADVANCED_FACE('',(#3781),#1036,.T.);
#14417=ADVANCED_FACE('',(#3782),#3460,.T.);
#14418=ADVANCED_FACE('',(#3783),#342,.T.);
#14419=ADVANCED_FACE('',(#3784,#211),#343,.T.);
#14420=ADVANCED_FACE('',(#3785),#344,.F.);
#14421=ADVANCED_FACE('',(#3786),#345,.F.);
#14422=ADVANCED_FACE('',(#3787),#346,.F.);
#14423=ADVANCED_FACE('',(#3788),#347,.F.);
#14424=ADVANCED_FACE('',(#3789),#348,.F.);
#14425=ADVANCED_FACE('',(#3790),#349,.F.);
#14426=ADVANCED_FACE('',(#3791),#350,.F.);
#14427=ADVANCED_FACE('',(#3792),#351,.F.);
#14428=ADVANCED_FACE('',(#3793),#352,.F.);
#14429=ADVANCED_FACE('',(#3794),#353,.F.);
#14430=ADVANCED_FACE('',(#3795),#354,.F.);
#14431=ADVANCED_FACE('',(#3796),#355,.F.);
#14432=ADVANCED_FACE('',(#3797),#356,.F.);
#14433=ADVANCED_FACE('',(#3798),#357,.F.);
#14434=ADVANCED_FACE('',(#3799),#358,.F.);
#14435=ADVANCED_FACE('',(#3800),#359,.F.);
#14436=ADVANCED_FACE('',(#3801),#360,.F.);
#14437=ADVANCED_FACE('',(#3802),#361,.F.);
#14438=ADVANCED_FACE('',(#3803),#362,.F.);
#14439=ADVANCED_FACE('',(#3804),#363,.F.);
#14440=ADVANCED_FACE('',(#3805),#364,.F.);
#14441=ADVANCED_FACE('',(#3806),#147,.F.);
#14442=ADVANCED_FACE('',(#3807),#3461,.T.);
#14443=ADVANCED_FACE('',(#3808,#212),#80,.T.);
#14444=ADVANCED_FACE('',(#3809,#213,#214,#215),#3462,.T.);
#14445=ADVANCED_FACE('',(#3810,#216),#81,.T.);
#14446=ADVANCED_FACE('',(#3811),#3463,.T.);
#14447=ADVANCED_FACE('',(#3812),#365,.F.);
#14448=ADVANCED_FACE('',(#3813),#366,.F.);
#14449=ADVANCED_FACE('',(#3814),#367,.F.);
#14450=ADVANCED_FACE('',(#3815),#368,.T.);
#14451=ADVANCED_FACE('',(#3816),#369,.F.);
#14452=ADVANCED_FACE('',(#3817),#370,.F.);
#14453=ADVANCED_FACE('',(#3818),#371,.F.);
#14454=ADVANCED_FACE('',(#3819),#372,.F.);
#14455=ADVANCED_FACE('',(#3820),#373,.F.);
#14456=ADVANCED_FACE('',(#3821),#374,.F.);
#14457=ADVANCED_FACE('',(#3822),#375,.F.);
#14458=ADVANCED_FACE('',(#3823),#376,.F.);
#14459=ADVANCED_FACE('',(#3824),#377,.F.);
#14460=ADVANCED_FACE('',(#3825),#378,.F.);
#14461=ADVANCED_FACE('',(#3826),#379,.F.);
#14462=ADVANCED_FACE('',(#3827),#380,.F.);
#14463=ADVANCED_FACE('',(#3828),#381,.F.);
#14464=ADVANCED_FACE('',(#3829),#382,.F.);
#14465=ADVANCED_FACE('',(#3830),#383,.F.);
#14466=ADVANCED_FACE('',(#3831),#384,.F.);
#14467=ADVANCED_FACE('',(#3832),#385,.F.);
#14468=ADVANCED_FACE('',(#3833),#386,.F.);
#14469=ADVANCED_FACE('',(#3834),#387,.F.);
#14470=ADVANCED_FACE('',(#3835),#388,.F.);
#14471=ADVANCED_FACE('',(#3836),#389,.F.);
#14472=ADVANCED_FACE('',(#3837),#390,.T.);
#14473=ADVANCED_FACE('',(#3838),#391,.F.);
#14474=ADVANCED_FACE('',(#3839),#392,.F.);
#14475=ADVANCED_FACE('',(#3840),#393,.F.);
#14476=ADVANCED_FACE('',(#3841),#394,.F.);
#14477=ADVANCED_FACE('',(#3842),#395,.T.);
#14478=ADVANCED_FACE('',(#3843),#396,.T.);
#14479=ADVANCED_FACE('',(#3844),#397,.F.);
#14480=ADVANCED_FACE('',(#3845),#398,.F.);
#14481=ADVANCED_FACE('',(#3846),#399,.T.);
#14482=ADVANCED_FACE('',(#3847),#400,.T.);
#14483=ADVANCED_FACE('',(#3848),#401,.F.);
#14484=ADVANCED_FACE('',(#3849),#402,.F.);
#14485=ADVANCED_FACE('',(#3850),#403,.F.);
#14486=ADVANCED_FACE('',(#3851),#404,.F.);
#14487=ADVANCED_FACE('',(#3852),#405,.F.);
#14488=ADVANCED_FACE('',(#3853),#406,.F.);
#14489=ADVANCED_FACE('',(#3854),#407,.F.);
#14490=ADVANCED_FACE('',(#3855),#408,.F.);
#14491=ADVANCED_FACE('',(#3856),#409,.F.);
#14492=ADVANCED_FACE('',(#3857),#410,.F.);
#14493=ADVANCED_FACE('',(#3858),#411,.F.);
#14494=ADVANCED_FACE('',(#3859),#412,.F.);
#14495=ADVANCED_FACE('',(#3860),#413,.F.);
#14496=ADVANCED_FACE('',(#3861),#414,.F.);
#14497=ADVANCED_FACE('',(#3862),#415,.F.);
#14498=ADVANCED_FACE('',(#3863),#416,.F.);
#14499=ADVANCED_FACE('',(#3864),#417,.F.);
#14500=ADVANCED_FACE('',(#3865),#418,.F.);
#14501=ADVANCED_FACE('',(#3866),#419,.F.);
#14502=ADVANCED_FACE('',(#3867),#420,.F.);
#14503=ADVANCED_FACE('',(#3868),#421,.F.);
#14504=ADVANCED_FACE('',(#3869),#422,.F.);
#14505=ADVANCED_FACE('',(#3870),#423,.F.);
#14506=ADVANCED_FACE('',(#3871),#424,.F.);
#14507=ADVANCED_FACE('',(#3872),#425,.T.);
#14508=ADVANCED_FACE('',(#3873),#426,.T.);
#14509=ADVANCED_FACE('',(#3874),#427,.F.);
#14510=ADVANCED_FACE('',(#3875),#428,.T.);
#14511=ADVANCED_FACE('',(#3876),#429,.F.);
#14512=ADVANCED_FACE('',(#3877),#148,.F.);
#14513=ADVANCED_FACE('',(#3878),#430,.T.);
#14514=ADVANCED_FACE('',(#3879),#3464,.T.);
#14515=ADVANCED_FACE('',(#3880),#3465,.F.);
#14516=ADVANCED_FACE('',(#3881),#3466,.F.);
#14517=ADVANCED_FACE('',(#3882),#3467,.F.);
#14518=ADVANCED_FACE('',(#3883),#3468,.T.);
#14519=ADVANCED_FACE('',(#3884),#431,.F.);
#14520=ADVANCED_FACE('',(#3885),#432,.F.);
#14521=ADVANCED_FACE('',(#3886),#433,.F.);
#14522=ADVANCED_FACE('',(#3887),#434,.F.);
#14523=ADVANCED_FACE('',(#3888),#435,.T.);
#14524=ADVANCED_FACE('',(#3889),#436,.T.);
#14525=ADVANCED_FACE('',(#3890),#437,.F.);
#14526=ADVANCED_FACE('',(#3891),#438,.F.);
#14527=ADVANCED_FACE('',(#3892),#439,.F.);
#14528=ADVANCED_FACE('',(#3893),#440,.F.);
#14529=ADVANCED_FACE('',(#3894),#441,.T.);
#14530=ADVANCED_FACE('',(#3895),#442,.T.);
#14531=ADVANCED_FACE('',(#3896),#443,.F.);
#14532=ADVANCED_FACE('',(#3897),#444,.F.);
#14533=ADVANCED_FACE('',(#3898),#445,.T.);
#14534=ADVANCED_FACE('',(#3899),#446,.F.);
#14535=ADVANCED_FACE('',(#3900),#447,.F.);
#14536=ADVANCED_FACE('',(#3901),#448,.F.);
#14537=ADVANCED_FACE('',(#3902),#449,.F.);
#14538=ADVANCED_FACE('',(#3903),#450,.T.);
#14539=ADVANCED_FACE('',(#3904),#451,.T.);
#14540=ADVANCED_FACE('',(#3905),#452,.T.);
#14541=ADVANCED_FACE('',(#3906),#453,.T.);
#14542=ADVANCED_FACE('',(#3907),#454,.T.);
#14543=ADVANCED_FACE('',(#3908),#455,.T.);
#14544=ADVANCED_FACE('',(#3909),#1037,.F.);
#14545=ADVANCED_FACE('',(#3910),#456,.F.);
#14546=ADVANCED_FACE('',(#3911),#457,.F.);
#14547=ADVANCED_FACE('',(#3912),#1038,.F.);
#14548=ADVANCED_FACE('',(#3913),#1039,.F.);
#14549=ADVANCED_FACE('',(#3914),#458,.F.);
#14550=ADVANCED_FACE('',(#3915),#459,.F.);
#14551=ADVANCED_FACE('',(#3916),#460,.F.);
#14552=ADVANCED_FACE('',(#3917),#1040,.F.);
#14553=ADVANCED_FACE('',(#3918),#461,.T.);
#14554=ADVANCED_FACE('',(#3919),#462,.T.);
#14555=ADVANCED_FACE('',(#3920),#463,.T.);
#14556=ADVANCED_FACE('',(#3921),#464,.F.);
#14557=ADVANCED_FACE('',(#3922),#465,.T.);
#14558=ADVANCED_FACE('',(#3923),#466,.T.);
#14559=ADVANCED_FACE('',(#3924),#3469,.T.);
#14560=ADVANCED_FACE('',(#3925),#467,.T.);
#14561=ADVANCED_FACE('',(#3926),#3470,.T.);
#14562=ADVANCED_FACE('',(#3927),#3471,.T.);
#14563=ADVANCED_FACE('',(#3928),#468,.T.);
#14564=ADVANCED_FACE('',(#3929),#3472,.T.);
#14565=ADVANCED_FACE('',(#3930),#3473,.T.);
#14566=ADVANCED_FACE('',(#3931),#469,.T.);
#14567=ADVANCED_FACE('',(#3932),#3474,.T.);
#14568=ADVANCED_FACE('',(#3933),#3475,.T.);
#14569=ADVANCED_FACE('',(#3934),#470,.F.);
#14570=ADVANCED_FACE('',(#3935,#217),#471,.T.);
#14571=ADVANCED_FACE('',(#3936,#218),#472,.T.);
#14572=ADVANCED_FACE('',(#3937),#473,.T.);
#14573=ADVANCED_FACE('',(#3938),#474,.T.);
#14574=ADVANCED_FACE('',(#3939,#219),#475,.F.);
#14575=ADVANCED_FACE('',(#3940),#476,.T.);
#14576=ADVANCED_FACE('',(#3941),#477,.T.);
#14577=ADVANCED_FACE('',(#3942),#478,.T.);
#14578=ADVANCED_FACE('',(#3943),#479,.T.);
#14579=ADVANCED_FACE('',(#3944),#480,.T.);
#14580=ADVANCED_FACE('',(#3945),#481,.F.);
#14581=ADVANCED_FACE('',(#3946),#482,.T.);
#14582=ADVANCED_FACE('',(#3947),#483,.T.);
#14583=ADVANCED_FACE('',(#3948),#484,.T.);
#14584=ADVANCED_FACE('',(#3949),#485,.F.);
#14585=ADVANCED_FACE('',(#3950),#486,.F.);
#14586=ADVANCED_FACE('',(#3951),#487,.F.);
#14587=ADVANCED_FACE('',(#3952),#488,.F.);
#14588=ADVANCED_FACE('',(#3953),#489,.T.);
#14589=ADVANCED_FACE('',(#3954),#490,.T.);
#14590=ADVANCED_FACE('',(#3955),#491,.T.);
#14591=ADVANCED_FACE('',(#3956),#492,.T.);
#14592=ADVANCED_FACE('',(#3957),#493,.T.);
#14593=ADVANCED_FACE('',(#3958),#3476,.T.);
#14594=ADVANCED_FACE('',(#3959),#3477,.T.);
#14595=ADVANCED_FACE('',(#3960),#494,.T.);
#14596=ADVANCED_FACE('',(#3961),#495,.T.);
#14597=ADVANCED_FACE('',(#3962),#496,.T.);
#14598=ADVANCED_FACE('',(#3963),#497,.T.);
#14599=ADVANCED_FACE('',(#3964),#498,.T.);
#14600=ADVANCED_FACE('',(#3965),#499,.T.);
#14601=ADVANCED_FACE('',(#3966),#3478,.T.);
#14602=ADVANCED_FACE('',(#3967),#3479,.T.);
#14603=ADVANCED_FACE('',(#3968),#500,.T.);
#14604=ADVANCED_FACE('',(#3969),#501,.T.);
#14605=ADVANCED_FACE('',(#3970),#502,.T.);
#14606=ADVANCED_FACE('',(#3971,#220),#503,.F.);
#14607=ADVANCED_FACE('',(#3972),#504,.T.);
#14608=ADVANCED_FACE('',(#3973),#505,.T.);
#14609=ADVANCED_FACE('',(#3974),#506,.F.);
#14610=ADVANCED_FACE('',(#3975),#3480,.F.);
#14611=ADVANCED_FACE('',(#3976),#3481,.F.);
#14612=ADVANCED_FACE('',(#3977),#507,.F.);
#14613=ADVANCED_FACE('',(#3978),#508,.T.);
#14614=ADVANCED_FACE('',(#3979),#509,.F.);
#14615=ADVANCED_FACE('',(#3980),#510,.T.);
#14616=ADVANCED_FACE('',(#3981),#511,.F.);
#14617=ADVANCED_FACE('',(#3982),#512,.F.);
#14618=ADVANCED_FACE('',(#3983),#3482,.F.);
#14619=ADVANCED_FACE('',(#3984),#513,.F.);
#14620=ADVANCED_FACE('',(#3985),#3483,.F.);
#14621=ADVANCED_FACE('',(#3986),#514,.F.);
#14622=ADVANCED_FACE('',(#3987),#3484,.F.);
#14623=ADVANCED_FACE('',(#3988),#3485,.F.);
#14624=ADVANCED_FACE('',(#3989),#515,.F.);
#14625=ADVANCED_FACE('',(#3990),#516,.F.);
#14626=ADVANCED_FACE('',(#3991),#517,.F.);
#14627=ADVANCED_FACE('',(#3992),#518,.F.);
#14628=ADVANCED_FACE('',(#3993),#519,.T.);
#14629=ADVANCED_FACE('',(#3994),#520,.F.);
#14630=ADVANCED_FACE('',(#3995),#521,.F.);
#14631=ADVANCED_FACE('',(#3996),#522,.F.);
#14632=ADVANCED_FACE('',(#3997),#523,.T.);
#14633=ADVANCED_FACE('',(#3998),#524,.T.);
#14634=ADVANCED_FACE('',(#3999),#525,.F.);
#14635=ADVANCED_FACE('',(#4000),#526,.F.);
#14636=ADVANCED_FACE('',(#4001),#527,.F.);
#14637=ADVANCED_FACE('',(#4002),#528,.T.);
#14638=ADVANCED_FACE('',(#4003,#221,#222,#223),#529,.T.);
#14639=ADVANCED_FACE('',(#4004),#14256,.T.);
#14640=ADVANCED_FACE('',(#4005),#14257,.T.);
#14641=ADVANCED_FACE('',(#4006),#14258,.T.);
#14642=ADVANCED_FACE('',(#4007),#14259,.T.);
#14643=ADVANCED_FACE('',(#4008),#14260,.T.);
#14644=ADVANCED_FACE('',(#4009),#14261,.T.);
#14645=ADVANCED_FACE('',(#4010),#3486,.T.);
#14646=ADVANCED_FACE('',(#4011),#1041,.T.);
#14647=ADVANCED_FACE('',(#4012),#3487,.T.);
#14648=ADVANCED_FACE('',(#4013),#3488,.F.);
#14649=ADVANCED_FACE('',(#4014,#224),#3489,.T.);
#14650=ADVANCED_FACE('',(#4015),#14262,.T.);
#14651=ADVANCED_FACE('',(#4016),#14263,.F.);
#14652=ADVANCED_FACE('',(#4017),#14264,.F.);
#14653=ADVANCED_FACE('',(#4018),#3490,.T.);
#14654=ADVANCED_FACE('',(#4019),#3491,.T.);
#14655=ADVANCED_FACE('',(#4020),#14265,.T.);
#14656=ADVANCED_FACE('',(#4021),#14266,.T.);
#14657=ADVANCED_FACE('',(#4022),#14267,.T.);
#14658=ADVANCED_FACE('',(#4023),#3492,.F.);
#14659=ADVANCED_FACE('',(#4024),#3493,.T.);
#14660=ADVANCED_FACE('',(#4025),#3494,.T.);
#14661=ADVANCED_FACE('',(#4026),#3495,.T.);
#14662=ADVANCED_FACE('',(#4027),#14268,.T.);
#14663=ADVANCED_FACE('',(#4028),#14269,.F.);
#14664=ADVANCED_FACE('',(#4029),#3496,.T.);
#14665=ADVANCED_FACE('',(#4030),#3497,.T.);
#14666=ADVANCED_FACE('',(#4031),#14270,.F.);
#14667=ADVANCED_FACE('',(#4032),#14271,.T.);
#14668=ADVANCED_FACE('',(#4033),#14272,.T.);
#14669=ADVANCED_FACE('',(#4034),#149,.F.);
#14670=ADVANCED_FACE('',(#4035),#150,.T.);
#14671=ADVANCED_FACE('',(#4036),#151,.T.);
#14672=ADVANCED_FACE('',(#4037),#3498,.T.);
#14673=ADVANCED_FACE('',(#4038),#3499,.T.);
#14674=ADVANCED_FACE('',(#4039),#530,.F.);
#14675=ADVANCED_FACE('',(#4040),#152,.T.);
#14676=ADVANCED_FACE('',(#4041),#153,.T.);
#14677=ADVANCED_FACE('',(#4042),#531,.T.);
#14678=ADVANCED_FACE('',(#4043),#154,.F.);
#14679=ADVANCED_FACE('',(#4044),#3500,.T.);
#14680=ADVANCED_FACE('',(#4045),#532,.F.);
#14681=ADVANCED_FACE('',(#4046),#533,.F.);
#14682=ADVANCED_FACE('',(#4047),#534,.F.);
#14683=ADVANCED_FACE('',(#4048),#535,.F.);
#14684=ADVANCED_FACE('',(#4049),#536,.F.);
#14685=ADVANCED_FACE('',(#4050),#537,.F.);
#14686=ADVANCED_FACE('',(#4051),#538,.T.);
#14687=ADVANCED_FACE('',(#4052),#3501,.T.);
#14688=ADVANCED_FACE('',(#4053),#3502,.T.);
#14689=ADVANCED_FACE('',(#4054),#14273,.T.);
#14690=ADVANCED_FACE('',(#4055),#3503,.T.);
#14691=ADVANCED_FACE('',(#4056),#3504,.T.);
#14692=ADVANCED_FACE('',(#4057),#3505,.F.);
#14693=ADVANCED_FACE('',(#4058),#3506,.F.);
#14694=ADVANCED_FACE('',(#4059),#14274,.F.);
#14695=ADVANCED_FACE('',(#4060),#14275,.T.);
#14696=ADVANCED_FACE('',(#4061),#3507,.T.);
#14697=ADVANCED_FACE('',(#4062),#539,.T.);
#14698=ADVANCED_FACE('',(#4063),#155,.F.);
#14699=ADVANCED_FACE('',(#4064),#3508,.F.);
#14700=ADVANCED_FACE('',(#4065),#156,.F.);
#14701=ADVANCED_FACE('',(#4066),#540,.F.);
#14702=ADVANCED_FACE('',(#4067),#541,.F.);
#14703=ADVANCED_FACE('',(#4068),#542,.T.);
#14704=ADVANCED_FACE('',(#4069),#14276,.F.);
#14705=ADVANCED_FACE('',(#4070),#543,.F.);
#14706=ADVANCED_FACE('',(#4071),#544,.T.);
#14707=ADVANCED_FACE('',(#4072),#545,.F.);
#14708=ADVANCED_FACE('',(#4073),#546,.T.);
#14709=ADVANCED_FACE('',(#4074),#14277,.F.);
#14710=ADVANCED_FACE('',(#4075),#3509,.F.);
#14711=ADVANCED_FACE('',(#4076),#157,.F.);
#14712=ADVANCED_FACE('',(#4077),#3510,.T.);
#14713=ADVANCED_FACE('',(#4078),#3511,.F.);
#14714=ADVANCED_FACE('',(#4079),#158,.F.);
#14715=ADVANCED_FACE('',(#4080),#3512,.F.);
#14716=ADVANCED_FACE('',(#4081),#159,.F.);
#14717=ADVANCED_FACE('',(#4082),#547,.F.);
#14718=ADVANCED_FACE('',(#4083),#548,.F.);
#14719=ADVANCED_FACE('',(#4084),#160,.F.);
#14720=ADVANCED_FACE('',(#4085),#14278,.T.);
#14721=ADVANCED_FACE('',(#4086),#14279,.T.);
#14722=ADVANCED_FACE('',(#4087),#14280,.F.);
#14723=ADVANCED_FACE('',(#4088),#161,.F.);
#14724=ADVANCED_FACE('',(#4089),#3513,.F.);
#14725=ADVANCED_FACE('',(#4090),#14281,.F.);
#14726=ADVANCED_FACE('',(#4091),#3514,.T.);
#14727=ADVANCED_FACE('',(#4092),#549,.F.);
#14728=ADVANCED_FACE('',(#4093),#14282,.T.);
#14729=ADVANCED_FACE('',(#4094),#3515,.F.);
#14730=ADVANCED_FACE('',(#4095),#3516,.F.);
#14731=ADVANCED_FACE('',(#4096),#3517,.F.);
#14732=ADVANCED_FACE('',(#4097),#550,.T.);
#14733=ADVANCED_FACE('',(#4098),#551,.T.);
#14734=ADVANCED_FACE('',(#4099),#552,.F.);
#14735=ADVANCED_FACE('',(#4100),#553,.F.);
#14736=ADVANCED_FACE('',(#4101),#3518,.F.);
#14737=ADVANCED_FACE('',(#4102),#162,.T.);
#14738=ADVANCED_FACE('',(#4103),#163,.T.);
#14739=ADVANCED_FACE('',(#4104),#3519,.F.);
#14740=ADVANCED_FACE('',(#4105),#14283,.T.);
#14741=ADVANCED_FACE('',(#4106),#14284,.F.);
#14742=ADVANCED_FACE('',(#4107),#3520,.T.);
#14743=ADVANCED_FACE('',(#4108),#164,.F.);
#14744=ADVANCED_FACE('',(#4109),#3521,.T.);
#14745=ADVANCED_FACE('',(#4110),#14285,.T.);
#14746=ADVANCED_FACE('',(#4111),#554,.T.);
#14747=ADVANCED_FACE('',(#4112),#555,.T.);
#14748=ADVANCED_FACE('',(#4113,#225,#226,#227,#228),#556,.F.);
#14749=ADVANCED_FACE('',(#4114,#229),#557,.F.);
#14750=ADVANCED_FACE('',(#4115),#558,.F.);
#14751=ADVANCED_FACE('',(#4116),#3522,.F.);
#14752=ADVANCED_FACE('',(#4117),#3523,.F.);
#14753=ADVANCED_FACE('',(#4118),#559,.F.);
#14754=ADVANCED_FACE('',(#4119),#560,.F.);
#14755=ADVANCED_FACE('',(#4120),#561,.F.);
#14756=ADVANCED_FACE('',(#4121),#562,.F.);
#14757=ADVANCED_FACE('',(#4122),#3524,.T.);
#14758=ADVANCED_FACE('',(#4123),#3525,.F.);
#14759=ADVANCED_FACE('',(#4124),#3526,.T.);
#14760=ADVANCED_FACE('',(#4125),#3527,.T.);
#14761=ADVANCED_FACE('',(#4126),#14286,.T.);
#14762=ADVANCED_FACE('',(#4127),#14287,.T.);
#14763=ADVANCED_FACE('',(#4128),#3528,.T.);
#14764=ADVANCED_FACE('',(#4129),#3529,.T.);
#14765=ADVANCED_FACE('',(#4130),#3530,.T.);
#14766=ADVANCED_FACE('',(#4131),#14288,.T.);
#14767=ADVANCED_FACE('',(#4132),#3531,.T.);
#14768=ADVANCED_FACE('',(#4133),#563,.T.);
#14769=ADVANCED_FACE('',(#4134),#3532,.T.);
#14770=ADVANCED_FACE('',(#4135),#14289,.T.);
#14771=ADVANCED_FACE('',(#4136),#3533,.T.);
#14772=ADVANCED_FACE('',(#4137),#3534,.T.);
#14773=ADVANCED_FACE('',(#4138),#14290,.F.);
#14774=ADVANCED_FACE('',(#4139,#230),#564,.F.);
#14775=ADVANCED_FACE('',(#4140),#3535,.T.);
#14776=ADVANCED_FACE('',(#4141),#3536,.T.);
#14777=ADVANCED_FACE('',(#4142),#165,.T.);
#14778=ADVANCED_FACE('',(#4143),#166,.T.);
#14779=ADVANCED_FACE('',(#4144),#3537,.T.);
#14780=ADVANCED_FACE('',(#4145,#231),#565,.T.);
#14781=ADVANCED_FACE('',(#4146),#566,.F.);
#14782=ADVANCED_FACE('',(#4147),#3538,.F.);
#14783=ADVANCED_FACE('',(#4148),#3539,.F.);
#14784=ADVANCED_FACE('',(#4149),#167,.T.);
#14785=ADVANCED_FACE('',(#4150),#14291,.F.);
#14786=ADVANCED_FACE('',(#4151),#14292,.F.);
#14787=ADVANCED_FACE('',(#4152),#14293,.F.);
#14788=ADVANCED_FACE('',(#4153),#3540,.F.);
#14789=ADVANCED_FACE('',(#4154),#3541,.F.);
#14790=ADVANCED_FACE('',(#4155),#14294,.F.);
#14791=ADVANCED_FACE('',(#4156),#3542,.F.);
#14792=ADVANCED_FACE('',(#4157),#3543,.T.);
#14793=ADVANCED_FACE('',(#4158),#14295,.F.);
#14794=ADVANCED_FACE('',(#4159),#567,.T.);
#14795=ADVANCED_FACE('',(#4160),#568,.F.);
#14796=ADVANCED_FACE('',(#4161),#569,.F.);
#14797=ADVANCED_FACE('',(#4162),#570,.F.);
#14798=ADVANCED_FACE('',(#4163),#3544,.T.);
#14799=ADVANCED_FACE('',(#4164),#571,.F.);
#14800=ADVANCED_FACE('',(#4165),#572,.F.);
#14801=ADVANCED_FACE('',(#4166),#573,.T.);
#14802=ADVANCED_FACE('',(#4167,#232),#82,.T.);
#14803=ADVANCED_FACE('',(#4168),#1042,.T.);
#14804=ADVANCED_FACE('',(#4169),#3545,.T.);
#14805=ADVANCED_FACE('',(#4170),#3546,.T.);
#14806=ADVANCED_FACE('',(#4171,#233),#574,.T.);
#14807=ADVANCED_FACE('',(#4172),#575,.T.);
#14808=ADVANCED_FACE('',(#4173),#576,.T.);
#14809=ADVANCED_FACE('',(#4174),#577,.T.);
#14810=ADVANCED_FACE('',(#4175),#578,.T.);
#14811=ADVANCED_FACE('',(#4176),#579,.T.);
#14812=ADVANCED_FACE('',(#4177),#580,.T.);
#14813=ADVANCED_FACE('',(#4178),#581,.T.);
#14814=ADVANCED_FACE('',(#4179),#582,.T.);
#14815=ADVANCED_FACE('',(#4180),#583,.T.);
#14816=ADVANCED_FACE('',(#4181),#584,.T.);
#14817=ADVANCED_FACE('',(#4182),#585,.T.);
#14818=ADVANCED_FACE('',(#4183),#586,.T.);
#14819=ADVANCED_FACE('',(#4184),#587,.F.);
#14820=ADVANCED_FACE('',(#4185),#588,.T.);
#14821=ADVANCED_FACE('',(#4186),#3547,.T.);
#14822=ADVANCED_FACE('',(#4187),#3548,.T.);
#14823=ADVANCED_FACE('',(#4188),#3549,.T.);
#14824=ADVANCED_FACE('',(#4189),#3550,.T.);
#14825=ADVANCED_FACE('',(#4190),#3551,.T.);
#14826=ADVANCED_FACE('',(#4191),#3552,.T.);
#14827=ADVANCED_FACE('',(#4192),#3553,.F.);
#14828=ADVANCED_FACE('',(#4193),#3554,.T.);
#14829=ADVANCED_FACE('',(#4194),#3555,.F.);
#14830=ADVANCED_FACE('',(#4195),#3556,.T.);
#14831=ADVANCED_FACE('',(#4196),#3557,.T.);
#14832=ADVANCED_FACE('',(#4197),#3558,.T.);
#14833=ADVANCED_FACE('',(#4198),#3559,.T.);
#14834=ADVANCED_FACE('',(#4199),#3560,.T.);
#14835=ADVANCED_FACE('',(#4200),#3561,.T.);
#14836=ADVANCED_FACE('',(#4201),#3562,.T.);
#14837=ADVANCED_FACE('',(#4202),#3563,.T.);
#14838=ADVANCED_FACE('',(#4203),#3564,.F.);
#14839=ADVANCED_FACE('',(#4204),#3565,.T.);
#14840=ADVANCED_FACE('',(#4205,#234),#589,.T.);
#14841=ADVANCED_FACE('',(#4206),#590,.T.);
#14842=ADVANCED_FACE('',(#4207),#591,.F.);
#14843=ADVANCED_FACE('',(#4208),#3566,.T.);
#14844=ADVANCED_FACE('',(#4209),#592,.F.);
#14845=ADVANCED_FACE('',(#4210),#593,.T.);
#14846=ADVANCED_FACE('',(#4211),#3567,.F.);
#14847=ADVANCED_FACE('',(#4212),#594,.T.);
#14848=ADVANCED_FACE('',(#4213),#3568,.T.);
#14849=ADVANCED_FACE('',(#4214),#3569,.F.);
#14850=ADVANCED_FACE('',(#4215),#3570,.T.);
#14851=ADVANCED_FACE('',(#4216),#595,.T.);
#14852=ADVANCED_FACE('',(#4217),#596,.T.);
#14853=ADVANCED_FACE('',(#4218),#597,.T.);
#14854=ADVANCED_FACE('',(#4219),#3571,.T.);
#14855=ADVANCED_FACE('',(#4220),#598,.F.);
#14856=ADVANCED_FACE('',(#4221),#599,.F.);
#14857=ADVANCED_FACE('',(#4222),#3572,.T.);
#14858=ADVANCED_FACE('',(#4223),#600,.T.);
#14859=ADVANCED_FACE('',(#4224),#601,.T.);
#14860=ADVANCED_FACE('',(#4225),#602,.T.);
#14861=ADVANCED_FACE('',(#4226),#603,.F.);
#14862=ADVANCED_FACE('',(#4227),#604,.T.);
#14863=ADVANCED_FACE('',(#4228),#605,.F.);
#14864=ADVANCED_FACE('',(#4229),#3573,.T.);
#14865=ADVANCED_FACE('',(#4230),#606,.F.);
#14866=ADVANCED_FACE('',(#4231),#3574,.T.);
#14867=ADVANCED_FACE('',(#4232),#607,.T.);
#14868=ADVANCED_FACE('',(#4233),#608,.T.);
#14869=ADVANCED_FACE('',(#4234),#609,.T.);
#14870=ADVANCED_FACE('',(#4235),#610,.F.);
#14871=ADVANCED_FACE('',(#4236),#611,.T.);
#14872=ADVANCED_FACE('',(#4237),#612,.T.);
#14873=ADVANCED_FACE('',(#4238),#613,.T.);
#14874=ADVANCED_FACE('',(#4239),#614,.F.);
#14875=ADVANCED_FACE('',(#4240),#3575,.T.);
#14876=ADVANCED_FACE('',(#4241),#615,.T.);
#14877=ADVANCED_FACE('',(#4242),#616,.F.);
#14878=ADVANCED_FACE('',(#4243),#3576,.T.);
#14879=ADVANCED_FACE('',(#4244),#617,.F.);
#14880=ADVANCED_FACE('',(#4245),#618,.T.);
#14881=ADVANCED_FACE('',(#4246),#3577,.F.);
#14882=ADVANCED_FACE('',(#4247),#3578,.T.);
#14883=ADVANCED_FACE('',(#4248),#3579,.F.);
#14884=ADVANCED_FACE('',(#4249),#3580,.T.);
#14885=ADVANCED_FACE('',(#4250),#619,.T.);
#14886=ADVANCED_FACE('',(#4251),#620,.T.);
#14887=ADVANCED_FACE('',(#4252),#3581,.T.);
#14888=ADVANCED_FACE('',(#4253),#621,.F.);
#14889=ADVANCED_FACE('',(#4254),#622,.F.);
#14890=ADVANCED_FACE('',(#4255,#235),#623,.F.);
#14891=ADVANCED_FACE('',(#4256,#236),#624,.T.);
#14892=ADVANCED_FACE('',(#4257),#625,.F.);
#14893=ADVANCED_FACE('',(#4258),#626,.F.);
#14894=ADVANCED_FACE('',(#4259),#627,.F.);
#14895=ADVANCED_FACE('',(#4260),#628,.F.);
#14896=ADVANCED_FACE('',(#4261),#3582,.T.);
#14897=ADVANCED_FACE('',(#4262),#629,.F.);
#14898=ADVANCED_FACE('',(#4263),#3583,.T.);
#14899=ADVANCED_FACE('',(#4264),#630,.F.);
#14900=ADVANCED_FACE('',(#4265,#237),#631,.T.);
#14901=ADVANCED_FACE('',(#4266),#3584,.T.);
#14902=ADVANCED_FACE('',(#4267,#238),#632,.F.);
#14903=ADVANCED_FACE('',(#4268),#633,.F.);
#14904=ADVANCED_FACE('',(#4269),#634,.F.);
#14905=ADVANCED_FACE('',(#4270,#239),#635,.T.);
#14906=ADVANCED_FACE('',(#4271),#636,.F.);
#14907=ADVANCED_FACE('',(#4272),#3585,.T.);
#14908=ADVANCED_FACE('',(#4273,#240),#1043,.F.);
#14909=ADVANCED_FACE('',(#4274),#3586,.T.);
#14910=ADVANCED_FACE('',(#4275),#3587,.T.);
#14911=ADVANCED_FACE('',(#4276),#3588,.F.);
#14912=ADVANCED_FACE('',(#4277),#3589,.F.);
#14913=ADVANCED_FACE('',(#4278),#3590,.F.);
#14914=ADVANCED_FACE('',(#4279),#3591,.F.);
#14915=ADVANCED_FACE('',(#4280),#3592,.F.);
#14916=ADVANCED_FACE('',(#4281),#3593,.F.);
#14917=ADVANCED_FACE('',(#4282),#3594,.F.);
#14918=ADVANCED_FACE('',(#4283),#3595,.T.);
#14919=ADVANCED_FACE('',(#4284),#1044,.T.);
#14920=ADVANCED_FACE('',(#4285),#3596,.F.);
#14921=ADVANCED_FACE('',(#4286),#3597,.T.);
#14922=ADVANCED_FACE('',(#4287),#3598,.F.);
#14923=ADVANCED_FACE('',(#4288,#241),#637,.F.);
#14924=ADVANCED_FACE('',(#4289,#242),#638,.F.);
#14925=ADVANCED_FACE('',(#4290,#243),#639,.T.);
#14926=ADVANCED_FACE('',(#4291),#640,.F.);
#14927=ADVANCED_FACE('',(#4292),#641,.T.);
#14928=ADVANCED_FACE('',(#4293),#642,.T.);
#14929=ADVANCED_FACE('',(#4294),#643,.T.);
#14930=ADVANCED_FACE('',(#4295),#644,.F.);
#14931=ADVANCED_FACE('',(#4296),#645,.T.);
#14932=ADVANCED_FACE('',(#4297),#3599,.T.);
#14933=ADVANCED_FACE('',(#4298),#646,.T.);
#14934=ADVANCED_FACE('',(#4299),#3600,.T.);
#14935=ADVANCED_FACE('',(#4300),#647,.T.);
#14936=ADVANCED_FACE('',(#4301),#3601,.T.);
#14937=ADVANCED_FACE('',(#4302),#3602,.T.);
#14938=ADVANCED_FACE('',(#4303,#244),#648,.T.);
#14939=ADVANCED_FACE('',(#4304,#245,#246,#247),#649,.F.);
#14940=ADVANCED_FACE('',(#4305),#650,.T.);
#14941=ADVANCED_FACE('',(#4306,#248,#249),#651,.F.);
#14942=ADVANCED_FACE('',(#4307),#652,.F.);
#14943=ADVANCED_FACE('',(#4308),#653,.F.);
#14944=ADVANCED_FACE('',(#4309),#654,.F.);
#14945=ADVANCED_FACE('',(#4310),#655,.F.);
#14946=ADVANCED_FACE('',(#4311,#250,#251,#252),#656,.T.);
#14947=ADVANCED_FACE('',(#4312),#3603,.T.);
#14948=ADVANCED_FACE('',(#4313),#657,.F.);
#14949=ADVANCED_FACE('',(#4314,#253,#254),#658,.T.);
#14950=ADVANCED_FACE('',(#4315),#659,.T.);
#14951=ADVANCED_FACE('',(#4316),#660,.T.);
#14952=ADVANCED_FACE('',(#4317,#255),#661,.F.);
#14953=ADVANCED_FACE('',(#4318),#662,.F.);
#14954=ADVANCED_FACE('',(#4319),#3604,.T.);
#14955=ADVANCED_FACE('',(#4320,#256),#663,.F.);
#14956=ADVANCED_FACE('',(#4321),#664,.F.);
#14957=ADVANCED_FACE('',(#4322,#257),#665,.F.);
#14958=ADVANCED_FACE('',(#4323),#666,.T.);
#14959=ADVANCED_FACE('',(#4324),#667,.T.);
#14960=ADVANCED_FACE('',(#4325),#668,.F.);
#14961=ADVANCED_FACE('',(#4326),#3605,.T.);
#14962=ADVANCED_FACE('',(#4327),#14296,.F.);
#14963=ADVANCED_FACE('',(#4328),#3606,.T.);
#14964=ADVANCED_FACE('',(#4329),#1045,.T.);
#14965=ADVANCED_FACE('',(#4330),#14297,.T.);
#14966=ADVANCED_FACE('',(#4331),#1046,.T.);
#14967=ADVANCED_FACE('',(#4332),#14298,.T.);
#14968=ADVANCED_FACE('',(#4333,#258,#259),#3607,.T.);
#14969=ADVANCED_FACE('',(#4334),#14299,.T.);
#14970=ADVANCED_FACE('',(#4335),#3608,.T.);
#14971=ADVANCED_FACE('',(#4336),#14300,.T.);
#14972=ADVANCED_FACE('',(#4337),#14301,.T.);
#14973=ADVANCED_FACE('',(#4338),#168,.F.);
#14974=ADVANCED_FACE('',(#4339),#14302,.F.);
#14975=ADVANCED_FACE('',(#4340),#3609,.T.);
#14976=ADVANCED_FACE('',(#4341),#3610,.T.);
#14977=ADVANCED_FACE('',(#4342),#14303,.F.);
#14978=ADVANCED_FACE('',(#4343,#260,#261),#3611,.F.);
#14979=ADVANCED_FACE('',(#4344),#169,.F.);
#14980=ADVANCED_FACE('',(#4345),#14304,.T.);
#14981=ADVANCED_FACE('',(#4346),#3612,.F.);
#14982=ADVANCED_FACE('',(#4347),#3613,.T.);
#14983=ADVANCED_FACE('',(#4348),#3614,.T.);
#14984=ADVANCED_FACE('',(#4349),#14305,.F.);
#14985=ADVANCED_FACE('',(#4350),#3615,.T.);
#14986=ADVANCED_FACE('',(#4351),#3616,.T.);
#14987=ADVANCED_FACE('',(#4352),#3617,.T.);
#14988=ADVANCED_FACE('',(#4353),#3618,.F.);
#14989=ADVANCED_FACE('',(#4354),#3619,.F.);
#14990=ADVANCED_FACE('',(#4355),#3620,.F.);
#14991=ADVANCED_FACE('',(#4356),#83,.T.);
#14992=ADVANCED_FACE('',(#4357),#3621,.T.);
#14993=ADVANCED_FACE('',(#4358),#3622,.T.);
#14994=ADVANCED_FACE('',(#4359),#84,.T.);
#14995=ADVANCED_FACE('',(#4360),#3623,.T.);
#14996=ADVANCED_FACE('',(#4361),#85,.T.);
#14997=ADVANCED_FACE('',(#4362),#3624,.F.);
#14998=ADVANCED_FACE('',(#4363),#3625,.T.);
#14999=ADVANCED_FACE('',(#4364),#3626,.T.);
#15000=ADVANCED_FACE('',(#4365),#3627,.F.);
#15001=ADVANCED_FACE('',(#4366),#3628,.F.);
#15002=ADVANCED_FACE('',(#4367),#3629,.T.);
#15003=ADVANCED_FACE('',(#4368),#3630,.F.);
#15004=ADVANCED_FACE('',(#4369),#3631,.F.);
#15005=ADVANCED_FACE('',(#4370),#3632,.F.);
#15006=ADVANCED_FACE('',(#4371),#14306,.T.);
#15007=ADVANCED_FACE('',(#4372),#1047,.F.);
#15008=ADVANCED_FACE('',(#4373),#14307,.F.);
#15009=ADVANCED_FACE('',(#4374),#3633,.F.);
#15010=ADVANCED_FACE('',(#4375),#3634,.F.);
#15011=ADVANCED_FACE('',(#4376),#669,.F.);
#15012=ADVANCED_FACE('',(#4377),#670,.F.);
#15013=ADVANCED_FACE('',(#4378),#671,.F.);
#15014=ADVANCED_FACE('',(#4379),#3635,.F.);
#15015=ADVANCED_FACE('',(#4380),#3636,.F.);
#15016=ADVANCED_FACE('',(#4381),#672,.T.);
#15017=ADVANCED_FACE('',(#4382),#3637,.T.);
#15018=ADVANCED_FACE('',(#4383,#262,#263,#264),#673,.F.);
#15019=ADVANCED_FACE('',(#4384),#674,.T.);
#15020=ADVANCED_FACE('',(#4385),#3638,.T.);
#15021=ADVANCED_FACE('',(#4386),#675,.T.);
#15022=ADVANCED_FACE('',(#4387),#3639,.T.);
#15023=ADVANCED_FACE('',(#4388),#676,.F.);
#15024=ADVANCED_FACE('',(#4389),#170,.F.);
#15025=ADVANCED_FACE('',(#4390),#171,.F.);
#15026=ADVANCED_FACE('',(#4391),#172,.F.);
#15027=ADVANCED_FACE('',(#4392),#173,.F.);
#15028=ADVANCED_FACE('',(#4393),#174,.F.);
#15029=ADVANCED_FACE('',(#4394),#14308,.F.);
#15030=ADVANCED_FACE('',(#4395),#175,.F.);
#15031=ADVANCED_FACE('',(#4396),#86,.T.);
#15032=ADVANCED_FACE('',(#4397),#677,.F.);
#15033=ADVANCED_FACE('',(#4398),#14309,.T.);
#15034=ADVANCED_FACE('',(#4399),#87,.T.);
#15035=ADVANCED_FACE('',(#4400),#3640,.T.);
#15036=ADVANCED_FACE('',(#4401),#3641,.T.);
#15037=ADVANCED_FACE('',(#4402),#88,.T.);
#15038=ADVANCED_FACE('',(#4403),#3642,.T.);
#15039=ADVANCED_FACE('',(#4404),#3643,.T.);
#15040=ADVANCED_FACE('',(#4405),#89,.T.);
#15041=ADVANCED_FACE('',(#4406),#3644,.T.);
#15042=ADVANCED_FACE('',(#4407),#3645,.T.);
#15043=ADVANCED_FACE('',(#4408),#90,.T.);
#15044=ADVANCED_FACE('',(#4409),#3646,.T.);
#15045=ADVANCED_FACE('',(#4410),#3647,.T.);
#15046=ADVANCED_FACE('',(#4411),#91,.T.);
#15047=ADVANCED_FACE('',(#4412),#3648,.T.);
#15048=ADVANCED_FACE('',(#4413),#3649,.T.);
#15049=ADVANCED_FACE('',(#4414),#92,.T.);
#15050=ADVANCED_FACE('',(#4415),#3650,.T.);
#15051=ADVANCED_FACE('',(#4416),#3651,.T.);
#15052=ADVANCED_FACE('',(#4417),#3652,.T.);
#15053=ADVANCED_FACE('',(#4418),#93,.T.);
#15054=ADVANCED_FACE('',(#4419),#3653,.T.);
#15055=ADVANCED_FACE('',(#4420),#3654,.T.);
#15056=ADVANCED_FACE('',(#4421),#94,.T.);
#15057=ADVANCED_FACE('',(#4422),#3655,.T.);
#15058=ADVANCED_FACE('',(#4423),#95,.T.);
#15059=ADVANCED_FACE('',(#4424),#3656,.T.);
#15060=ADVANCED_FACE('',(#4425),#3657,.T.);
#15061=ADVANCED_FACE('',(#4426),#3658,.T.);
#15062=ADVANCED_FACE('',(#4427),#3659,.T.);
#15063=ADVANCED_FACE('',(#4428),#678,.F.);
#15064=ADVANCED_FACE('',(#4429),#679,.T.);
#15065=ADVANCED_FACE('',(#4430),#680,.F.);
#15066=ADVANCED_FACE('',(#4431,#265),#681,.F.);
#15067=ADVANCED_FACE('',(#4432),#682,.T.);
#15068=ADVANCED_FACE('',(#4433),#3660,.T.);
#15069=ADVANCED_FACE('',(#4434,#266),#683,.F.);
#15070=ADVANCED_FACE('',(#4435),#684,.T.);
#15071=ADVANCED_FACE('',(#4436),#3661,.T.);
#15072=ADVANCED_FACE('',(#4437,#267),#685,.F.);
#15073=ADVANCED_FACE('',(#4438),#14310,.T.);
#15074=ADVANCED_FACE('',(#4439),#176,.T.);
#15075=ADVANCED_FACE('',(#4440),#686,.T.);
#15076=ADVANCED_FACE('',(#4441),#14311,.F.);
#15077=ADVANCED_FACE('',(#4442,#268),#687,.T.);
#15078=ADVANCED_FACE('',(#4443,#269,#270),#688,.F.);
#15079=ADVANCED_FACE('',(#4444),#14312,.F.);
#15080=ADVANCED_FACE('',(#4445),#3662,.T.);
#15081=ADVANCED_FACE('',(#4446),#3663,.F.);
#15082=ADVANCED_FACE('',(#4447),#96,.T.);
#15083=ADVANCED_FACE('',(#4448),#689,.T.);
#15084=ADVANCED_FACE('',(#4449),#690,.T.);
#15085=ADVANCED_FACE('',(#4450),#3664,.T.);
#15086=ADVANCED_FACE('',(#4451),#3665,.T.);
#15087=ADVANCED_FACE('',(#4452),#691,.T.);
#15088=ADVANCED_FACE('',(#4453),#177,.T.);
#15089=ADVANCED_FACE('',(#4454),#178,.T.);
#15090=ADVANCED_FACE('',(#4455),#3666,.T.);
#15091=ADVANCED_FACE('',(#4456),#179,.T.);
#15092=ADVANCED_FACE('',(#4457),#3667,.T.);
#15093=ADVANCED_FACE('',(#4458),#3668,.F.);
#15094=ADVANCED_FACE('',(#4459),#180,.F.);
#15095=ADVANCED_FACE('',(#4460),#181,.F.);
#15096=ADVANCED_FACE('',(#4461),#692,.T.);
#15097=ADVANCED_FACE('',(#4462),#693,.T.);
#15098=ADVANCED_FACE('',(#4463),#3669,.T.);
#15099=ADVANCED_FACE('',(#4464),#3670,.F.);
#15100=ADVANCED_FACE('',(#4465),#182,.F.);
#15101=ADVANCED_FACE('',(#4466),#694,.F.);
#15102=ADVANCED_FACE('',(#4467,#271,#272),#695,.T.);
#15103=ADVANCED_FACE('',(#4468),#696,.F.);
#15104=ADVANCED_FACE('',(#4469),#697,.T.);
#15105=ADVANCED_FACE('',(#4470),#698,.F.);
#15106=ADVANCED_FACE('',(#4471),#699,.T.);
#15107=ADVANCED_FACE('',(#4472),#700,.T.);
#15108=ADVANCED_FACE('',(#4473),#701,.F.);
#15109=ADVANCED_FACE('',(#4474),#702,.F.);
#15110=ADVANCED_FACE('',(#4475),#703,.F.);
#15111=ADVANCED_FACE('',(#4476),#704,.T.);
#15112=ADVANCED_FACE('',(#4477),#705,.T.);
#15113=ADVANCED_FACE('',(#4478),#706,.F.);
#15114=ADVANCED_FACE('',(#4479),#183,.F.);
#15115=ADVANCED_FACE('',(#4480),#184,.F.);
#15116=ADVANCED_FACE('',(#4481),#97,.F.);
#15117=ADVANCED_FACE('',(#4482),#3671,.F.);
#15118=ADVANCED_FACE('',(#4483),#14313,.F.);
#15119=ADVANCED_FACE('',(#4484),#3672,.T.);
#15120=ADVANCED_FACE('',(#4485),#3673,.F.);
#15121=ADVANCED_FACE('',(#4486),#185,.F.);
#15122=ADVANCED_FACE('',(#4487),#186,.F.);
#15123=ADVANCED_FACE('',(#4488),#3674,.T.);
#15124=ADVANCED_FACE('',(#4489),#3675,.T.);
#15125=ADVANCED_FACE('',(#4490),#3676,.F.);
#15126=ADVANCED_FACE('',(#4491),#3677,.T.);
#15127=ADVANCED_FACE('',(#4492),#3678,.T.);
#15128=ADVANCED_FACE('',(#4493),#3679,.T.);
#15129=ADVANCED_FACE('',(#4494),#3680,.T.);
#15130=ADVANCED_FACE('',(#4495),#14314,.T.);
#15131=ADVANCED_FACE('',(#4496),#3681,.T.);
#15132=ADVANCED_FACE('',(#4497),#14315,.T.);
#15133=ADVANCED_FACE('',(#4498),#3682,.T.);
#15134=ADVANCED_FACE('',(#4499),#187,.F.);
#15135=ADVANCED_FACE('',(#4500),#188,.F.);
#15136=ADVANCED_FACE('',(#4501,#273),#707,.F.);
#15137=ADVANCED_FACE('',(#4502),#14316,.F.);
#15138=ADVANCED_FACE('',(#4503),#189,.F.);
#15139=ADVANCED_FACE('',(#4504),#190,.F.);
#15140=ADVANCED_FACE('',(#4505),#191,.F.);
#15141=ADVANCED_FACE('',(#4506),#14317,.T.);
#15142=ADVANCED_FACE('',(#4507),#708,.F.);
#15143=ADVANCED_FACE('',(#4508),#709,.F.);
#15144=ADVANCED_FACE('',(#4509),#710,.F.);
#15145=ADVANCED_FACE('',(#4510),#711,.T.);
#15146=ADVANCED_FACE('',(#4511),#712,.F.);
#15147=ADVANCED_FACE('',(#4512),#3683,.F.);
#15148=ADVANCED_FACE('',(#4513,#274),#713,.F.);
#15149=ADVANCED_FACE('',(#4514),#3684,.T.);
#15150=ADVANCED_FACE('',(#4515),#3685,.F.);
#15151=ADVANCED_FACE('',(#4516,#275),#714,.F.);
#15152=ADVANCED_FACE('',(#4517,#276),#715,.T.);
#15153=ADVANCED_FACE('',(#4518),#14318,.T.);
#15154=ADVANCED_FACE('',(#4519),#14319,.T.);
#15155=ADVANCED_FACE('',(#4520),#14320,.T.);
#15156=ADVANCED_FACE('',(#4521),#14321,.T.);
#15157=ADVANCED_FACE('',(#4522),#716,.F.);
#15158=ADVANCED_FACE('',(#4523),#717,.T.);
#15159=ADVANCED_FACE('',(#4524),#3686,.F.);
#15160=ADVANCED_FACE('',(#4525),#3687,.T.);
#15161=ADVANCED_FACE('',(#4526),#718,.F.);
#15162=ADVANCED_FACE('',(#4527),#719,.F.);
#15163=ADVANCED_FACE('',(#4528),#1048,.F.);
#15164=ADVANCED_FACE('',(#4529),#1049,.F.);
#15165=ADVANCED_FACE('',(#4530),#14322,.T.);
#15166=ADVANCED_FACE('',(#4531),#3688,.T.);
#15167=ADVANCED_FACE('',(#4532),#14323,.F.);
#15168=ADVANCED_FACE('',(#4533),#3689,.T.);
#15169=ADVANCED_FACE('',(#4534),#14324,.F.);
#15170=ADVANCED_FACE('',(#4535),#1050,.T.);
#15171=ADVANCED_FACE('',(#4536),#1051,.T.);
#15172=ADVANCED_FACE('',(#4537),#720,.F.);
#15173=ADVANCED_FACE('',(#4538),#1052,.F.);
#15174=ADVANCED_FACE('',(#4539),#1053,.F.);
#15175=ADVANCED_FACE('',(#4540),#1054,.F.);
#15176=ADVANCED_FACE('',(#4541),#721,.F.);
#15177=ADVANCED_FACE('',(#4542),#1055,.F.);
#15178=ADVANCED_FACE('',(#4543),#1056,.F.);
#15179=ADVANCED_FACE('',(#4544),#722,.F.);
#15180=ADVANCED_FACE('',(#4545),#723,.F.);
#15181=ADVANCED_FACE('',(#4546,#277),#724,.F.);
#15182=ADVANCED_FACE('',(#4547),#725,.T.);
#15183=ADVANCED_FACE('',(#4548),#726,.T.);
#15184=ADVANCED_FACE('',(#4549),#727,.T.);
#15185=ADVANCED_FACE('',(#4550),#728,.T.);
#15186=ADVANCED_FACE('',(#4551),#729,.T.);
#15187=ADVANCED_FACE('',(#4552),#730,.T.);
#15188=ADVANCED_FACE('',(#4553),#731,.F.);
#15189=ADVANCED_FACE('',(#4554),#732,.F.);
#15190=ADVANCED_FACE('',(#4555,#278),#733,.F.);
#15191=ADVANCED_FACE('',(#4556),#734,.F.);
#15192=CLOSED_SHELL('',(#14325,#14326,#14327,#14328,#14329,#14330,#14331,
#14332,#14333,#14334,#14335,#14336,#14337,#14338,#14339,#14340,#14341,#14342,
#14343,#14344,#14345,#14346,#14347,#14348,#14349,#14350,#14351,#14352,#14353,
#14354,#14355,#14356,#14357,#14358,#14359,#14360,#14361,#14362,#14363,#14364,
#14365,#14366,#14367,#14368,#14369,#14370,#14371,#14372,#14373,#14374,#14375,
#14376,#14377,#14378,#14379,#14380,#14381,#14382,#14383,#14384,#14385,#14386,
#14387,#14388,#14389,#14390,#14391,#14392,#14393,#14394,#14395,#14396,#14397,
#14398,#14399,#14400,#14401,#14402,#14403,#14404,#14405,#14406,#14407,#14408,
#14409,#14410,#14411));
#15193=CLOSED_SHELL('',(#14412,#14413,#14414,#14415,#14416,#14417,#14418,
#14419,#14420,#14421,#14422,#14423,#14424,#14425,#14426,#14427,#14428,#14429,
#14430,#14431,#14432,#14433,#14434,#14435,#14436,#14437,#14438,#14439,#14440));
#15194=CLOSED_SHELL('',(#14441,#14442,#14443,#14444,#14445,#14446,#14447,
#14448,#14449,#14450,#14451,#14452,#14453,#14454,#14455,#14456,#14457,#14458,
#14459,#14460,#14461,#14462,#14463,#14464,#14465,#14466,#14467,#14468,#14469,
#14470,#14471,#14472,#14473,#14474,#14475,#14476,#14477,#14478,#14479,#14480,
#14481,#14482,#14483,#14484,#14485,#14486,#14487,#14488,#14489,#14490,#14491,
#14492,#14493,#14494,#14495,#14496,#14497,#14498,#14499,#14500,#14501,#14502,
#14503,#14504,#14505,#14506,#14507,#14508,#14509,#14510,#14511,#14512,#14513));
#15195=CLOSED_SHELL('',(#14514,#14515,#14516,#14517,#14518,#14519,#14520,
#14521,#14522,#14523,#14524,#14525,#14526,#14527,#14528,#14529,#14530,#14531,
#14532,#14533,#14534,#14535,#14536,#14537,#14538,#14539,#14540,#14541,#14542,
#14543,#14544,#14545,#14546,#14547,#14548,#14549,#14550,#14551,#14552,#14553,
#14554,#14555,#14556,#14557,#14558,#14559,#14560,#14561,#14562,#14563,#14564,
#14565,#14566,#14567,#14568,#14569,#14570,#14571,#14572,#14573,#14574,#14575,
#14576,#14577,#14578,#14579,#14580,#14581,#14582,#14583,#14584,#14585,#14586,
#14587,#14588,#14589,#14590,#14591,#14592,#14593,#14594,#14595,#14596,#14597,
#14598,#14599,#14600,#14601,#14602,#14603,#14604,#14605,#14606,#14607,#14608,
#14609,#14610,#14611,#14612,#14613,#14614,#14615,#14616,#14617,#14618,#14619,
#14620,#14621,#14622,#14623,#14624,#14625,#14626,#14627,#14628,#14629,#14630,
#14631,#14632,#14633,#14634,#14635,#14636,#14637,#14638));
#15196=CLOSED_SHELL('',(#14639,#14640,#14641,#14642,#14643,#14644,#14645,
#14646,#14647,#14648,#14649,#14650,#14651,#14652,#14653,#14654,#14655,#14656,
#14657,#14658,#14659,#14660,#14661,#14662,#14663,#14664,#14665,#14666,#14667,
#14668,#14669,#14670,#14671,#14672,#14673,#14674,#14675,#14676,#14677,#14678,
#14679,#14680,#14681,#14682,#14683,#14684,#14685,#14686,#14687,#14688,#14689,
#14690,#14691,#14692,#14693,#14694,#14695,#14696,#14697,#14698,#14699,#14700,
#14701,#14702,#14703,#14704,#14705,#14706,#14707,#14708,#14709,#14710,#14711,
#14712,#14713,#14714,#14715,#14716,#14717,#14718,#14719,#14720,#14721,#14722,
#14723,#14724,#14725,#14726,#14727,#14728,#14729,#14730,#14731,#14732,#14733,
#14734,#14735,#14736,#14737,#14738,#14739,#14740,#14741,#14742,#14743,#14744,
#14745,#14746,#14747,#14748,#14749,#14750,#14751,#14752,#14753,#14754,#14755,
#14756,#14757,#14758,#14759,#14760,#14761,#14762,#14763,#14764,#14765,#14766,
#14767,#14768,#14769,#14770,#14771,#14772,#14773,#14774,#14775,#14776,#14777,
#14778,#14779,#14780,#14781,#14782,#14783,#14784,#14785,#14786,#14787,#14788,
#14789,#14790,#14791,#14792,#14793,#14794,#14795,#14796,#14797,#14798,#14799,
#14800,#14801));
#15197=CLOSED_SHELL('',(#14802,#14803,#14804,#14805,#14806,#14807,#14808,
#14809,#14810,#14811,#14812,#14813,#14814,#14815,#14816,#14817,#14818,#14819,
#14820));
#15198=CLOSED_SHELL('',(#14821,#14822,#14823,#14824,#14825,#14826,#14827,
#14828,#14829,#14830,#14831,#14832,#14833,#14834,#14835,#14836,#14837,#14838,
#14839,#14840,#14841,#14842,#14843,#14844,#14845,#14846,#14847,#14848,#14849,
#14850,#14851,#14852,#14853,#14854,#14855,#14856,#14857,#14858,#14859,#14860,
#14861,#14862,#14863,#14864,#14865,#14866,#14867,#14868,#14869,#14870,#14871,
#14872,#14873,#14874,#14875,#14876,#14877,#14878,#14879,#14880,#14881,#14882,
#14883,#14884,#14885,#14886,#14887,#14888,#14889,#14890,#14891,#14892,#14893,
#14894,#14895,#14896,#14897,#14898,#14899,#14900,#14901,#14902,#14903,#14904,
#14905,#14906,#14907));
#15199=CLOSED_SHELL('',(#14908,#14909,#14910,#14911,#14912,#14913,#14914,
#14915,#14916,#14917,#14918,#14919,#14920,#14921,#14922,#14923,#14924,#14925,
#14926,#14927,#14928,#14929,#14930,#14931,#14932,#14933,#14934,#14935,#14936,
#14937,#14938,#14939,#14940,#14941,#14942,#14943,#14944,#14945,#14946,#14947,
#14948,#14949,#14950,#14951,#14952,#14953,#14954,#14955,#14956,#14957,#14958,
#14959,#14960,#14961));
#15200=CLOSED_SHELL('',(#14962,#14963,#14964,#14965,#14966,#14967,#14968,
#14969,#14970,#14971,#14972,#14973,#14974,#14975,#14976,#14977,#14978,#14979,
#14980,#14981,#14982,#14983,#14984,#14985,#14986,#14987,#14988,#14989,#14990,
#14991,#14992,#14993,#14994,#14995,#14996,#14997,#14998,#14999,#15000,#15001,
#15002,#15003,#15004,#15005,#15006,#15007,#15008,#15009,#15010,#15011,#15012,
#15013,#15014,#15015,#15016,#15017,#15018,#15019,#15020,#15021,#15022,#15023,
#15024,#15025,#15026,#15027,#15028,#15029,#15030,#15031,#15032,#15033,#15034,
#15035,#15036,#15037,#15038,#15039,#15040,#15041,#15042,#15043,#15044,#15045,
#15046,#15047,#15048,#15049,#15050,#15051,#15052,#15053,#15054,#15055,#15056,
#15057,#15058,#15059,#15060,#15061,#15062,#15063,#15064,#15065,#15066,#15067,
#15068,#15069,#15070,#15071,#15072,#15073,#15074,#15075,#15076,#15077,#15078,
#15079,#15080,#15081,#15082,#15083,#15084,#15085,#15086,#15087,#15088,#15089,
#15090,#15091,#15092,#15093,#15094,#15095,#15096,#15097,#15098,#15099,#15100,
#15101,#15102,#15103,#15104,#15105,#15106,#15107,#15108,#15109,#15110,#15111,
#15112,#15113,#15114,#15115,#15116,#15117,#15118,#15119,#15120,#15121,#15122,
#15123,#15124,#15125,#15126,#15127,#15128,#15129,#15130,#15131,#15132,#15133,
#15134,#15135,#15136,#15137,#15138,#15139,#15140,#15141,#15142,#15143,#15144,
#15145,#15146,#15147,#15148));
#15201=CLOSED_SHELL('',(#15149,#15150,#15151,#15152));
#15202=CLOSED_SHELL('',(#15153,#15154,#15155,#15156,#15157,#15158,#15159,
#15160,#15161,#15162));
#15203=CLOSED_SHELL('',(#15163,#15164,#15165,#15166,#15167,#15168,#15169,
#15170,#15171,#15172,#15173,#15174,#15175,#15176,#15177,#15178,#15179,#15180,
#15181,#15182,#15183,#15184,#15185,#15186,#15187,#15188,#15189,#15190,#15191));
#15204=DERIVED_UNIT_ELEMENT(#15228,1.);
#15205=DERIVED_UNIT_ELEMENT(#62976,-3.);
#15206=DERIVED_UNIT_ELEMENT(#15228,1.);
#15207=DERIVED_UNIT_ELEMENT(#62976,-3.);
#15208=DERIVED_UNIT_ELEMENT(#15228,1.);
#15209=DERIVED_UNIT_ELEMENT(#62976,-3.);
#15210=DERIVED_UNIT_ELEMENT(#15228,1.);
#15211=DERIVED_UNIT_ELEMENT(#62976,-3.);
#15212=DERIVED_UNIT_ELEMENT(#15228,1.);
#15213=DERIVED_UNIT_ELEMENT(#62976,-3.);
#15214=DERIVED_UNIT_ELEMENT(#15228,1.);
#15215=DERIVED_UNIT_ELEMENT(#62976,-3.);
#15216=DERIVED_UNIT_ELEMENT(#15228,1.);
#15217=DERIVED_UNIT_ELEMENT(#62976,-3.);
#15218=DERIVED_UNIT_ELEMENT(#15228,1.);
#15219=DERIVED_UNIT_ELEMENT(#62976,-3.);
#15220=DERIVED_UNIT_ELEMENT(#15228,1.);
#15221=DERIVED_UNIT_ELEMENT(#62976,-3.);
#15222=DERIVED_UNIT_ELEMENT(#15228,1.);
#15223=DERIVED_UNIT_ELEMENT(#62976,-3.);
#15224=DERIVED_UNIT_ELEMENT(#15228,1.);
#15225=DERIVED_UNIT_ELEMENT(#62976,-3.);
#15226=DERIVED_UNIT_ELEMENT(#15228,1.);
#15227=DERIVED_UNIT_ELEMENT(#62976,-3.);
#15228=(
MASS_UNIT()
NAMED_UNIT(*)
SI_UNIT(.KILO.,.GRAM.)
);
#15229=DERIVED_UNIT((#15204,#15205));
#15230=DERIVED_UNIT((#15206,#15207));
#15231=DERIVED_UNIT((#15208,#15209));
#15232=DERIVED_UNIT((#15210,#15211));
#15233=DERIVED_UNIT((#15212,#15213));
#15234=DERIVED_UNIT((#15214,#15215));
#15235=DERIVED_UNIT((#15216,#15217));
#15236=DERIVED_UNIT((#15218,#15219));
#15237=DERIVED_UNIT((#15220,#15221));
#15238=DERIVED_UNIT((#15222,#15223));
#15239=DERIVED_UNIT((#15224,#15225));
#15240=DERIVED_UNIT((#15226,#15227));
#15241=MEASURE_REPRESENTATION_ITEM('density measure',
POSITIVE_RATIO_MEASURE(7850.),#15229);
#15242=MEASURE_REPRESENTATION_ITEM('density measure',
POSITIVE_RATIO_MEASURE(7850.),#15230);
#15243=MEASURE_REPRESENTATION_ITEM('density measure',
POSITIVE_RATIO_MEASURE(7850.),#15231);
#15244=MEASURE_REPRESENTATION_ITEM('density measure',
POSITIVE_RATIO_MEASURE(7850.),#15232);
#15245=MEASURE_REPRESENTATION_ITEM('density measure',
POSITIVE_RATIO_MEASURE(7850.),#15233);
#15246=MEASURE_REPRESENTATION_ITEM('density measure',
POSITIVE_RATIO_MEASURE(7850.),#15234);
#15247=MEASURE_REPRESENTATION_ITEM('density measure',
POSITIVE_RATIO_MEASURE(7850.),#15235);
#15248=MEASURE_REPRESENTATION_ITEM('density measure',
POSITIVE_RATIO_MEASURE(7850.),#15236);
#15249=MEASURE_REPRESENTATION_ITEM('density measure',
POSITIVE_RATIO_MEASURE(7850.),#15237);
#15250=MEASURE_REPRESENTATION_ITEM('density measure',
POSITIVE_RATIO_MEASURE(7850.),#15238);
#15251=MEASURE_REPRESENTATION_ITEM('density measure',
POSITIVE_RATIO_MEASURE(7850.),#15239);
#15252=MEASURE_REPRESENTATION_ITEM('density measure',
POSITIVE_RATIO_MEASURE(7850.),#15240);
#15253=PROPERTY_DEFINITION_REPRESENTATION(#15313,#15277);
#15254=PROPERTY_DEFINITION_REPRESENTATION(#15314,#15278);
#15255=PROPERTY_DEFINITION_REPRESENTATION(#15315,#15279);
#15256=PROPERTY_DEFINITION_REPRESENTATION(#15316,#15280);
#15257=PROPERTY_DEFINITION_REPRESENTATION(#15317,#15281);
#15258=PROPERTY_DEFINITION_REPRESENTATION(#15318,#15282);
#15259=PROPERTY_DEFINITION_REPRESENTATION(#15319,#15283);
#15260=PROPERTY_DEFINITION_REPRESENTATION(#15320,#15284);
#15261=PROPERTY_DEFINITION_REPRESENTATION(#15321,#15285);
#15262=PROPERTY_DEFINITION_REPRESENTATION(#15322,#15286);
#15263=PROPERTY_DEFINITION_REPRESENTATION(#15323,#15287);
#15264=PROPERTY_DEFINITION_REPRESENTATION(#15324,#15288);
#15265=PROPERTY_DEFINITION_REPRESENTATION(#15325,#15289);
#15266=PROPERTY_DEFINITION_REPRESENTATION(#15326,#15290);
#15267=PROPERTY_DEFINITION_REPRESENTATION(#15327,#15291);
#15268=PROPERTY_DEFINITION_REPRESENTATION(#15328,#15292);
#15269=PROPERTY_DEFINITION_REPRESENTATION(#15329,#15293);
#15270=PROPERTY_DEFINITION_REPRESENTATION(#15330,#15294);
#15271=PROPERTY_DEFINITION_REPRESENTATION(#15331,#15295);
#15272=PROPERTY_DEFINITION_REPRESENTATION(#15332,#15296);
#15273=PROPERTY_DEFINITION_REPRESENTATION(#15333,#15297);
#15274=PROPERTY_DEFINITION_REPRESENTATION(#15334,#15298);
#15275=PROPERTY_DEFINITION_REPRESENTATION(#15335,#15299);
#15276=PROPERTY_DEFINITION_REPRESENTATION(#15336,#15300);
#15277=REPRESENTATION('material name',(#15301),#62962);
#15278=REPRESENTATION('density',(#15241),#62962);
#15279=REPRESENTATION('material name',(#15302),#62963);
#15280=REPRESENTATION('density',(#15242),#62963);
#15281=REPRESENTATION('material name',(#15303),#62964);
#15282=REPRESENTATION('density',(#15243),#62964);
#15283=REPRESENTATION('material name',(#15304),#62965);
#15284=REPRESENTATION('density',(#15244),#62965);
#15285=REPRESENTATION('material name',(#15305),#62966);
#15286=REPRESENTATION('density',(#15245),#62966);
#15287=REPRESENTATION('material name',(#15306),#62967);
#15288=REPRESENTATION('density',(#15246),#62967);
#15289=REPRESENTATION('material name',(#15307),#62968);
#15290=REPRESENTATION('density',(#15247),#62968);
#15291=REPRESENTATION('material name',(#15308),#62969);
#15292=REPRESENTATION('density',(#15248),#62969);
#15293=REPRESENTATION('material name',(#15309),#62970);
#15294=REPRESENTATION('density',(#15249),#62970);
#15295=REPRESENTATION('material name',(#15310),#62971);
#15296=REPRESENTATION('density',(#15250),#62971);
#15297=REPRESENTATION('material name',(#15311),#62972);
#15298=REPRESENTATION('density',(#15251),#62972);
#15299=REPRESENTATION('material name',(#15312),#62973);
#15300=REPRESENTATION('density',(#15252),#62973);
#15301=DESCRIPTIVE_REPRESENTATION_ITEM('Steel','Steel');
#15302=DESCRIPTIVE_REPRESENTATION_ITEM('Steel','Steel');
#15303=DESCRIPTIVE_REPRESENTATION_ITEM('Steel','Steel');
#15304=DESCRIPTIVE_REPRESENTATION_ITEM('Steel','Steel');
#15305=DESCRIPTIVE_REPRESENTATION_ITEM('Steel','Steel');
#15306=DESCRIPTIVE_REPRESENTATION_ITEM('Steel','Steel');
#15307=DESCRIPTIVE_REPRESENTATION_ITEM('Steel','Steel');
#15308=DESCRIPTIVE_REPRESENTATION_ITEM('Steel','Steel');
#15309=DESCRIPTIVE_REPRESENTATION_ITEM('Steel','Steel');
#15310=DESCRIPTIVE_REPRESENTATION_ITEM('Steel','Steel');
#15311=DESCRIPTIVE_REPRESENTATION_ITEM('Steel','Steel');
#15312=DESCRIPTIVE_REPRESENTATION_ITEM('Steel','Steel');
#15313=PROPERTY_DEFINITION('material property','material name',#63035);
#15314=PROPERTY_DEFINITION('material property','density of part',#63035);
#15315=PROPERTY_DEFINITION('material property','material name',#63036);
#15316=PROPERTY_DEFINITION('material property','density of part',#63036);
#15317=PROPERTY_DEFINITION('material property','material name',#63037);
#15318=PROPERTY_DEFINITION('material property','density of part',#63037);
#15319=PROPERTY_DEFINITION('material property','material name',#63038);
#15320=PROPERTY_DEFINITION('material property','density of part',#63038);
#15321=PROPERTY_DEFINITION('material property','material name',#63039);
#15322=PROPERTY_DEFINITION('material property','density of part',#63039);
#15323=PROPERTY_DEFINITION('material property','material name',#63040);
#15324=PROPERTY_DEFINITION('material property','density of part',#63040);
#15325=PROPERTY_DEFINITION('material property','material name',#63041);
#15326=PROPERTY_DEFINITION('material property','density of part',#63041);
#15327=PROPERTY_DEFINITION('material property','material name',#63042);
#15328=PROPERTY_DEFINITION('material property','density of part',#63042);
#15329=PROPERTY_DEFINITION('material property','material name',#63043);
#15330=PROPERTY_DEFINITION('material property','density of part',#63043);
#15331=PROPERTY_DEFINITION('material property','material name',#63044);
#15332=PROPERTY_DEFINITION('material property','density of part',#63044);
#15333=PROPERTY_DEFINITION('material property','material name',#63045);
#15334=PROPERTY_DEFINITION('material property','density of part',#63045);
#15335=PROPERTY_DEFINITION('material property','material name',#63046);
#15336=PROPERTY_DEFINITION('material property','density of part',#63046);
#15337=AXIS2_PLACEMENT_3D('',#21387,#16956,#16957);
#15338=AXIS2_PLACEMENT_3D('',#21388,#16958,#16959);
#15339=AXIS2_PLACEMENT_3D('',#21389,#16960,#16961);
#15340=AXIS2_PLACEMENT_3D('',#21391,#16962,#16963);
#15341=AXIS2_PLACEMENT_3D('',#21393,#16964,#16965);
#15342=AXIS2_PLACEMENT_3D('',#21394,#16966,#16967);
#15343=AXIS2_PLACEMENT_3D('',#21395,#16968,#16969);
#15344=AXIS2_PLACEMENT_3D('',#21398,#16971,#16972);
#15345=AXIS2_PLACEMENT_3D('',#21399,#16973,#16974);
#15346=AXIS2_PLACEMENT_3D('',#21401,#16975,#16976);
#15347=AXIS2_PLACEMENT_3D('',#21403,#16978,#16979);
#15348=AXIS2_PLACEMENT_3D('',#21405,#16980,#16981);
#15349=AXIS2_PLACEMENT_3D('',#21408,#16983,#16984);
#15350=AXIS2_PLACEMENT_3D('',#21409,#16985,#16986);
#15351=AXIS2_PLACEMENT_3D('',#21411,#16987,#16988);
#15352=AXIS2_PLACEMENT_3D('',#21414,#16990,#16991);
#15353=AXIS2_PLACEMENT_3D('',#21415,#16992,#16993);
#15354=AXIS2_PLACEMENT_3D('',#21417,#16994,#16995);
#15355=AXIS2_PLACEMENT_3D('',#21421,#16997,#16998);
#15356=AXIS2_PLACEMENT_3D('',#21445,#16999,#17000);
#15357=AXIS2_PLACEMENT_3D('',#21446,#17001,#17002);
#15358=AXIS2_PLACEMENT_3D('',#21449,#17003,#17004);
#15359=AXIS2_PLACEMENT_3D('',#21453,#17006,#17007);
#15360=AXIS2_PLACEMENT_3D('',#21455,#17009,#17010);
#15361=AXIS2_PLACEMENT_3D('',#21457,#17011,#17012);
#15362=AXIS2_PLACEMENT_3D('',#21459,#17013,#17014);
#15363=AXIS2_PLACEMENT_3D('',#21461,#17015,#17016);
#15364=AXIS2_PLACEMENT_3D('',#21463,#17017,#17018);
#15365=AXIS2_PLACEMENT_3D('',#21464,#17019,#17020);
#15366=AXIS2_PLACEMENT_3D('',#21465,#17021,#17022);
#15367=AXIS2_PLACEMENT_3D('',#21467,#17023,#17024);
#15368=AXIS2_PLACEMENT_3D('',#21470,#17026,#17027);
#15369=AXIS2_PLACEMENT_3D('',#21471,#17028,#17029);
#15370=AXIS2_PLACEMENT_3D('',#21473,#17030,#17031);
#15371=AXIS2_PLACEMENT_3D('',#21476,#17033,#17034);
#15372=AXIS2_PLACEMENT_3D('',#21477,#17035,#17036);
#15373=AXIS2_PLACEMENT_3D('',#21478,#17037,#17038);
#15374=AXIS2_PLACEMENT_3D('',#21480,#17039,#17040);
#15375=AXIS2_PLACEMENT_3D('',#21483,#17042,#17043);
#15376=AXIS2_PLACEMENT_3D('',#21484,#17044,#17045);
#15377=AXIS2_PLACEMENT_3D('',#21487,#17047,#17048);
#15378=AXIS2_PLACEMENT_3D('',#21488,#17049,#17050);
#15379=AXIS2_PLACEMENT_3D('',#21490,#17051,#17052);
#15380=AXIS2_PLACEMENT_3D('',#21493,#17054,#17055);
#15381=AXIS2_PLACEMENT_3D('',#21494,#17056,#17057);
#15382=AXIS2_PLACEMENT_3D('',#21496,#17058,#17059);
#15383=AXIS2_PLACEMENT_3D('',#21499,#17061,#17062);
#15384=AXIS2_PLACEMENT_3D('',#21500,#17063,#17064);
#15385=AXIS2_PLACEMENT_3D('',#21502,#17065,#17066);
#15386=AXIS2_PLACEMENT_3D('',#21505,#17068,#17069);
#15387=AXIS2_PLACEMENT_3D('',#21506,#17070,#17071);
#15388=AXIS2_PLACEMENT_3D('',#21508,#17072,#17073);
#15389=AXIS2_PLACEMENT_3D('',#21510,#17074,#17075);
#15390=AXIS2_PLACEMENT_3D('',#21511,#17076,#17077);
#15391=AXIS2_PLACEMENT_3D('',#21512,#17078,#17079);
#15392=AXIS2_PLACEMENT_3D('',#21514,#17080,#17081);
#15393=AXIS2_PLACEMENT_3D('',#21517,#17083,#17084);
#15394=AXIS2_PLACEMENT_3D('',#21518,#17085,#17086);
#15395=AXIS2_PLACEMENT_3D('',#21520,#17087,#17088);
#15396=AXIS2_PLACEMENT_3D('',#21522,#17090,#17091);
#15397=AXIS2_PLACEMENT_3D('',#21524,#17092,#17093);
#15398=AXIS2_PLACEMENT_3D('',#21527,#17095,#17096);
#15399=AXIS2_PLACEMENT_3D('',#21528,#17097,#17098);
#15400=AXIS2_PLACEMENT_3D('',#21529,#17099,#17100);
#15401=AXIS2_PLACEMENT_3D('',#21530,#17101,#17102);
#15402=AXIS2_PLACEMENT_3D('',#21531,#17103,#17104);
#15403=AXIS2_PLACEMENT_3D('',#21532,#17105,#17106);
#15404=AXIS2_PLACEMENT_3D('',#21533,#17107,#17108);
#15405=AXIS2_PLACEMENT_3D('',#21542,#17113,#17114);
#15406=AXIS2_PLACEMENT_3D('',#21548,#17118,#17119);
#15407=AXIS2_PLACEMENT_3D('',#21552,#17122,#17123);
#15408=AXIS2_PLACEMENT_3D('',#21556,#17126,#17127);
#15409=AXIS2_PLACEMENT_3D('',#21565,#17132,#17133);
#15410=AXIS2_PLACEMENT_3D('',#21573,#17138,#17139);
#15411=AXIS2_PLACEMENT_3D('',#21577,#17142,#17143);
#15412=AXIS2_PLACEMENT_3D('',#21586,#17148,#17149);
#15413=AXIS2_PLACEMENT_3D('',#21592,#17153,#17154);
#15414=AXIS2_PLACEMENT_3D('',#21598,#17158,#17159);
#15415=AXIS2_PLACEMENT_3D('',#21604,#17163,#17164);
#15416=AXIS2_PLACEMENT_3D('',#21608,#17167,#17168);
#15417=AXIS2_PLACEMENT_3D('',#21611,#17171,#17172);
#15418=AXIS2_PLACEMENT_3D('',#21618,#17177,#17178);
#15419=AXIS2_PLACEMENT_3D('',#21620,#17180,#17181);
#15420=AXIS2_PLACEMENT_3D('',#21626,#17185,#17186);
#15421=AXIS2_PLACEMENT_3D('',#21630,#17189,#17190);
#15422=AXIS2_PLACEMENT_3D('',#21634,#17193,#17194);
#15423=AXIS2_PLACEMENT_3D('',#21636,#17196,#17197);
#15424=AXIS2_PLACEMENT_3D('',#21637,#17198,#17199);
#15425=AXIS2_PLACEMENT_3D('',#21646,#17204,#17205);
#15426=AXIS2_PLACEMENT_3D('',#21655,#17210,#17211);
#15427=AXIS2_PLACEMENT_3D('',#21665,#17217,#17218);
#15428=AXIS2_PLACEMENT_3D('',#21667,#17220,#17221);
#15429=AXIS2_PLACEMENT_3D('',#21673,#17225,#17226);
#15430=AXIS2_PLACEMENT_3D('',#21679,#17230,#17231);
#15431=AXIS2_PLACEMENT_3D('',#21684,#17235,#17236);
#15432=AXIS2_PLACEMENT_3D('',#21689,#17240,#17241);
#15433=AXIS2_PLACEMENT_3D('',#21693,#17244,#17245);
#15434=AXIS2_PLACEMENT_3D('',#21696,#17248,#17249);
#15435=AXIS2_PLACEMENT_3D('',#21698,#17251,#17252);
#15436=AXIS2_PLACEMENT_3D('',#21704,#17256,#17257);
#15437=AXIS2_PLACEMENT_3D('',#21707,#17260,#17261);
#15438=AXIS2_PLACEMENT_3D('',#21710,#17264,#17265);
#15439=AXIS2_PLACEMENT_3D('',#21712,#17267,#17268);
#15440=AXIS2_PLACEMENT_3D('',#21714,#17270,#17271);
#15441=AXIS2_PLACEMENT_3D('',#21715,#17272,#17273);
#15442=AXIS2_PLACEMENT_3D('',#27767,#17274,#17275);
#15443=AXIS2_PLACEMENT_3D('',#27790,#17276,#17277);
#15444=AXIS2_PLACEMENT_3D('',#27791,#17278,#17279);
#15445=AXIS2_PLACEMENT_3D('',#33842,#17280,#17281);
#15446=AXIS2_PLACEMENT_3D('',#33845,#17282,#17283);
#15447=AXIS2_PLACEMENT_3D('',#33849,#17285,#17286);
#15448=AXIS2_PLACEMENT_3D('',#33851,#17288,#17289);
#15449=AXIS2_PLACEMENT_3D('',#33857,#17293,#17294);
#15450=AXIS2_PLACEMENT_3D('',#33859,#17295,#17296);
#15451=AXIS2_PLACEMENT_3D('',#33861,#17297,#17298);
#15452=AXIS2_PLACEMENT_3D('',#33863,#17300,#17301);
#15453=AXIS2_PLACEMENT_3D('',#33864,#17302,#17303);
#15454=AXIS2_PLACEMENT_3D('',#33873,#17308,#17309);
#15455=AXIS2_PLACEMENT_3D('',#33876,#17312,#17313);
#15456=AXIS2_PLACEMENT_3D('',#33879,#17316,#17317);
#15457=AXIS2_PLACEMENT_3D('',#33880,#17318,#17319);
#15458=AXIS2_PLACEMENT_3D('',#33883,#17322,#17323);
#15459=AXIS2_PLACEMENT_3D('',#33884,#17324,#17325);
#15460=AXIS2_PLACEMENT_3D('',#33885,#17326,#17327);
#15461=AXIS2_PLACEMENT_3D('',#33886,#17328,#17329);
#15462=AXIS2_PLACEMENT_3D('',#33887,#17330,#17331);
#15463=AXIS2_PLACEMENT_3D('',#33888,#17332,#17333);
#15464=AXIS2_PLACEMENT_3D('',#33897,#17338,#17339);
#15465=AXIS2_PLACEMENT_3D('',#33903,#17343,#17344);
#15466=AXIS2_PLACEMENT_3D('',#33907,#17347,#17348);
#15467=AXIS2_PLACEMENT_3D('',#33908,#17349,#17350);
#15468=AXIS2_PLACEMENT_3D('',#33912,#17353,#17354);
#15469=AXIS2_PLACEMENT_3D('',#33914,#17356,#17357);
#15470=AXIS2_PLACEMENT_3D('',#33915,#17358,#17359);
#15471=AXIS2_PLACEMENT_3D('',#33916,#17360,#17361);
#15472=AXIS2_PLACEMENT_3D('',#33917,#17362,#17363);
#15473=AXIS2_PLACEMENT_3D('',#33919,#17364,#17365);
#15474=AXIS2_PLACEMENT_3D('',#33922,#17367,#17368);
#15475=AXIS2_PLACEMENT_3D('',#33923,#17369,#17370);
#15476=AXIS2_PLACEMENT_3D('',#33926,#17371,#17372);
#15477=AXIS2_PLACEMENT_3D('',#33928,#17373,#17374);
#15478=AXIS2_PLACEMENT_3D('',#33930,#17375,#17376);
#15479=AXIS2_PLACEMENT_3D('',#33932,#17377,#17378);
#15480=AXIS2_PLACEMENT_3D('',#33934,#17379,#17380);
#15481=AXIS2_PLACEMENT_3D('',#33936,#17381,#17382);
#15482=AXIS2_PLACEMENT_3D('',#33938,#17383,#17384);
#15483=AXIS2_PLACEMENT_3D('',#33940,#17385,#17386);
#15484=AXIS2_PLACEMENT_3D('',#33942,#17387,#17388);
#15485=AXIS2_PLACEMENT_3D('',#33944,#17389,#17390);
#15486=AXIS2_PLACEMENT_3D('',#33946,#17391,#17392);
#15487=AXIS2_PLACEMENT_3D('',#33948,#17393,#17394);
#15488=AXIS2_PLACEMENT_3D('',#33950,#17395,#17396);
#15489=AXIS2_PLACEMENT_3D('',#33952,#17397,#17398);
#15490=AXIS2_PLACEMENT_3D('',#33954,#17399,#17400);
#15491=AXIS2_PLACEMENT_3D('',#33956,#17401,#17402);
#15492=AXIS2_PLACEMENT_3D('',#33958,#17403,#17404);
#15493=AXIS2_PLACEMENT_3D('',#33960,#17405,#17406);
#15494=AXIS2_PLACEMENT_3D('',#33962,#17407,#17408);
#15495=AXIS2_PLACEMENT_3D('',#33963,#17409,#17410);
#15496=AXIS2_PLACEMENT_3D('',#33964,#17411,#17412);
#15497=AXIS2_PLACEMENT_3D('',#33966,#17413,#17414);
#15498=AXIS2_PLACEMENT_3D('',#33968,#17415,#17416);
#15499=AXIS2_PLACEMENT_3D('',#33969,#17417,#17418);
#15500=AXIS2_PLACEMENT_3D('',#33970,#17419,#17420);
#15501=AXIS2_PLACEMENT_3D('',#33974,#17422,#17423);
#15502=AXIS2_PLACEMENT_3D('',#33975,#17424,#17425);
#15503=AXIS2_PLACEMENT_3D('',#33976,#17426,#17427);
#15504=AXIS2_PLACEMENT_3D('',#33979,#17428,#17429);
#15505=AXIS2_PLACEMENT_3D('',#33981,#17431,#17432);
#15506=AXIS2_PLACEMENT_3D('',#33982,#17433,#17434);
#15507=AXIS2_PLACEMENT_3D('',#33984,#17435,#17436);
#15508=AXIS2_PLACEMENT_3D('',#33986,#17438,#17439);
#15509=AXIS2_PLACEMENT_3D('',#33987,#17440,#17441);
#15510=AXIS2_PLACEMENT_3D('',#33988,#17442,#17443);
#15511=AXIS2_PLACEMENT_3D('',#33994,#17447,#17448);
#15512=AXIS2_PLACEMENT_3D('',#34000,#17452,#17453);
#15513=AXIS2_PLACEMENT_3D('',#34004,#17456,#17457);
#15514=AXIS2_PLACEMENT_3D('',#34008,#17460,#17461);
#15515=AXIS2_PLACEMENT_3D('',#34012,#17464,#17465);
#15516=AXIS2_PLACEMENT_3D('',#34016,#17468,#17469);
#15517=AXIS2_PLACEMENT_3D('',#34020,#17472,#17473);
#15518=AXIS2_PLACEMENT_3D('',#34024,#17476,#17477);
#15519=AXIS2_PLACEMENT_3D('',#34028,#17480,#17481);
#15520=AXIS2_PLACEMENT_3D('',#34032,#17484,#17485);
#15521=AXIS2_PLACEMENT_3D('',#34036,#17488,#17489);
#15522=AXIS2_PLACEMENT_3D('',#34040,#17492,#17493);
#15523=AXIS2_PLACEMENT_3D('',#34044,#17496,#17497);
#15524=AXIS2_PLACEMENT_3D('',#34048,#17500,#17501);
#15525=AXIS2_PLACEMENT_3D('',#34052,#17504,#17505);
#15526=AXIS2_PLACEMENT_3D('',#34056,#17508,#17509);
#15527=AXIS2_PLACEMENT_3D('',#34060,#17512,#17513);
#15528=AXIS2_PLACEMENT_3D('',#34062,#17515,#17516);
#15529=AXIS2_PLACEMENT_3D('',#34066,#17519,#17520);
#15530=AXIS2_PLACEMENT_3D('',#34068,#17522,#17523);
#15531=AXIS2_PLACEMENT_3D('',#34069,#17524,#17525);
#15532=AXIS2_PLACEMENT_3D('',#34080,#17526,#17527);
#15533=AXIS2_PLACEMENT_3D('',#34084,#17529,#17530);
#15534=AXIS2_PLACEMENT_3D('',#34086,#17531,#17532);
#15535=AXIS2_PLACEMENT_3D('',#34088,#17533,#17534);
#15536=AXIS2_PLACEMENT_3D('',#34092,#17536,#17537);
#15537=AXIS2_PLACEMENT_3D('',#34093,#17538,#17539);
#15538=AXIS2_PLACEMENT_3D('',#34094,#17540,#17541);
#15539=AXIS2_PLACEMENT_3D('',#34097,#17542,#17543);
#15540=AXIS2_PLACEMENT_3D('',#34099,#17544,#17545);
#15541=AXIS2_PLACEMENT_3D('',#34101,#17546,#17547);
#15542=AXIS2_PLACEMENT_3D('',#34104,#17549,#17550);
#15543=AXIS2_PLACEMENT_3D('',#34106,#17551,#17552);
#15544=AXIS2_PLACEMENT_3D('',#34107,#17553,#17554);
#15545=AXIS2_PLACEMENT_3D('',#34108,#17555,#17556);
#15546=AXIS2_PLACEMENT_3D('',#34111,#17557,#17558);
#15547=AXIS2_PLACEMENT_3D('',#34113,#17559,#17560);
#15548=AXIS2_PLACEMENT_3D('',#34115,#17561,#17562);
#15549=AXIS2_PLACEMENT_3D('',#34117,#17563,#17564);
#15550=AXIS2_PLACEMENT_3D('',#34119,#17565,#17566);
#15551=AXIS2_PLACEMENT_3D('',#34121,#17567,#17568);
#15552=AXIS2_PLACEMENT_3D('',#34123,#17569,#17570);
#15553=AXIS2_PLACEMENT_3D('',#34125,#17571,#17572);
#15554=AXIS2_PLACEMENT_3D('',#34127,#17573,#17574);
#15555=AXIS2_PLACEMENT_3D('',#34129,#17575,#17576);
#15556=AXIS2_PLACEMENT_3D('',#34131,#17577,#17578);
#15557=AXIS2_PLACEMENT_3D('',#34133,#17579,#17580);
#15558=AXIS2_PLACEMENT_3D('',#34135,#17581,#17582);
#15559=AXIS2_PLACEMENT_3D('',#34137,#17583,#17584);
#15560=AXIS2_PLACEMENT_3D('',#34139,#17585,#17586);
#15561=AXIS2_PLACEMENT_3D('',#34141,#17587,#17588);
#15562=AXIS2_PLACEMENT_3D('',#34143,#17589,#17590);
#15563=AXIS2_PLACEMENT_3D('',#34145,#17591,#17592);
#15564=AXIS2_PLACEMENT_3D('',#34147,#17593,#17594);
#15565=AXIS2_PLACEMENT_3D('',#34148,#17595,#17596);
#15566=AXIS2_PLACEMENT_3D('',#34149,#17597,#17598);
#15567=AXIS2_PLACEMENT_3D('',#34151,#17599,#17600);
#15568=AXIS2_PLACEMENT_3D('',#34155,#17602,#17603);
#15569=AXIS2_PLACEMENT_3D('',#34162,#17607,#17608);
#15570=AXIS2_PLACEMENT_3D('',#34165,#17610,#17611);
#15571=AXIS2_PLACEMENT_3D('',#34167,#17612,#17613);
#15572=AXIS2_PLACEMENT_3D('',#34173,#17617,#17618);
#15573=AXIS2_PLACEMENT_3D('',#34176,#17619,#17620);
#15574=AXIS2_PLACEMENT_3D('',#34183,#17624,#17625);
#15575=AXIS2_PLACEMENT_3D('',#34190,#17629,#17630);
#15576=AXIS2_PLACEMENT_3D('',#34194,#17632,#17633);
#15577=AXIS2_PLACEMENT_3D('',#34198,#17635,#17636);
#15578=AXIS2_PLACEMENT_3D('',#34208,#17642,#17643);
#15579=AXIS2_PLACEMENT_3D('',#34216,#17649,#17650);
#15580=AXIS2_PLACEMENT_3D('',#34218,#17651,#17652);
#15581=AXIS2_PLACEMENT_3D('',#34221,#17653,#17654);
#15582=AXIS2_PLACEMENT_3D('',#34223,#17655,#17656);
#15583=AXIS2_PLACEMENT_3D('',#34225,#17657,#17658);
#15584=AXIS2_PLACEMENT_3D('',#34227,#17659,#17660);
#15585=AXIS2_PLACEMENT_3D('',#34229,#17661,#17662);
#15586=AXIS2_PLACEMENT_3D('',#34231,#17663,#17664);
#15587=AXIS2_PLACEMENT_3D('',#34233,#17665,#17666);
#15588=AXIS2_PLACEMENT_3D('',#34235,#17667,#17668);
#15589=AXIS2_PLACEMENT_3D('',#34237,#17669,#17670);
#15590=AXIS2_PLACEMENT_3D('',#34239,#17671,#17672);
#15591=AXIS2_PLACEMENT_3D('',#34241,#17673,#17674);
#15592=AXIS2_PLACEMENT_3D('',#34243,#17675,#17676);
#15593=AXIS2_PLACEMENT_3D('',#34245,#17677,#17678);
#15594=AXIS2_PLACEMENT_3D('',#34247,#17679,#17680);
#15595=AXIS2_PLACEMENT_3D('',#34249,#17681,#17682);
#15596=AXIS2_PLACEMENT_3D('',#34251,#17683,#17684);
#15597=AXIS2_PLACEMENT_3D('',#34253,#17685,#17686);
#15598=AXIS2_PLACEMENT_3D('',#34255,#17687,#17688);
#15599=AXIS2_PLACEMENT_3D('',#34257,#17689,#17690);
#15600=AXIS2_PLACEMENT_3D('',#34258,#17691,#17692);
#15601=AXIS2_PLACEMENT_3D('',#34259,#17693,#17694);
#15602=AXIS2_PLACEMENT_3D('',#34260,#17695,#17696);
#15603=AXIS2_PLACEMENT_3D('',#34261,#17697,#17698);
#15604=AXIS2_PLACEMENT_3D('',#34263,#17699,#17700);
#15605=AXIS2_PLACEMENT_3D('',#34265,#17702,#17703);
#15606=AXIS2_PLACEMENT_3D('',#34266,#17704,#17705);
#15607=AXIS2_PLACEMENT_3D('',#34267,#17706,#17707);
#15608=AXIS2_PLACEMENT_3D('',#34268,#17708,#17709);
#15609=AXIS2_PLACEMENT_3D('',#34270,#17711,#17712);
#15610=AXIS2_PLACEMENT_3D('',#34272,#17714,#17715);
#15611=AXIS2_PLACEMENT_3D('',#34273,#17716,#17717);
#15612=AXIS2_PLACEMENT_3D('',#34275,#17719,#17720);
#15613=AXIS2_PLACEMENT_3D('',#34276,#17721,#17722);
#15614=AXIS2_PLACEMENT_3D('',#34282,#17726,#17727);
#15615=AXIS2_PLACEMENT_3D('',#34286,#17730,#17731);
#15616=AXIS2_PLACEMENT_3D('',#34322,#17750,#17751);
#15617=AXIS2_PLACEMENT_3D('',#34325,#17754,#17755);
#15618=AXIS2_PLACEMENT_3D('',#34327,#17757,#17758);
#15619=AXIS2_PLACEMENT_3D('',#34329,#17760,#17761);
#15620=AXIS2_PLACEMENT_3D('',#34331,#17763,#17764);
#15621=AXIS2_PLACEMENT_3D('',#34333,#17766,#17767);
#15622=AXIS2_PLACEMENT_3D('',#34335,#17769,#17770);
#15623=AXIS2_PLACEMENT_3D('',#34337,#17772,#17773);
#15624=AXIS2_PLACEMENT_3D('',#34339,#17775,#17776);
#15625=AXIS2_PLACEMENT_3D('',#34341,#17778,#17779);
#15626=AXIS2_PLACEMENT_3D('',#34343,#17781,#17782);
#15627=AXIS2_PLACEMENT_3D('',#34345,#17784,#17785);
#15628=AXIS2_PLACEMENT_3D('',#34347,#17787,#17788);
#15629=AXIS2_PLACEMENT_3D('',#34349,#17790,#17791);
#15630=AXIS2_PLACEMENT_3D('',#34351,#17793,#17794);
#15631=AXIS2_PLACEMENT_3D('',#34353,#17796,#17797);
#15632=AXIS2_PLACEMENT_3D('',#34355,#17799,#17800);
#15633=AXIS2_PLACEMENT_3D('',#34356,#17801,#17802);
#15634=AXIS2_PLACEMENT_3D('',#34357,#17803,#17804);
#15635=AXIS2_PLACEMENT_3D('',#34358,#17805,#17806);
#15636=AXIS2_PLACEMENT_3D('',#34360,#17808,#17809);
#15637=AXIS2_PLACEMENT_3D('',#34361,#17810,#17811);
#15638=AXIS2_PLACEMENT_3D('',#34362,#17812,#17813);
#15639=AXIS2_PLACEMENT_3D('',#34364,#17815,#17816);
#15640=AXIS2_PLACEMENT_3D('',#34365,#17817,#17818);
#15641=AXIS2_PLACEMENT_3D('',#34366,#17819,#17820);
#15642=AXIS2_PLACEMENT_3D('',#34368,#17822,#17823);
#15643=AXIS2_PLACEMENT_3D('',#34369,#17824,#17825);
#15644=AXIS2_PLACEMENT_3D('',#34370,#17826,#17827);
#15645=AXIS2_PLACEMENT_3D('',#34372,#17829,#17830);
#15646=AXIS2_PLACEMENT_3D('',#34374,#17832,#17833);
#15647=AXIS2_PLACEMENT_3D('',#34375,#17834,#17835);
#15648=AXIS2_PLACEMENT_3D('',#34376,#17836,#17837);
#15649=AXIS2_PLACEMENT_3D('',#34417,#17858,#17859);
#15650=AXIS2_PLACEMENT_3D('',#34420,#17862,#17863);
#15651=AXIS2_PLACEMENT_3D('',#34422,#17865,#17866);
#15652=AXIS2_PLACEMENT_3D('',#34424,#17868,#17869);
#15653=AXIS2_PLACEMENT_3D('',#34426,#17871,#17872);
#15654=AXIS2_PLACEMENT_3D('',#34428,#17874,#17875);
#15655=AXIS2_PLACEMENT_3D('',#34430,#17877,#17878);
#15656=AXIS2_PLACEMENT_3D('',#34432,#17880,#17881);
#15657=AXIS2_PLACEMENT_3D('',#34434,#17883,#17884);
#15658=AXIS2_PLACEMENT_3D('',#34436,#17886,#17887);
#15659=AXIS2_PLACEMENT_3D('',#34438,#17889,#17890);
#15660=AXIS2_PLACEMENT_3D('',#34440,#17892,#17893);
#15661=AXIS2_PLACEMENT_3D('',#34442,#17895,#17896);
#15662=AXIS2_PLACEMENT_3D('',#34444,#17898,#17899);
#15663=AXIS2_PLACEMENT_3D('',#34446,#17901,#17902);
#15664=AXIS2_PLACEMENT_3D('',#34448,#17904,#17905);
#15665=AXIS2_PLACEMENT_3D('',#34450,#17907,#17908);
#15666=AXIS2_PLACEMENT_3D('',#34452,#17910,#17911);
#15667=AXIS2_PLACEMENT_3D('',#34454,#17913,#17914);
#15668=AXIS2_PLACEMENT_3D('',#34456,#17916,#17917);
#15669=AXIS2_PLACEMENT_3D('',#34457,#17918,#17919);
#15670=AXIS2_PLACEMENT_3D('',#34458,#17920,#17921);
#15671=AXIS2_PLACEMENT_3D('',#34459,#17922,#17923);
#15672=AXIS2_PLACEMENT_3D('',#34460,#17924,#17925);
#15673=AXIS2_PLACEMENT_3D('',#34461,#17926,#17927);
#15674=AXIS2_PLACEMENT_3D('',#34462,#17928,#17929);
#15675=AXIS2_PLACEMENT_3D('',#34463,#17930,#17931);
#15676=AXIS2_PLACEMENT_3D('',#34464,#17932,#17933);
#15677=AXIS2_PLACEMENT_3D('',#34473,#17934,#17935);
#15678=AXIS2_PLACEMENT_3D('',#34474,#17936,#17937);
#15679=AXIS2_PLACEMENT_3D('',#34475,#17938,#17939);
#15680=AXIS2_PLACEMENT_3D('',#34476,#17940,#17941);
#15681=AXIS2_PLACEMENT_3D('',#34479,#17942,#17943);
#15682=AXIS2_PLACEMENT_3D('',#34481,#17944,#17945);
#15683=AXIS2_PLACEMENT_3D('',#34483,#17946,#17947);
#15684=AXIS2_PLACEMENT_3D('',#34487,#17949,#17950);
#15685=AXIS2_PLACEMENT_3D('',#34489,#17952,#17953);
#15686=AXIS2_PLACEMENT_3D('',#34491,#17954,#17955);
#15687=AXIS2_PLACEMENT_3D('',#34494,#17957,#17958);
#15688=AXIS2_PLACEMENT_3D('',#34495,#17959,#17960);
#15689=AXIS2_PLACEMENT_3D('',#34498,#17961,#17962);
#15690=AXIS2_PLACEMENT_3D('',#34502,#17964,#17965);
#15691=AXIS2_PLACEMENT_3D('',#34504,#17967,#17968);
#15692=AXIS2_PLACEMENT_3D('',#34507,#17969,#17970);
#15693=AXIS2_PLACEMENT_3D('',#34511,#17972,#17973);
#15694=AXIS2_PLACEMENT_3D('',#34513,#17975,#17976);
#15695=AXIS2_PLACEMENT_3D('',#34516,#17977,#17978);
#15696=AXIS2_PLACEMENT_3D('',#34520,#17980,#17981);
#15697=AXIS2_PLACEMENT_3D('',#34522,#17982,#17983);
#15698=AXIS2_PLACEMENT_3D('',#34524,#17985,#17986);
#15699=AXIS2_PLACEMENT_3D('',#34533,#17991,#17992);
#15700=AXIS2_PLACEMENT_3D('',#34539,#17996,#17997);
#15701=AXIS2_PLACEMENT_3D('',#34545,#18001,#18002);
#15702=AXIS2_PLACEMENT_3D('',#34554,#18007,#18008);
#15703=AXIS2_PLACEMENT_3D('',#34560,#18012,#18013);
#15704=AXIS2_PLACEMENT_3D('',#34566,#18017,#18018);
#15705=AXIS2_PLACEMENT_3D('',#34575,#18023,#18024);
#15706=AXIS2_PLACEMENT_3D('',#34584,#18029,#18030);
#15707=AXIS2_PLACEMENT_3D('',#34591,#18035,#18036);
#15708=AXIS2_PLACEMENT_3D('',#34602,#18043,#18044);
#15709=AXIS2_PLACEMENT_3D('',#34608,#18048,#18049);
#15710=AXIS2_PLACEMENT_3D('',#34614,#18053,#18054);
#15711=AXIS2_PLACEMENT_3D('',#34617,#18055,#18056);
#15712=AXIS2_PLACEMENT_3D('',#34626,#18061,#18062);
#15713=AXIS2_PLACEMENT_3D('',#34628,#18064,#18065);
#15714=AXIS2_PLACEMENT_3D('',#34636,#18069,#18070);
#15715=AXIS2_PLACEMENT_3D('',#34637,#18071,#18072);
#15716=AXIS2_PLACEMENT_3D('',#34638,#18073,#18074);
#15717=AXIS2_PLACEMENT_3D('',#34651,#18081,#18082);
#15718=AXIS2_PLACEMENT_3D('',#34664,#18089,#18090);
#15719=AXIS2_PLACEMENT_3D('',#34670,#18094,#18095);
#15720=AXIS2_PLACEMENT_3D('',#34679,#18100,#18101);
#15721=AXIS2_PLACEMENT_3D('',#34689,#18107,#18108);
#15722=AXIS2_PLACEMENT_3D('',#34693,#18111,#18112);
#15723=AXIS2_PLACEMENT_3D('',#34699,#18116,#18117);
#15724=AXIS2_PLACEMENT_3D('',#34701,#18119,#18120);
#15725=AXIS2_PLACEMENT_3D('',#34705,#18123,#18124);
#15726=AXIS2_PLACEMENT_3D('',#34711,#18128,#18129);
#15727=AXIS2_PLACEMENT_3D('',#34713,#18131,#18132);
#15728=AXIS2_PLACEMENT_3D('',#34718,#18134,#18135);
#15729=AXIS2_PLACEMENT_3D('',#34721,#18137,#18138);
#15730=AXIS2_PLACEMENT_3D('',#34722,#18139,#18140);
#15731=AXIS2_PLACEMENT_3D('',#34728,#18144,#18145);
#15732=AXIS2_PLACEMENT_3D('',#34734,#18149,#18150);
#15733=AXIS2_PLACEMENT_3D('',#34736,#18151,#18152);
#15734=AXIS2_PLACEMENT_3D('',#34739,#18154,#18155);
#15735=AXIS2_PLACEMENT_3D('',#34740,#18156,#18157);
#15736=AXIS2_PLACEMENT_3D('',#34742,#18158,#18159);
#15737=AXIS2_PLACEMENT_3D('',#34745,#18161,#18162);
#15738=AXIS2_PLACEMENT_3D('',#34746,#18163,#18164);
#15739=AXIS2_PLACEMENT_3D('',#34752,#18168,#18169);
#15740=AXIS2_PLACEMENT_3D('',#34758,#18173,#18174);
#15741=AXIS2_PLACEMENT_3D('',#34762,#18177,#18178);
#15742=AXIS2_PLACEMENT_3D('',#34763,#18179,#18180);
#15743=AXIS2_PLACEMENT_3D('',#34764,#18181,#18182);
#15744=AXIS2_PLACEMENT_3D('',#34765,#18183,#18184);
#15745=AXIS2_PLACEMENT_3D('',#34767,#18186,#18187);
#15746=AXIS2_PLACEMENT_3D('',#34770,#18190,#18191);
#15747=AXIS2_PLACEMENT_3D('',#34771,#18192,#18193);
#15748=AXIS2_PLACEMENT_3D('',#34772,#18194,#18195);
#15749=AXIS2_PLACEMENT_3D('',#34780,#18201,#18202);
#15750=AXIS2_PLACEMENT_3D('',#34786,#18206,#18207);
#15751=AXIS2_PLACEMENT_3D('',#34788,#18208,#18209);
#15752=AXIS2_PLACEMENT_3D('',#34790,#18210,#18211);
#15753=AXIS2_PLACEMENT_3D('',#34792,#18213,#18214);
#15754=AXIS2_PLACEMENT_3D('',#34800,#18219,#18220);
#15755=AXIS2_PLACEMENT_3D('',#34802,#18221,#18222);
#15756=AXIS2_PLACEMENT_3D('',#34804,#18223,#18224);
#15757=AXIS2_PLACEMENT_3D('',#34806,#18226,#18227);
#15758=AXIS2_PLACEMENT_3D('',#34808,#18228,#18229);
#15759=AXIS2_PLACEMENT_3D('',#34811,#18231,#18232);
#15760=AXIS2_PLACEMENT_3D('',#34812,#18233,#18234);
#15761=AXIS2_PLACEMENT_3D('',#34815,#18237,#18238);
#15762=AXIS2_PLACEMENT_3D('',#34817,#18239,#18240);
#15763=AXIS2_PLACEMENT_3D('',#34820,#18242,#18243);
#15764=AXIS2_PLACEMENT_3D('',#34821,#18244,#18245);
#15765=AXIS2_PLACEMENT_3D('',#34823,#18246,#18247);
#15766=AXIS2_PLACEMENT_3D('',#34825,#18248,#18249);
#15767=AXIS2_PLACEMENT_3D('',#34827,#18251,#18252);
#15768=AXIS2_PLACEMENT_3D('',#34833,#18256,#18257);
#15769=AXIS2_PLACEMENT_3D('',#34834,#18258,#18259);
#15770=AXIS2_PLACEMENT_3D('',#34835,#18260,#18261);
#15771=AXIS2_PLACEMENT_3D('',#34836,#18262,#18263);
#15772=AXIS2_PLACEMENT_3D('',#34838,#18264,#18265);
#15773=AXIS2_PLACEMENT_3D('',#34840,#18266,#18267);
#15774=AXIS2_PLACEMENT_3D('',#34842,#18269,#18270);
#15775=AXIS2_PLACEMENT_3D('',#34844,#18272,#18273);
#15776=AXIS2_PLACEMENT_3D('',#34846,#18275,#18276);
#15777=AXIS2_PLACEMENT_3D('',#34848,#18278,#18279);
#15778=AXIS2_PLACEMENT_3D('',#34849,#18280,#18281);
#15779=AXIS2_PLACEMENT_3D('',#34854,#18283,#18284);
#15780=AXIS2_PLACEMENT_3D('',#34860,#18288,#18289);
#15781=AXIS2_PLACEMENT_3D('',#34862,#18291,#18292);
#15782=AXIS2_PLACEMENT_3D('',#34874,#18299,#18300);
#15783=AXIS2_PLACEMENT_3D('',#34875,#18301,#18302);
#15784=AXIS2_PLACEMENT_3D('',#34885,#18308,#18309);
#15785=AXIS2_PLACEMENT_3D('',#34894,#18315,#18316);
#15786=AXIS2_PLACEMENT_3D('',#34909,#18325,#18326);
#15787=AXIS2_PLACEMENT_3D('',#34915,#18330,#18331);
#15788=AXIS2_PLACEMENT_3D('',#34921,#18335,#18336);
#15789=AXIS2_PLACEMENT_3D('',#34923,#18338,#18339);
#15790=AXIS2_PLACEMENT_3D('',#34925,#18341,#18342);
#15791=AXIS2_PLACEMENT_3D('',#34927,#18344,#18345);
#15792=AXIS2_PLACEMENT_3D('',#34933,#18349,#18350);
#15793=AXIS2_PLACEMENT_3D('',#34935,#18352,#18353);
#15794=AXIS2_PLACEMENT_3D('',#34937,#18355,#18356);
#15795=AXIS2_PLACEMENT_3D('',#34941,#18359,#18360);
#15796=AXIS2_PLACEMENT_3D('',#34949,#18365,#18366);
#15797=AXIS2_PLACEMENT_3D('',#34955,#18370,#18371);
#15798=AXIS2_PLACEMENT_3D('',#34962,#18376,#18377);
#15799=AXIS2_PLACEMENT_3D('',#34968,#18381,#18382);
#15800=AXIS2_PLACEMENT_3D('',#34969,#18383,#18384);
#15801=AXIS2_PLACEMENT_3D('',#34970,#18385,#18386);
#15802=AXIS2_PLACEMENT_3D('',#34971,#18387,#18388);
#15803=AXIS2_PLACEMENT_3D('',#34973,#18389,#18390);
#15804=AXIS2_PLACEMENT_3D('',#34975,#18392,#18393);
#15805=AXIS2_PLACEMENT_3D('',#34979,#18396,#18397);
#15806=AXIS2_PLACEMENT_3D('',#34985,#18401,#18402);
#15807=AXIS2_PLACEMENT_3D('',#34991,#18406,#18407);
#15808=AXIS2_PLACEMENT_3D('',#34996,#18411,#18412);
#15809=AXIS2_PLACEMENT_3D('',#35001,#18416,#18417);
#15810=AXIS2_PLACEMENT_3D('',#35007,#18420,#18421);
#15811=AXIS2_PLACEMENT_3D('',#35011,#18424,#18425);
#15812=AXIS2_PLACEMENT_3D('',#35012,#18426,#18427);
#15813=AXIS2_PLACEMENT_3D('',#35015,#18429,#18430);
#15814=AXIS2_PLACEMENT_3D('',#35016,#18431,#18432);
#15815=AXIS2_PLACEMENT_3D('',#35018,#18433,#18434);
#15816=AXIS2_PLACEMENT_3D('',#35021,#18437,#18438);
#15817=AXIS2_PLACEMENT_3D('',#35022,#18439,#18440);
#15818=AXIS2_PLACEMENT_3D('',#35027,#18443,#18444);
#15819=AXIS2_PLACEMENT_3D('',#35029,#18446,#18447);
#15820=AXIS2_PLACEMENT_3D('',#35033,#18450,#18451);
#15821=AXIS2_PLACEMENT_3D('',#35041,#18456,#18457);
#15822=AXIS2_PLACEMENT_3D('',#35042,#18458,#18459);
#15823=AXIS2_PLACEMENT_3D('',#35043,#18460,#18461);
#15824=AXIS2_PLACEMENT_3D('',#35045,#18463,#18464);
#15825=AXIS2_PLACEMENT_3D('',#35048,#18466,#18467);
#15826=AXIS2_PLACEMENT_3D('',#35049,#18468,#18469);
#15827=AXIS2_PLACEMENT_3D('',#35052,#18472,#18473);
#15828=AXIS2_PLACEMENT_3D('',#35056,#18476,#18477);
#15829=AXIS2_PLACEMENT_3D('',#35057,#18478,#18479);
#15830=AXIS2_PLACEMENT_3D('',#35062,#18483,#18484);
#15831=AXIS2_PLACEMENT_3D('',#35064,#18486,#18487);
#15832=AXIS2_PLACEMENT_3D('',#35065,#18488,#18489);
#15833=AXIS2_PLACEMENT_3D('',#35071,#18493,#18494);
#15834=AXIS2_PLACEMENT_3D('',#35074,#18496,#18497);
#15835=AXIS2_PLACEMENT_3D('',#35075,#18498,#18499);
#15836=AXIS2_PLACEMENT_3D('',#35079,#18502,#18503);
#15837=AXIS2_PLACEMENT_3D('',#35082,#18505,#18506);
#15838=AXIS2_PLACEMENT_3D('',#35083,#18507,#18508);
#15839=AXIS2_PLACEMENT_3D('',#35087,#18511,#18512);
#15840=AXIS2_PLACEMENT_3D('',#35090,#18514,#18515);
#15841=AXIS2_PLACEMENT_3D('',#35091,#18516,#18517);
#15842=AXIS2_PLACEMENT_3D('',#35094,#18519,#18520);
#15843=AXIS2_PLACEMENT_3D('',#35095,#18521,#18522);
#15844=AXIS2_PLACEMENT_3D('',#35096,#18523,#18524);
#15845=AXIS2_PLACEMENT_3D('',#35097,#18525,#18526);
#15846=AXIS2_PLACEMENT_3D('',#35101,#18530,#18531);
#15847=AXIS2_PLACEMENT_3D('',#35104,#18534,#18535);
#15848=AXIS2_PLACEMENT_3D('',#35105,#18536,#18537);
#15849=AXIS2_PLACEMENT_3D('',#35114,#18542,#18543);
#15850=AXIS2_PLACEMENT_3D('',#35123,#18548,#18549);
#15851=AXIS2_PLACEMENT_3D('',#35130,#18554,#18555);
#15852=AXIS2_PLACEMENT_3D('',#35134,#18558,#18559);
#15853=AXIS2_PLACEMENT_3D('',#35138,#18562,#18563);
#15854=AXIS2_PLACEMENT_3D('',#35141,#18566,#18567);
#15855=AXIS2_PLACEMENT_3D('',#35145,#18570,#18571);
#15856=AXIS2_PLACEMENT_3D('',#35147,#18573,#18574);
#15857=AXIS2_PLACEMENT_3D('',#35148,#18575,#18576);
#15858=AXIS2_PLACEMENT_3D('',#35149,#18577,#18578);
#15859=AXIS2_PLACEMENT_3D('',#35150,#18579,#18580);
#15860=AXIS2_PLACEMENT_3D('',#35153,#18581,#18582);
#15861=AXIS2_PLACEMENT_3D('',#35154,#18583,#18584);
#15862=AXIS2_PLACEMENT_3D('',#35156,#18585,#18586);
#15863=AXIS2_PLACEMENT_3D('',#35158,#18587,#18588);
#15864=AXIS2_PLACEMENT_3D('',#35160,#18589,#18590);
#15865=AXIS2_PLACEMENT_3D('',#35162,#18591,#18592);
#15866=AXIS2_PLACEMENT_3D('',#35163,#18593,#18594);
#15867=AXIS2_PLACEMENT_3D('',#35164,#18595,#18596);
#15868=AXIS2_PLACEMENT_3D('',#35167,#18597,#18598);
#15869=AXIS2_PLACEMENT_3D('',#35169,#18599,#18600);
#15870=AXIS2_PLACEMENT_3D('',#35171,#18601,#18602);
#15871=AXIS2_PLACEMENT_3D('',#35172,#18603,#18604);
#15872=AXIS2_PLACEMENT_3D('',#35174,#18605,#18606);
#15873=AXIS2_PLACEMENT_3D('',#35176,#18607,#18608);
#15874=AXIS2_PLACEMENT_3D('',#35177,#18609,#18610);
#15875=AXIS2_PLACEMENT_3D('',#35178,#18611,#18612);
#15876=AXIS2_PLACEMENT_3D('',#35362,#18613,#18614);
#15877=AXIS2_PLACEMENT_3D('',#35363,#18615,#18616);
#15878=AXIS2_PLACEMENT_3D('',#35364,#18617,#18618);
#15879=AXIS2_PLACEMENT_3D('',#35366,#18619,#18620);
#15880=AXIS2_PLACEMENT_3D('',#35368,#18621,#18622);
#15881=AXIS2_PLACEMENT_3D('',#35538,#18623,#18624);
#15882=AXIS2_PLACEMENT_3D('',#35540,#18625,#18626);
#15883=AXIS2_PLACEMENT_3D('',#35541,#18627,#18628);
#15884=AXIS2_PLACEMENT_3D('',#35542,#18629,#18630);
#15885=AXIS2_PLACEMENT_3D('',#35544,#18631,#18632);
#15886=AXIS2_PLACEMENT_3D('',#35545,#18633,#18634);
#15887=AXIS2_PLACEMENT_3D('',#35546,#18635,#18636);
#15888=AXIS2_PLACEMENT_3D('',#35548,#18637,#18638);
#15889=AXIS2_PLACEMENT_3D('',#35551,#18640,#18641);
#15890=AXIS2_PLACEMENT_3D('',#35552,#18642,#18643);
#15891=AXIS2_PLACEMENT_3D('',#35555,#18644,#18645);
#15892=AXIS2_PLACEMENT_3D('',#35556,#18646,#18647);
#15893=AXIS2_PLACEMENT_3D('',#35559,#18649,#18650);
#15894=AXIS2_PLACEMENT_3D('',#35560,#18651,#18652);
#15895=AXIS2_PLACEMENT_3D('',#35563,#18653,#18654);
#15896=AXIS2_PLACEMENT_3D('',#35564,#18655,#18656);
#15897=AXIS2_PLACEMENT_3D('',#35566,#18658,#18659);
#15898=AXIS2_PLACEMENT_3D('',#35569,#18660,#18661);
#15899=AXIS2_PLACEMENT_3D('',#35573,#18663,#18664);
#15900=AXIS2_PLACEMENT_3D('',#35577,#18666,#18667);
#15901=AXIS2_PLACEMENT_3D('',#35607,#18669,#18670);
#15902=AXIS2_PLACEMENT_3D('',#35611,#18672,#18673);
#15903=AXIS2_PLACEMENT_3D('',#35614,#18675,#18676);
#15904=AXIS2_PLACEMENT_3D('',#35615,#18677,#18678);
#15905=AXIS2_PLACEMENT_3D('',#35616,#18679,#18680);
#15906=AXIS2_PLACEMENT_3D('',#35618,#18681,#18682);
#15907=AXIS2_PLACEMENT_3D('',#35622,#18684,#18685);
#15908=AXIS2_PLACEMENT_3D('',#35647,#18688,#18689);
#15909=AXIS2_PLACEMENT_3D('',#35719,#18691,#18692);
#15910=AXIS2_PLACEMENT_3D('',#35729,#18694,#18695);
#15911=AXIS2_PLACEMENT_3D('',#35762,#18696,#18697);
#15912=AXIS2_PLACEMENT_3D('',#35764,#18698,#18699);
#15913=AXIS2_PLACEMENT_3D('',#35765,#18700,#18701);
#15914=AXIS2_PLACEMENT_3D('',#35766,#18702,#18703);
#15915=AXIS2_PLACEMENT_3D('',#35769,#18704,#18705);
#15916=AXIS2_PLACEMENT_3D('',#35786,#18706,#18707);
#15917=AXIS2_PLACEMENT_3D('',#35801,#18708,#18709);
#15918=AXIS2_PLACEMENT_3D('',#35804,#18710,#18711);
#15919=AXIS2_PLACEMENT_3D('',#35821,#18712,#18713);
#15920=AXIS2_PLACEMENT_3D('',#35836,#18714,#18715);
#15921=AXIS2_PLACEMENT_3D('',#35839,#18716,#18717);
#15922=AXIS2_PLACEMENT_3D('',#35843,#18719,#18720);
#15923=AXIS2_PLACEMENT_3D('',#35845,#18722,#18723);
#15924=AXIS2_PLACEMENT_3D('',#35847,#18724,#18725);
#15925=AXIS2_PLACEMENT_3D('',#36015,#18726,#18727);
#15926=AXIS2_PLACEMENT_3D('',#36058,#18728,#18729);
#15927=AXIS2_PLACEMENT_3D('',#36073,#18731,#18732);
#15928=AXIS2_PLACEMENT_3D('',#36077,#18734,#18735);
#15929=AXIS2_PLACEMENT_3D('',#36080,#18737,#18738);
#15930=AXIS2_PLACEMENT_3D('',#36081,#18739,#18740);
#15931=AXIS2_PLACEMENT_3D('',#36102,#18741,#18742);
#15932=AXIS2_PLACEMENT_3D('',#36119,#18743,#18744);
#15933=AXIS2_PLACEMENT_3D('',#36121,#18745,#18746);
#15934=AXIS2_PLACEMENT_3D('',#36134,#18747,#18748);
#15935=AXIS2_PLACEMENT_3D('',#36137,#18749,#18750);
#15936=AXIS2_PLACEMENT_3D('',#36139,#18751,#18752);
#15937=AXIS2_PLACEMENT_3D('',#36141,#18753,#18754);
#15938=AXIS2_PLACEMENT_3D('',#36142,#18755,#18756);
#15939=AXIS2_PLACEMENT_3D('',#36143,#18757,#18758);
#15940=AXIS2_PLACEMENT_3D('',#36145,#18759,#18760);
#15941=AXIS2_PLACEMENT_3D('',#36146,#18761,#18762);
#15942=AXIS2_PLACEMENT_3D('',#36147,#18763,#18764);
#15943=AXIS2_PLACEMENT_3D('',#36149,#18765,#18766);
#15944=AXIS2_PLACEMENT_3D('',#36152,#18768,#18769);
#15945=AXIS2_PLACEMENT_3D('',#36153,#18770,#18771);
#15946=AXIS2_PLACEMENT_3D('',#36155,#18772,#18773);
#15947=AXIS2_PLACEMENT_3D('',#36157,#18774,#18775);
#15948=AXIS2_PLACEMENT_3D('',#36346,#18777,#18778);
#15949=AXIS2_PLACEMENT_3D('',#36351,#18781,#18782);
#15950=AXIS2_PLACEMENT_3D('',#36353,#18784,#18785);
#15951=AXIS2_PLACEMENT_3D('',#36357,#18787,#18788);
#15952=AXIS2_PLACEMENT_3D('',#36359,#18789,#18790);
#15953=AXIS2_PLACEMENT_3D('',#36361,#18792,#18793);
#15954=AXIS2_PLACEMENT_3D('',#36363,#18794,#18795);
#15955=AXIS2_PLACEMENT_3D('',#36365,#18796,#18797);
#15956=AXIS2_PLACEMENT_3D('',#36367,#18799,#18800);
#15957=AXIS2_PLACEMENT_3D('',#36370,#18801,#18802);
#15958=AXIS2_PLACEMENT_3D('',#36390,#18803,#18804);
#15959=AXIS2_PLACEMENT_3D('',#36391,#18805,#18806);
#15960=AXIS2_PLACEMENT_3D('',#36398,#18807,#18808);
#15961=AXIS2_PLACEMENT_3D('',#36413,#18809,#18810);
#15962=AXIS2_PLACEMENT_3D('',#36416,#18811,#18812);
#15963=AXIS2_PLACEMENT_3D('',#36582,#18813,#18814);
#15964=AXIS2_PLACEMENT_3D('',#36597,#18816,#18817);
#15965=AXIS2_PLACEMENT_3D('',#36601,#18819,#18820);
#15966=AXIS2_PLACEMENT_3D('',#36605,#18822,#18823);
#15967=AXIS2_PLACEMENT_3D('',#36609,#18825,#18826);
#15968=AXIS2_PLACEMENT_3D('',#36632,#18829,#18830);
#15969=AXIS2_PLACEMENT_3D('',#36675,#18832,#18833);
#15970=AXIS2_PLACEMENT_3D('',#36677,#18834,#18835);
#15971=AXIS2_PLACEMENT_3D('',#36679,#18837,#18838);
#15972=AXIS2_PLACEMENT_3D('',#36696,#18839,#18840);
#15973=AXIS2_PLACEMENT_3D('',#36697,#18841,#18842);
#15974=AXIS2_PLACEMENT_3D('',#36698,#18843,#18844);
#15975=AXIS2_PLACEMENT_3D('',#36701,#18845,#18846);
#15976=AXIS2_PLACEMENT_3D('',#36718,#18847,#18848);
#15977=AXIS2_PLACEMENT_3D('',#36733,#18849,#18850);
#15978=AXIS2_PLACEMENT_3D('',#36736,#18851,#18852);
#15979=AXIS2_PLACEMENT_3D('',#36751,#18853,#18854);
#15980=AXIS2_PLACEMENT_3D('',#38298,#18855,#18856);
#15981=AXIS2_PLACEMENT_3D('',#38514,#18857,#18858);
#15982=AXIS2_PLACEMENT_3D('',#38960,#18859,#18860);
#15983=AXIS2_PLACEMENT_3D('',#39176,#18861,#18862);
#15984=AXIS2_PLACEMENT_3D('',#39177,#18863,#18864);
#15985=AXIS2_PLACEMENT_3D('',#39179,#18866,#18867);
#15986=AXIS2_PLACEMENT_3D('',#39181,#18869,#18870);
#15987=AXIS2_PLACEMENT_3D('',#40483,#18871,#18872);
#15988=AXIS2_PLACEMENT_3D('',#41331,#18873,#18874);
#15989=AXIS2_PLACEMENT_3D('',#41334,#18877,#18878);
#15990=AXIS2_PLACEMENT_3D('',#41340,#18882,#18883);
#15991=AXIS2_PLACEMENT_3D('',#41344,#18887,#18888);
#15992=AXIS2_PLACEMENT_3D('',#41348,#18892,#18893);
#15993=AXIS2_PLACEMENT_3D('',#41357,#18898,#18899);
#15994=AXIS2_PLACEMENT_3D('',#41366,#18904,#18905);
#15995=AXIS2_PLACEMENT_3D('',#41375,#18910,#18911);
#15996=AXIS2_PLACEMENT_3D('',#41377,#18913,#18914);
#15997=AXIS2_PLACEMENT_3D('',#41379,#18916,#18917);
#15998=AXIS2_PLACEMENT_3D('',#41381,#18919,#18920);
#15999=AXIS2_PLACEMENT_3D('',#41400,#18921,#18922);
#16000=AXIS2_PLACEMENT_3D('',#41413,#18923,#18924);
#16001=AXIS2_PLACEMENT_3D('',#41414,#18925,#18926);
#16002=AXIS2_PLACEMENT_3D('',#41431,#18928,#18929);
#16003=AXIS2_PLACEMENT_3D('',#41448,#18931,#18932);
#16004=AXIS2_PLACEMENT_3D('',#41450,#18934,#18935);
#16005=AXIS2_PLACEMENT_3D('',#41452,#18937,#18938);
#16006=AXIS2_PLACEMENT_3D('',#41469,#18939,#18940);
#16007=AXIS2_PLACEMENT_3D('',#41485,#18941,#18942);
#16008=AXIS2_PLACEMENT_3D('',#41486,#18943,#18944);
#16009=AXIS2_PLACEMENT_3D('',#41489,#18945,#18946);
#16010=AXIS2_PLACEMENT_3D('',#41491,#18947,#18948);
#16011=AXIS2_PLACEMENT_3D('',#41493,#18949,#18950);
#16012=AXIS2_PLACEMENT_3D('',#41494,#18951,#18952);
#16013=AXIS2_PLACEMENT_3D('',#41495,#18953,#18954);
#16014=AXIS2_PLACEMENT_3D('',#41498,#18957,#18958);
#16015=AXIS2_PLACEMENT_3D('',#41501,#18959,#18960);
#16016=AXIS2_PLACEMENT_3D('',#41646,#18964,#18965);
#16017=AXIS2_PLACEMENT_3D('',#41648,#18966,#18967);
#16018=AXIS2_PLACEMENT_3D('',#41649,#18968,#18969);
#16019=AXIS2_PLACEMENT_3D('',#41650,#18970,#18971);
#16020=AXIS2_PLACEMENT_3D('',#41654,#18973,#18974);
#16021=AXIS2_PLACEMENT_3D('',#41954,#18976,#18977);
#16022=AXIS2_PLACEMENT_3D('',#41955,#18978,#18979);
#16023=AXIS2_PLACEMENT_3D('',#41959,#18982,#18983);
#16024=AXIS2_PLACEMENT_3D('',#41967,#18989,#18990);
#16025=AXIS2_PLACEMENT_3D('',#41969,#18992,#18993);
#16026=AXIS2_PLACEMENT_3D('',#41996,#18994,#18995);
#16027=AXIS2_PLACEMENT_3D('',#41997,#18996,#18997);
#16028=AXIS2_PLACEMENT_3D('',#41999,#18998,#18999);
#16029=AXIS2_PLACEMENT_3D('',#42002,#19001,#19002);
#16030=AXIS2_PLACEMENT_3D('',#42004,#19004,#19005);
#16031=AXIS2_PLACEMENT_3D('',#42006,#19007,#19008);
#16032=AXIS2_PLACEMENT_3D('',#42008,#19010,#19011);
#16033=AXIS2_PLACEMENT_3D('',#42012,#19014,#19015);
#16034=AXIS2_PLACEMENT_3D('',#42014,#19016,#19017);
#16035=AXIS2_PLACEMENT_3D('',#42016,#19018,#19019);
#16036=AXIS2_PLACEMENT_3D('',#42031,#19020,#19021);
#16037=AXIS2_PLACEMENT_3D('',#42034,#19023,#19024);
#16038=AXIS2_PLACEMENT_3D('',#42407,#19025,#19026);
#16039=AXIS2_PLACEMENT_3D('',#42408,#19027,#19028);
#16040=AXIS2_PLACEMENT_3D('',#42409,#19029,#19030);
#16041=AXIS2_PLACEMENT_3D('',#42411,#19032,#19033);
#16042=AXIS2_PLACEMENT_3D('',#42413,#19034,#19035);
#16043=AXIS2_PLACEMENT_3D('',#42561,#19037,#19038);
#16044=AXIS2_PLACEMENT_3D('',#42562,#19039,#19040);
#16045=AXIS2_PLACEMENT_3D('',#42682,#19042,#19043);
#16046=AXIS2_PLACEMENT_3D('',#42683,#19044,#19045);
#16047=AXIS2_PLACEMENT_3D('',#42684,#19046,#19047);
#16048=AXIS2_PLACEMENT_3D('',#42864,#19048,#19049);
#16049=AXIS2_PLACEMENT_3D('',#42865,#19050,#19051);
#16050=AXIS2_PLACEMENT_3D('',#42866,#19052,#19053);
#16051=AXIS2_PLACEMENT_3D('',#42867,#19054,#19055);
#16052=AXIS2_PLACEMENT_3D('',#42969,#19056,#19057);
#16053=AXIS2_PLACEMENT_3D('',#42970,#19058,#19059);
#16054=AXIS2_PLACEMENT_3D('',#42971,#19060,#19061);
#16055=AXIS2_PLACEMENT_3D('',#42987,#19062,#19063);
#16056=AXIS2_PLACEMENT_3D('',#42988,#19064,#19065);
#16057=AXIS2_PLACEMENT_3D('',#43115,#19066,#19067);
#16058=AXIS2_PLACEMENT_3D('',#43118,#19069,#19070);
#16059=AXIS2_PLACEMENT_3D('',#43119,#19071,#19072);
#16060=AXIS2_PLACEMENT_3D('',#43121,#19073,#19074);
#16061=AXIS2_PLACEMENT_3D('',#43133,#19075,#19076);
#16062=AXIS2_PLACEMENT_3D('',#43134,#19077,#19078);
#16063=AXIS2_PLACEMENT_3D('',#43138,#19080,#19081);
#16064=AXIS2_PLACEMENT_3D('',#43141,#19083,#19084);
#16065=AXIS2_PLACEMENT_3D('',#43142,#19085,#19086);
#16066=AXIS2_PLACEMENT_3D('',#43177,#19090,#19091);
#16067=AXIS2_PLACEMENT_3D('',#43179,#19092,#19093);
#16068=AXIS2_PLACEMENT_3D('',#43180,#19094,#19095);
#16069=AXIS2_PLACEMENT_3D('',#43181,#19096,#19097);
#16070=AXIS2_PLACEMENT_3D('',#43182,#19098,#19099);
#16071=AXIS2_PLACEMENT_3D('',#43183,#19100,#19101);
#16072=AXIS2_PLACEMENT_3D('',#43184,#19102,#19103);
#16073=AXIS2_PLACEMENT_3D('',#43188,#19105,#19106);
#16074=AXIS2_PLACEMENT_3D('',#43189,#19107,#19108);
#16075=AXIS2_PLACEMENT_3D('',#43190,#19109,#19110);
#16076=AXIS2_PLACEMENT_3D('',#43193,#19112,#19113);
#16077=AXIS2_PLACEMENT_3D('',#43194,#19114,#19115);
#16078=AXIS2_PLACEMENT_3D('',#43198,#19118,#19119);
#16079=AXIS2_PLACEMENT_3D('',#43200,#19121,#19122);
#16080=AXIS2_PLACEMENT_3D('',#43208,#19127,#19128);
#16081=AXIS2_PLACEMENT_3D('',#43227,#19135,#19136);
#16082=AXIS2_PLACEMENT_3D('',#43229,#19137,#19138);
#16083=AXIS2_PLACEMENT_3D('',#43296,#19140,#19141);
#16084=AXIS2_PLACEMENT_3D('',#43362,#19142,#19143);
#16085=AXIS2_PLACEMENT_3D('',#43363,#19144,#19145);
#16086=AXIS2_PLACEMENT_3D('',#43395,#19147,#19148);
#16087=AXIS2_PLACEMENT_3D('',#43397,#19149,#19150);
#16088=AXIS2_PLACEMENT_3D('',#43398,#19151,#19152);
#16089=AXIS2_PLACEMENT_3D('',#43399,#19153,#19154);
#16090=AXIS2_PLACEMENT_3D('',#43401,#19155,#19156);
#16091=AXIS2_PLACEMENT_3D('',#43402,#19157,#19158);
#16092=AXIS2_PLACEMENT_3D('',#43403,#19159,#19160);
#16093=AXIS2_PLACEMENT_3D('',#43730,#19162,#19163);
#16094=AXIS2_PLACEMENT_3D('',#43732,#19164,#19165);
#16095=AXIS2_PLACEMENT_3D('',#43743,#19166,#19167);
#16096=AXIS2_PLACEMENT_3D('',#43744,#19168,#19169);
#16097=AXIS2_PLACEMENT_3D('',#43745,#19170,#19171);
#16098=AXIS2_PLACEMENT_3D('',#43746,#19172,#19173);
#16099=AXIS2_PLACEMENT_3D('',#43747,#19174,#19175);
#16100=AXIS2_PLACEMENT_3D('',#43748,#19176,#19177);
#16101=AXIS2_PLACEMENT_3D('',#43749,#19178,#19179);
#16102=AXIS2_PLACEMENT_3D('',#43751,#19181,#19182);
#16103=AXIS2_PLACEMENT_3D('',#43755,#19184,#19185);
#16104=AXIS2_PLACEMENT_3D('',#43761,#19188,#19189);
#16105=AXIS2_PLACEMENT_3D('',#43764,#19191,#19192);
#16106=AXIS2_PLACEMENT_3D('',#43765,#19193,#19194);
#16107=AXIS2_PLACEMENT_3D('',#43766,#19195,#19196);
#16108=AXIS2_PLACEMENT_3D('',#43767,#19197,#19198);
#16109=AXIS2_PLACEMENT_3D('',#43768,#19199,#19200);
#16110=AXIS2_PLACEMENT_3D('',#43780,#19202,#19203);
#16111=AXIS2_PLACEMENT_3D('',#43781,#19204,#19205);
#16112=AXIS2_PLACEMENT_3D('',#43782,#19206,#19207);
#16113=AXIS2_PLACEMENT_3D('',#43783,#19208,#19209);
#16114=AXIS2_PLACEMENT_3D('',#43785,#19210,#19211);
#16115=AXIS2_PLACEMENT_3D('',#43788,#19213,#19214);
#16116=AXIS2_PLACEMENT_3D('',#43789,#19215,#19216);
#16117=AXIS2_PLACEMENT_3D('',#43792,#19218,#19219);
#16118=AXIS2_PLACEMENT_3D('',#43795,#19221,#19222);
#16119=AXIS2_PLACEMENT_3D('',#43796,#19223,#19224);
#16120=AXIS2_PLACEMENT_3D('',#43801,#19226,#19227);
#16121=AXIS2_PLACEMENT_3D('',#43804,#19229,#19230);
#16122=AXIS2_PLACEMENT_3D('',#43805,#19231,#19232);
#16123=AXIS2_PLACEMENT_3D('',#43809,#19234,#19235);
#16124=AXIS2_PLACEMENT_3D('',#43811,#19237,#19238);
#16125=AXIS2_PLACEMENT_3D('',#43816,#19242,#19243);
#16126=AXIS2_PLACEMENT_3D('',#43817,#19244,#19245);
#16127=AXIS2_PLACEMENT_3D('',#43818,#19246,#19247);
#16128=AXIS2_PLACEMENT_3D('',#43819,#19248,#19249);
#16129=AXIS2_PLACEMENT_3D('',#43820,#19250,#19251);
#16130=AXIS2_PLACEMENT_3D('',#43821,#19252,#19253);
#16131=AXIS2_PLACEMENT_3D('',#43822,#19254,#19255);
#16132=AXIS2_PLACEMENT_3D('',#43823,#19256,#19257);
#16133=AXIS2_PLACEMENT_3D('',#43844,#19258,#19259);
#16134=AXIS2_PLACEMENT_3D('',#43845,#19260,#19261);
#16135=AXIS2_PLACEMENT_3D('',#43874,#19262,#19263);
#16136=AXIS2_PLACEMENT_3D('',#43875,#19264,#19265);
#16137=AXIS2_PLACEMENT_3D('',#43890,#19266,#19267);
#16138=AXIS2_PLACEMENT_3D('',#43891,#19268,#19269);
#16139=AXIS2_PLACEMENT_3D('',#43906,#19270,#19271);
#16140=AXIS2_PLACEMENT_3D('',#43913,#19272,#19273);
#16141=AXIS2_PLACEMENT_3D('',#43915,#19275,#19276);
#16142=AXIS2_PLACEMENT_3D('',#43916,#19277,#19278);
#16143=AXIS2_PLACEMENT_3D('',#43917,#19279,#19280);
#16144=AXIS2_PLACEMENT_3D('',#43935,#19281,#19282);
#16145=AXIS2_PLACEMENT_3D('',#43937,#19284,#19285);
#16146=AXIS2_PLACEMENT_3D('',#43938,#19286,#19287);
#16147=AXIS2_PLACEMENT_3D('',#43975,#19288,#19289);
#16148=AXIS2_PLACEMENT_3D('',#43980,#19292,#19293);
#16149=AXIS2_PLACEMENT_3D('',#43981,#19294,#19295);
#16150=AXIS2_PLACEMENT_3D('',#43982,#19296,#19297);
#16151=AXIS2_PLACEMENT_3D('',#43983,#19298,#19299);
#16152=AXIS2_PLACEMENT_3D('',#43984,#19300,#19301);
#16153=AXIS2_PLACEMENT_3D('',#44213,#19302,#19303);
#16154=AXIS2_PLACEMENT_3D('',#44214,#19304,#19305);
#16155=AXIS2_PLACEMENT_3D('',#44217,#19308,#19309);
#16156=AXIS2_PLACEMENT_3D('',#44218,#19310,#19311);
#16157=AXIS2_PLACEMENT_3D('',#44247,#19312,#19313);
#16158=AXIS2_PLACEMENT_3D('',#44360,#19314,#19315);
#16159=AXIS2_PLACEMENT_3D('',#44361,#19316,#19317);
#16160=AXIS2_PLACEMENT_3D('',#44362,#19318,#19319);
#16161=AXIS2_PLACEMENT_3D('',#44391,#19320,#19321);
#16162=AXIS2_PLACEMENT_3D('',#44392,#19322,#19323);
#16163=AXIS2_PLACEMENT_3D('',#44393,#19324,#19325);
#16164=AXIS2_PLACEMENT_3D('',#44408,#19326,#19327);
#16165=AXIS2_PLACEMENT_3D('',#44421,#19328,#19329);
#16166=AXIS2_PLACEMENT_3D('',#44422,#19330,#19331);
#16167=AXIS2_PLACEMENT_3D('',#44423,#19332,#19333);
#16168=AXIS2_PLACEMENT_3D('',#44424,#19334,#19335);
#16169=AXIS2_PLACEMENT_3D('',#44425,#19336,#19337);
#16170=AXIS2_PLACEMENT_3D('',#44429,#19340,#19341);
#16171=AXIS2_PLACEMENT_3D('',#44431,#19343,#19344);
#16172=AXIS2_PLACEMENT_3D('',#44432,#19345,#19346);
#16173=AXIS2_PLACEMENT_3D('',#44433,#19347,#19348);
#16174=AXIS2_PLACEMENT_3D('',#44434,#19349,#19350);
#16175=AXIS2_PLACEMENT_3D('',#44435,#19351,#19352);
#16176=AXIS2_PLACEMENT_3D('',#44436,#19353,#19354);
#16177=AXIS2_PLACEMENT_3D('',#44437,#19355,#19356);
#16178=AXIS2_PLACEMENT_3D('',#44439,#19357,#19358);
#16179=AXIS2_PLACEMENT_3D('',#44442,#19359,#19360);
#16180=AXIS2_PLACEMENT_3D('',#44444,#19361,#19362);
#16181=AXIS2_PLACEMENT_3D('',#44446,#19363,#19364);
#16182=AXIS2_PLACEMENT_3D('',#44448,#19365,#19366);
#16183=AXIS2_PLACEMENT_3D('',#44450,#19367,#19368);
#16184=AXIS2_PLACEMENT_3D('',#44452,#19369,#19370);
#16185=AXIS2_PLACEMENT_3D('',#44454,#19371,#19372);
#16186=AXIS2_PLACEMENT_3D('',#44456,#19373,#19374);
#16187=AXIS2_PLACEMENT_3D('',#44458,#19375,#19376);
#16188=AXIS2_PLACEMENT_3D('',#44460,#19377,#19378);
#16189=AXIS2_PLACEMENT_3D('',#44462,#19379,#19380);
#16190=AXIS2_PLACEMENT_3D('',#44463,#19381,#19382);
#16191=AXIS2_PLACEMENT_3D('',#44464,#19383,#19384);
#16192=AXIS2_PLACEMENT_3D('',#44467,#19385,#19386);
#16193=AXIS2_PLACEMENT_3D('',#44470,#19388,#19389);
#16194=AXIS2_PLACEMENT_3D('',#44471,#19390,#19391);
#16195=AXIS2_PLACEMENT_3D('',#44472,#19392,#19393);
#16196=AXIS2_PLACEMENT_3D('',#44475,#19395,#19396);
#16197=AXIS2_PLACEMENT_3D('',#44476,#19397,#19398);
#16198=AXIS2_PLACEMENT_3D('',#44478,#19399,#19400);
#16199=AXIS2_PLACEMENT_3D('',#44480,#19402,#19403);
#16200=AXIS2_PLACEMENT_3D('',#44481,#19404,#19405);
#16201=AXIS2_PLACEMENT_3D('',#44487,#19409,#19410);
#16202=AXIS2_PLACEMENT_3D('',#44491,#19413,#19414);
#16203=AXIS2_PLACEMENT_3D('',#44495,#19417,#19418);
#16204=AXIS2_PLACEMENT_3D('',#44499,#19421,#19422);
#16205=AXIS2_PLACEMENT_3D('',#44503,#19425,#19426);
#16206=AXIS2_PLACEMENT_3D('',#44507,#19429,#19430);
#16207=AXIS2_PLACEMENT_3D('',#44511,#19433,#19434);
#16208=AXIS2_PLACEMENT_3D('',#44515,#19437,#19438);
#16209=AXIS2_PLACEMENT_3D('',#44519,#19441,#19442);
#16210=AXIS2_PLACEMENT_3D('',#44523,#19445,#19446);
#16211=AXIS2_PLACEMENT_3D('',#44527,#19449,#19450);
#16212=AXIS2_PLACEMENT_3D('',#44529,#19452,#19453);
#16213=AXIS2_PLACEMENT_3D('',#44530,#19454,#19455);
#16214=AXIS2_PLACEMENT_3D('',#44531,#19456,#19457);
#16215=AXIS2_PLACEMENT_3D('',#44532,#19458,#19459);
#16216=AXIS2_PLACEMENT_3D('',#44537,#19461,#19462);
#16217=AXIS2_PLACEMENT_3D('',#44563,#19464,#19465);
#16218=AXIS2_PLACEMENT_3D('',#44566,#19467,#19468);
#16219=AXIS2_PLACEMENT_3D('',#44568,#19469,#19470);
#16220=AXIS2_PLACEMENT_3D('',#44571,#19472,#19473);
#16221=AXIS2_PLACEMENT_3D('',#44572,#19474,#19475);
#16222=AXIS2_PLACEMENT_3D('',#44577,#19477,#19478);
#16223=AXIS2_PLACEMENT_3D('',#44580,#19480,#19481);
#16224=AXIS2_PLACEMENT_3D('',#44582,#19482,#19483);
#16225=AXIS2_PLACEMENT_3D('',#44585,#19485,#19486);
#16226=AXIS2_PLACEMENT_3D('',#44586,#19487,#19488);
#16227=AXIS2_PLACEMENT_3D('',#44591,#19490,#19491);
#16228=AXIS2_PLACEMENT_3D('',#44617,#19493,#19494);
#16229=AXIS2_PLACEMENT_3D('',#44621,#19496,#19497);
#16230=AXIS2_PLACEMENT_3D('',#44646,#19499,#19500);
#16231=AXIS2_PLACEMENT_3D('',#44648,#19501,#19502);
#16232=AXIS2_PLACEMENT_3D('',#44651,#19504,#19505);
#16233=AXIS2_PLACEMENT_3D('',#44653,#19506,#19507);
#16234=AXIS2_PLACEMENT_3D('',#44656,#19509,#19510);
#16235=AXIS2_PLACEMENT_3D('',#44657,#19511,#19512);
#16236=AXIS2_PLACEMENT_3D('',#44659,#19513,#19514);
#16237=AXIS2_PLACEMENT_3D('',#44663,#19516,#19517);
#16238=AXIS2_PLACEMENT_3D('',#44689,#19519,#19520);
#16239=AXIS2_PLACEMENT_3D('',#44693,#19522,#19523);
#16240=AXIS2_PLACEMENT_3D('',#44696,#19525,#19526);
#16241=AXIS2_PLACEMENT_3D('',#44697,#19527,#19528);
#16242=AXIS2_PLACEMENT_3D('',#44702,#19530,#19531);
#16243=AXIS2_PLACEMENT_3D('',#44728,#19533,#19534);
#16244=AXIS2_PLACEMENT_3D('',#44732,#19536,#19537);
#16245=AXIS2_PLACEMENT_3D('',#44757,#19539,#19540);
#16246=AXIS2_PLACEMENT_3D('',#44758,#19541,#19542);
#16247=AXIS2_PLACEMENT_3D('',#44763,#19544,#19545);
#16248=AXIS2_PLACEMENT_3D('',#44789,#19547,#19548);
#16249=AXIS2_PLACEMENT_3D('',#44793,#19550,#19551);
#16250=AXIS2_PLACEMENT_3D('',#44818,#19553,#19554);
#16251=AXIS2_PLACEMENT_3D('',#44819,#19555,#19556);
#16252=AXIS2_PLACEMENT_3D('',#44821,#19557,#19558);
#16253=AXIS2_PLACEMENT_3D('',#44824,#19560,#19561);
#16254=AXIS2_PLACEMENT_3D('',#44825,#19562,#19563);
#16255=AXIS2_PLACEMENT_3D('',#44827,#19564,#19565);
#16256=AXIS2_PLACEMENT_3D('',#44830,#19567,#19568);
#16257=AXIS2_PLACEMENT_3D('',#44831,#19569,#19570);
#16258=AXIS2_PLACEMENT_3D('',#44833,#19571,#19572);
#16259=AXIS2_PLACEMENT_3D('',#44836,#19574,#19575);
#16260=AXIS2_PLACEMENT_3D('',#44837,#19576,#19577);
#16261=AXIS2_PLACEMENT_3D('',#44840,#19578,#19579);
#16262=AXIS2_PLACEMENT_3D('',#44844,#19581,#19582);
#16263=AXIS2_PLACEMENT_3D('',#44846,#19584,#19585);
#16264=AXIS2_PLACEMENT_3D('',#44848,#19586,#19587);
#16265=AXIS2_PLACEMENT_3D('',#44851,#19589,#19590);
#16266=AXIS2_PLACEMENT_3D('',#44852,#19591,#19592);
#16267=AXIS2_PLACEMENT_3D('',#44854,#19593,#19594);
#16268=AXIS2_PLACEMENT_3D('',#44857,#19596,#19597);
#16269=AXIS2_PLACEMENT_3D('',#44858,#19598,#19599);
#16270=AXIS2_PLACEMENT_3D('',#44860,#19600,#19601);
#16271=AXIS2_PLACEMENT_3D('',#44864,#19603,#19604);
#16272=AXIS2_PLACEMENT_3D('',#44868,#19606,#19607);
#16273=AXIS2_PLACEMENT_3D('',#44871,#19609,#19610);
#16274=AXIS2_PLACEMENT_3D('',#44872,#19611,#19612);
#16275=AXIS2_PLACEMENT_3D('',#44874,#19613,#19614);
#16276=AXIS2_PLACEMENT_3D('',#44877,#19616,#19617);
#16277=AXIS2_PLACEMENT_3D('',#44878,#19618,#19619);
#16278=AXIS2_PLACEMENT_3D('',#44880,#19620,#19621);
#16279=AXIS2_PLACEMENT_3D('',#44883,#19623,#19624);
#16280=AXIS2_PLACEMENT_3D('',#44884,#19625,#19626);
#16281=AXIS2_PLACEMENT_3D('',#44886,#19627,#19628);
#16282=AXIS2_PLACEMENT_3D('',#44890,#19630,#19631);
#16283=AXIS2_PLACEMENT_3D('',#44894,#19633,#19634);
#16284=AXIS2_PLACEMENT_3D('',#44897,#19636,#19637);
#16285=AXIS2_PLACEMENT_3D('',#44898,#19638,#19639);
#16286=AXIS2_PLACEMENT_3D('',#44900,#19640,#19641);
#16287=AXIS2_PLACEMENT_3D('',#44902,#19642,#19643);
#16288=AXIS2_PLACEMENT_3D('',#44904,#19645,#19646);
#16289=AXIS2_PLACEMENT_3D('',#44906,#19647,#19648);
#16290=AXIS2_PLACEMENT_3D('',#44909,#19650,#19651);
#16291=AXIS2_PLACEMENT_3D('',#44910,#19652,#19653);
#16292=AXIS2_PLACEMENT_3D('',#44911,#19654,#19655);
#16293=AXIS2_PLACEMENT_3D('',#44912,#19656,#19657);
#16294=AXIS2_PLACEMENT_3D('',#44914,#19658,#19659);
#16295=AXIS2_PLACEMENT_3D('',#44917,#19661,#19662);
#16296=AXIS2_PLACEMENT_3D('',#44918,#19663,#19664);
#16297=AXIS2_PLACEMENT_3D('',#44919,#19665,#19666);
#16298=AXIS2_PLACEMENT_3D('',#44922,#19669,#19670);
#16299=AXIS2_PLACEMENT_3D('',#44925,#19673,#19674);
#16300=AXIS2_PLACEMENT_3D('',#44928,#19675,#19676);
#16301=AXIS2_PLACEMENT_3D('',#44932,#19678,#19679);
#16302=AXIS2_PLACEMENT_3D('',#44934,#19681,#19682);
#16303=AXIS2_PLACEMENT_3D('',#44938,#19686,#19687);
#16304=AXIS2_PLACEMENT_3D('',#44942,#19689,#19690);
#16305=AXIS2_PLACEMENT_3D('',#44944,#19692,#19693);
#16306=AXIS2_PLACEMENT_3D('',#44945,#19694,#19695);
#16307=AXIS2_PLACEMENT_3D('',#44952,#19700,#19701);
#16308=AXIS2_PLACEMENT_3D('',#44956,#19703,#19704);
#16309=AXIS2_PLACEMENT_3D('',#44958,#19706,#19707);
#16310=AXIS2_PLACEMENT_3D('',#44960,#19709,#19710);
#16311=AXIS2_PLACEMENT_3D('',#44962,#19712,#19713);
#16312=AXIS2_PLACEMENT_3D('',#44968,#19717,#19718);
#16313=AXIS2_PLACEMENT_3D('',#44971,#19721,#19722);
#16314=AXIS2_PLACEMENT_3D('',#44972,#19723,#19724);
#16315=AXIS2_PLACEMENT_3D('',#44973,#19725,#19726);
#16316=AXIS2_PLACEMENT_3D('',#44974,#19727,#19728);
#16317=AXIS2_PLACEMENT_3D('',#44977,#19731,#19732);
#16318=AXIS2_PLACEMENT_3D('',#44979,#19733,#19734);
#16319=AXIS2_PLACEMENT_3D('',#44982,#19736,#19737);
#16320=AXIS2_PLACEMENT_3D('',#44983,#19738,#19739);
#16321=AXIS2_PLACEMENT_3D('',#44989,#19743,#19744);
#16322=AXIS2_PLACEMENT_3D('',#44990,#19745,#19746);
#16323=AXIS2_PLACEMENT_3D('',#44996,#19750,#19751);
#16324=AXIS2_PLACEMENT_3D('',#45002,#19755,#19756);
#16325=AXIS2_PLACEMENT_3D('',#45004,#19758,#19759);
#16326=AXIS2_PLACEMENT_3D('',#45005,#19760,#19761);
#16327=AXIS2_PLACEMENT_3D('',#45007,#19763,#19764);
#16328=AXIS2_PLACEMENT_3D('',#45008,#19765,#19766);
#16329=AXIS2_PLACEMENT_3D('',#45009,#19767,#19768);
#16330=AXIS2_PLACEMENT_3D('',#45012,#19771,#19772);
#16331=AXIS2_PLACEMENT_3D('',#45015,#19773,#19774);
#16332=AXIS2_PLACEMENT_3D('',#45019,#19776,#19777);
#16333=AXIS2_PLACEMENT_3D('',#45021,#19779,#19780);
#16334=AXIS2_PLACEMENT_3D('',#45027,#19784,#19785);
#16335=AXIS2_PLACEMENT_3D('',#45029,#19786,#19787);
#16336=AXIS2_PLACEMENT_3D('',#45037,#19793,#19794);
#16337=AXIS2_PLACEMENT_3D('',#45043,#19798,#19799);
#16338=AXIS2_PLACEMENT_3D('',#45045,#19801,#19802);
#16339=AXIS2_PLACEMENT_3D('',#45048,#19804,#19805);
#16340=AXIS2_PLACEMENT_3D('',#45051,#19808,#19809);
#16341=AXIS2_PLACEMENT_3D('',#45054,#19812,#19813);
#16342=AXIS2_PLACEMENT_3D('',#45056,#19815,#19816);
#16343=AXIS2_PLACEMENT_3D('',#45057,#19817,#19818);
#16344=AXIS2_PLACEMENT_3D('',#45058,#19819,#19820);
#16345=AXIS2_PLACEMENT_3D('',#45061,#19823,#19824);
#16346=AXIS2_PLACEMENT_3D('',#45064,#19827,#19828);
#16347=AXIS2_PLACEMENT_3D('',#45067,#19829,#19830);
#16348=AXIS2_PLACEMENT_3D('',#45071,#19832,#19833);
#16349=AXIS2_PLACEMENT_3D('',#45073,#19835,#19836);
#16350=AXIS2_PLACEMENT_3D('',#45077,#19840,#19841);
#16351=AXIS2_PLACEMENT_3D('',#45081,#19843,#19844);
#16352=AXIS2_PLACEMENT_3D('',#45083,#19846,#19847);
#16353=AXIS2_PLACEMENT_3D('',#45084,#19848,#19849);
#16354=AXIS2_PLACEMENT_3D('',#45088,#19851,#19852);
#16355=AXIS2_PLACEMENT_3D('',#45090,#19854,#19855);
#16356=AXIS2_PLACEMENT_3D('',#45092,#19857,#19858);
#16357=AXIS2_PLACEMENT_3D('',#45093,#19859,#19860);
#16358=AXIS2_PLACEMENT_3D('',#45096,#19863,#19864);
#16359=AXIS2_PLACEMENT_3D('',#45097,#19865,#19866);
#16360=AXIS2_PLACEMENT_3D('',#45098,#19867,#19868);
#16361=AXIS2_PLACEMENT_3D('',#45099,#19869,#19870);
#16362=AXIS2_PLACEMENT_3D('',#45100,#19871,#19872);
#16363=AXIS2_PLACEMENT_3D('',#45101,#19873,#19874);
#16364=AXIS2_PLACEMENT_3D('',#45102,#19875,#19876);
#16365=AXIS2_PLACEMENT_3D('',#45103,#19877,#19878);
#16366=AXIS2_PLACEMENT_3D('',#45112,#19883,#19884);
#16367=AXIS2_PLACEMENT_3D('',#45118,#19888,#19889);
#16368=AXIS2_PLACEMENT_3D('',#45127,#19894,#19895);
#16369=AXIS2_PLACEMENT_3D('',#45129,#19896,#19897);
#16370=AXIS2_PLACEMENT_3D('',#45132,#19899,#19900);
#16371=AXIS2_PLACEMENT_3D('',#45133,#19901,#19902);
#16372=AXIS2_PLACEMENT_3D('',#45139,#19906,#19907);
#16373=AXIS2_PLACEMENT_3D('',#45141,#19908,#19909);
#16374=AXIS2_PLACEMENT_3D('',#45144,#19911,#19912);
#16375=AXIS2_PLACEMENT_3D('',#45145,#19913,#19914);
#16376=AXIS2_PLACEMENT_3D('',#45151,#19918,#19919);
#16377=AXIS2_PLACEMENT_3D('',#45153,#19920,#19921);
#16378=AXIS2_PLACEMENT_3D('',#45156,#19923,#19924);
#16379=AXIS2_PLACEMENT_3D('',#45157,#19925,#19926);
#16380=AXIS2_PLACEMENT_3D('',#45160,#19928,#19929);
#16381=AXIS2_PLACEMENT_3D('',#45161,#19930,#19931);
#16382=AXIS2_PLACEMENT_3D('',#45164,#19933,#19934);
#16383=AXIS2_PLACEMENT_3D('',#45168,#19937,#19938);
#16384=AXIS2_PLACEMENT_3D('',#45170,#19940,#19941);
#16385=AXIS2_PLACEMENT_3D('',#45174,#19944,#19945);
#16386=AXIS2_PLACEMENT_3D('',#45176,#19947,#19948);
#16387=AXIS2_PLACEMENT_3D('',#45177,#19949,#19950);
#16388=AXIS2_PLACEMENT_3D('',#45178,#19951,#19952);
#16389=AXIS2_PLACEMENT_3D('',#45179,#19953,#19954);
#16390=AXIS2_PLACEMENT_3D('',#45196,#19956,#19957);
#16391=AXIS2_PLACEMENT_3D('',#45218,#19959,#19960);
#16392=AXIS2_PLACEMENT_3D('',#45293,#19961,#19962);
#16393=AXIS2_PLACEMENT_3D('',#45296,#19963,#19964);
#16394=AXIS2_PLACEMENT_3D('',#45300,#19966,#19967);
#16395=AXIS2_PLACEMENT_3D('',#45302,#19969,#19970);
#16396=AXIS2_PLACEMENT_3D('',#45305,#19971,#19972);
#16397=AXIS2_PLACEMENT_3D('',#45309,#19974,#19975);
#16398=AXIS2_PLACEMENT_3D('',#45311,#19977,#19978);
#16399=AXIS2_PLACEMENT_3D('',#45314,#19980,#19981);
#16400=AXIS2_PLACEMENT_3D('',#45315,#19982,#19983);
#16401=AXIS2_PLACEMENT_3D('',#45317,#19984,#19985);
#16402=AXIS2_PLACEMENT_3D('',#45320,#19987,#19988);
#16403=AXIS2_PLACEMENT_3D('',#45321,#19989,#19990);
#16404=AXIS2_PLACEMENT_3D('',#45323,#19991,#19992);
#16405=AXIS2_PLACEMENT_3D('',#45325,#19994,#19995);
#16406=AXIS2_PLACEMENT_3D('',#45327,#19996,#19997);
#16407=AXIS2_PLACEMENT_3D('',#45330,#19999,#20000);
#16408=AXIS2_PLACEMENT_3D('',#45331,#20001,#20002);
#16409=AXIS2_PLACEMENT_3D('',#45333,#20003,#20004);
#16410=AXIS2_PLACEMENT_3D('',#45336,#20006,#20007);
#16411=AXIS2_PLACEMENT_3D('',#45337,#20008,#20009);
#16412=AXIS2_PLACEMENT_3D('',#45339,#20010,#20011);
#16413=AXIS2_PLACEMENT_3D('',#45342,#20013,#20014);
#16414=AXIS2_PLACEMENT_3D('',#45343,#20015,#20016);
#16415=AXIS2_PLACEMENT_3D('',#45345,#20017,#20018);
#16416=AXIS2_PLACEMENT_3D('',#45348,#20020,#20021);
#16417=AXIS2_PLACEMENT_3D('',#45349,#20022,#20023);
#16418=AXIS2_PLACEMENT_3D('',#45352,#20024,#20025);
#16419=AXIS2_PLACEMENT_3D('',#45356,#20027,#20028);
#16420=AXIS2_PLACEMENT_3D('',#45358,#20030,#20031);
#16421=AXIS2_PLACEMENT_3D('',#45360,#20032,#20033);
#16422=AXIS2_PLACEMENT_3D('',#45363,#20035,#20036);
#16423=AXIS2_PLACEMENT_3D('',#45364,#20037,#20038);
#16424=AXIS2_PLACEMENT_3D('',#45366,#20039,#20040);
#16425=AXIS2_PLACEMENT_3D('',#45369,#20042,#20043);
#16426=AXIS2_PLACEMENT_3D('',#45370,#20044,#20045);
#16427=AXIS2_PLACEMENT_3D('',#45373,#20047,#20048);
#16428=AXIS2_PLACEMENT_3D('',#45374,#20049,#20050);
#16429=AXIS2_PLACEMENT_3D('',#45376,#20051,#20052);
#16430=AXIS2_PLACEMENT_3D('',#45379,#20054,#20055);
#16431=AXIS2_PLACEMENT_3D('',#45380,#20056,#20057);
#16432=AXIS2_PLACEMENT_3D('',#45381,#20058,#20059);
#16433=AXIS2_PLACEMENT_3D('',#45382,#20060,#20061);
#16434=AXIS2_PLACEMENT_3D('',#45383,#20062,#20063);
#16435=AXIS2_PLACEMENT_3D('',#45389,#20067,#20068);
#16436=AXIS2_PLACEMENT_3D('',#45398,#20073,#20074);
#16437=AXIS2_PLACEMENT_3D('',#45404,#20078,#20079);
#16438=AXIS2_PLACEMENT_3D('',#45412,#20084,#20085);
#16439=AXIS2_PLACEMENT_3D('',#45418,#20089,#20090);
#16440=AXIS2_PLACEMENT_3D('',#45424,#20094,#20095);
#16441=AXIS2_PLACEMENT_3D('',#45426,#20096,#20097);
#16442=AXIS2_PLACEMENT_3D('',#45428,#20098,#20099);
#16443=AXIS2_PLACEMENT_3D('',#45430,#20101,#20102);
#16444=AXIS2_PLACEMENT_3D('',#45436,#20106,#20107);
#16445=AXIS2_PLACEMENT_3D('',#45438,#20108,#20109);
#16446=AXIS2_PLACEMENT_3D('',#45440,#20110,#20111);
#16447=AXIS2_PLACEMENT_3D('',#45442,#20113,#20114);
#16448=AXIS2_PLACEMENT_3D('',#45448,#20118,#20119);
#16449=AXIS2_PLACEMENT_3D('',#45452,#20121,#20122);
#16450=AXIS2_PLACEMENT_3D('',#45453,#20123,#20124);
#16451=AXIS2_PLACEMENT_3D('',#45454,#20125,#20126);
#16452=AXIS2_PLACEMENT_3D('',#45457,#20127,#20128);
#16453=AXIS2_PLACEMENT_3D('',#45461,#20130,#20131);
#16454=AXIS2_PLACEMENT_3D('',#45463,#20133,#20134);
#16455=AXIS2_PLACEMENT_3D('',#45472,#20139,#20140);
#16456=AXIS2_PLACEMENT_3D('',#45480,#20145,#20146);
#16457=AXIS2_PLACEMENT_3D('',#45484,#20149,#20150);
#16458=AXIS2_PLACEMENT_3D('',#45488,#20154,#20155);
#16459=AXIS2_PLACEMENT_3D('',#45497,#20161,#20162);
#16460=AXIS2_PLACEMENT_3D('',#45505,#20167,#20168);
#16461=AXIS2_PLACEMENT_3D('',#45506,#20169,#20170);
#16462=AXIS2_PLACEMENT_3D('',#45507,#20171,#20172);
#16463=AXIS2_PLACEMENT_3D('',#45516,#20177,#20178);
#16464=AXIS2_PLACEMENT_3D('',#45517,#20179,#20180);
#16465=AXIS2_PLACEMENT_3D('',#45519,#20181,#20182);
#16466=AXIS2_PLACEMENT_3D('',#45522,#20184,#20185);
#16467=AXIS2_PLACEMENT_3D('',#45523,#20186,#20187);
#16468=AXIS2_PLACEMENT_3D('',#45525,#20188,#20189);
#16469=AXIS2_PLACEMENT_3D('',#45526,#20190,#20191);
#16470=AXIS2_PLACEMENT_3D('',#45528,#20193,#20194);
#16471=AXIS2_PLACEMENT_3D('',#45532,#20197,#20198);
#16472=AXIS2_PLACEMENT_3D('',#45539,#20203,#20204);
#16473=AXIS2_PLACEMENT_3D('',#45543,#20207,#20208);
#16474=AXIS2_PLACEMENT_3D('',#45545,#20210,#20211);
#16475=AXIS2_PLACEMENT_3D('',#45548,#20213,#20214);
#16476=AXIS2_PLACEMENT_3D('',#45549,#20215,#20216);
#16477=AXIS2_PLACEMENT_3D('',#45550,#20217,#20218);
#16478=AXIS2_PLACEMENT_3D('',#45552,#20220,#20221);
#16479=AXIS2_PLACEMENT_3D('',#45553,#20222,#20223);
#16480=AXIS2_PLACEMENT_3D('',#45556,#20226,#20227);
#16481=AXIS2_PLACEMENT_3D('',#45557,#20228,#20229);
#16482=AXIS2_PLACEMENT_3D('',#45560,#20231,#20232);
#16483=AXIS2_PLACEMENT_3D('',#45561,#20233,#20234);
#16484=AXIS2_PLACEMENT_3D('',#45563,#20236,#20237);
#16485=AXIS2_PLACEMENT_3D('',#45565,#20239,#20240);
#16486=AXIS2_PLACEMENT_3D('',#45566,#20241,#20242);
#16487=AXIS2_PLACEMENT_3D('',#45567,#20243,#20244);
#16488=AXIS2_PLACEMENT_3D('',#45568,#20245,#20246);
#16489=AXIS2_PLACEMENT_3D('',#45569,#20247,#20248);
#16490=AXIS2_PLACEMENT_3D('',#45585,#20249,#20250);
#16491=AXIS2_PLACEMENT_3D('',#45587,#20251,#20252);
#16492=AXIS2_PLACEMENT_3D('',#45589,#20253,#20254);
#16493=AXIS2_PLACEMENT_3D('',#45591,#20255,#20256);
#16494=AXIS2_PLACEMENT_3D('',#45592,#20257,#20258);
#16495=AXIS2_PLACEMENT_3D('',#45593,#20259,#20260);
#16496=AXIS2_PLACEMENT_3D('',#45595,#20261,#20262);
#16497=AXIS2_PLACEMENT_3D('',#45598,#20264,#20265);
#16498=AXIS2_PLACEMENT_3D('',#45599,#20266,#20267);
#16499=AXIS2_PLACEMENT_3D('',#46088,#20269,#20270);
#16500=AXIS2_PLACEMENT_3D('',#46099,#20271,#20272);
#16501=AXIS2_PLACEMENT_3D('',#46111,#20273,#20274);
#16502=AXIS2_PLACEMENT_3D('',#46340,#20275,#20276);
#16503=AXIS2_PLACEMENT_3D('',#46343,#20277,#20278);
#16504=AXIS2_PLACEMENT_3D('',#46364,#20279,#20280);
#16505=AXIS2_PLACEMENT_3D('',#46366,#20281,#20282);
#16506=AXIS2_PLACEMENT_3D('',#46370,#20284,#20285);
#16507=AXIS2_PLACEMENT_3D('',#46656,#20286,#20287);
#16508=AXIS2_PLACEMENT_3D('',#46681,#20288,#20289);
#16509=AXIS2_PLACEMENT_3D('',#47026,#20290,#20291);
#16510=AXIS2_PLACEMENT_3D('',#47027,#20292,#20293);
#16511=AXIS2_PLACEMENT_3D('',#47029,#20294,#20295);
#16512=AXIS2_PLACEMENT_3D('',#47030,#20296,#20297);
#16513=AXIS2_PLACEMENT_3D('',#47031,#20298,#20299);
#16514=AXIS2_PLACEMENT_3D('',#47034,#20300,#20301);
#16515=AXIS2_PLACEMENT_3D('',#47038,#20303,#20304);
#16516=AXIS2_PLACEMENT_3D('',#48229,#20305,#20306);
#16517=AXIS2_PLACEMENT_3D('',#48367,#20307,#20308);
#16518=AXIS2_PLACEMENT_3D('',#48371,#20310,#20311);
#16519=AXIS2_PLACEMENT_3D('',#48398,#20312,#20313);
#16520=AXIS2_PLACEMENT_3D('',#48400,#20314,#20315);
#16521=AXIS2_PLACEMENT_3D('',#48566,#20316,#20317);
#16522=AXIS2_PLACEMENT_3D('',#48905,#20318,#20319);
#16523=AXIS2_PLACEMENT_3D('',#48907,#20320,#20321);
#16524=AXIS2_PLACEMENT_3D('',#48911,#20323,#20324);
#16525=AXIS2_PLACEMENT_3D('',#49046,#20326,#20327);
#16526=AXIS2_PLACEMENT_3D('',#49470,#20328,#20329);
#16527=AXIS2_PLACEMENT_3D('',#50107,#20330,#20331);
#16528=AXIS2_PLACEMENT_3D('',#50109,#20332,#20333);
#16529=AXIS2_PLACEMENT_3D('',#50110,#20334,#20335);
#16530=AXIS2_PLACEMENT_3D('',#50111,#20336,#20337);
#16531=AXIS2_PLACEMENT_3D('',#50242,#20339,#20340);
#16532=AXIS2_PLACEMENT_3D('',#50702,#20342,#20343);
#16533=AXIS2_PLACEMENT_3D('',#50705,#20344,#20345);
#16534=AXIS2_PLACEMENT_3D('',#50707,#20346,#20347);
#16535=AXIS2_PLACEMENT_3D('',#50709,#20348,#20349);
#16536=AXIS2_PLACEMENT_3D('',#50710,#20350,#20351);
#16537=AXIS2_PLACEMENT_3D('',#50711,#20352,#20353);
#16538=AXIS2_PLACEMENT_3D('',#50713,#20354,#20355);
#16539=AXIS2_PLACEMENT_3D('',#50714,#20356,#20357);
#16540=AXIS2_PLACEMENT_3D('',#51502,#20358,#20359);
#16541=AXIS2_PLACEMENT_3D('',#51504,#20360,#20361);
#16542=AXIS2_PLACEMENT_3D('',#51625,#20362,#20363);
#16543=AXIS2_PLACEMENT_3D('',#51626,#20364,#20365);
#16544=AXIS2_PLACEMENT_3D('',#51641,#20366,#20367);
#16545=AXIS2_PLACEMENT_3D('',#51642,#20368,#20369);
#16546=AXIS2_PLACEMENT_3D('',#51643,#20370,#20371);
#16547=AXIS2_PLACEMENT_3D('',#51645,#20372,#20373);
#16548=AXIS2_PLACEMENT_3D('',#51774,#20375,#20376);
#16549=AXIS2_PLACEMENT_3D('',#51775,#20377,#20378);
#16550=AXIS2_PLACEMENT_3D('',#52121,#20380,#20381);
#16551=AXIS2_PLACEMENT_3D('',#52123,#20383,#20384);
#16552=AXIS2_PLACEMENT_3D('',#52133,#20385,#20386);
#16553=AXIS2_PLACEMENT_3D('',#52135,#20387,#20388);
#16554=AXIS2_PLACEMENT_3D('',#52136,#20389,#20390);
#16555=AXIS2_PLACEMENT_3D('',#52137,#20391,#20392);
#16556=AXIS2_PLACEMENT_3D('',#52139,#20393,#20394);
#16557=AXIS2_PLACEMENT_3D('',#52142,#20396,#20397);
#16558=AXIS2_PLACEMENT_3D('',#53020,#20398,#20399);
#16559=AXIS2_PLACEMENT_3D('',#53420,#20400,#20401);
#16560=AXIS2_PLACEMENT_3D('',#53421,#20402,#20403);
#16561=AXIS2_PLACEMENT_3D('',#53422,#20404,#20405);
#16562=AXIS2_PLACEMENT_3D('',#53425,#20406,#20407);
#16563=AXIS2_PLACEMENT_3D('',#53427,#20408,#20409);
#16564=AXIS2_PLACEMENT_3D('',#53429,#20410,#20411);
#16565=AXIS2_PLACEMENT_3D('',#53430,#20412,#20413);
#16566=AXIS2_PLACEMENT_3D('',#53431,#20414,#20415);
#16567=AXIS2_PLACEMENT_3D('',#53434,#20416,#20417);
#16568=AXIS2_PLACEMENT_3D('',#53460,#20419,#20420);
#16569=AXIS2_PLACEMENT_3D('',#53484,#20422,#20423);
#16570=AXIS2_PLACEMENT_3D('',#53488,#20425,#20426);
#16571=AXIS2_PLACEMENT_3D('',#53490,#20428,#20429);
#16572=AXIS2_PLACEMENT_3D('',#53492,#20431,#20432);
#16573=AXIS2_PLACEMENT_3D('',#53567,#20433,#20434);
#16574=AXIS2_PLACEMENT_3D('',#53685,#20435,#20436);
#16575=AXIS2_PLACEMENT_3D('',#53710,#20438,#20439);
#16576=AXIS2_PLACEMENT_3D('',#53834,#20441,#20442);
#16577=AXIS2_PLACEMENT_3D('',#53837,#20443,#20444);
#16578=AXIS2_PLACEMENT_3D('',#54036,#20445,#20446);
#16579=AXIS2_PLACEMENT_3D('',#54037,#20447,#20448);
#16580=AXIS2_PLACEMENT_3D('',#54039,#20449,#20450);
#16581=AXIS2_PLACEMENT_3D('',#54065,#20452,#20453);
#16582=AXIS2_PLACEMENT_3D('',#54499,#20454,#20455);
#16583=AXIS2_PLACEMENT_3D('',#54502,#20456,#20457);
#16584=AXIS2_PLACEMENT_3D('',#54504,#20458,#20459);
#16585=AXIS2_PLACEMENT_3D('',#54505,#20460,#20461);
#16586=AXIS2_PLACEMENT_3D('',#54508,#20463,#20464);
#16587=AXIS2_PLACEMENT_3D('',#54509,#20465,#20466);
#16588=AXIS2_PLACEMENT_3D('',#54511,#20467,#20468);
#16589=AXIS2_PLACEMENT_3D('',#54514,#20470,#20471);
#16590=AXIS2_PLACEMENT_3D('',#54515,#20472,#20473);
#16591=AXIS2_PLACEMENT_3D('',#54517,#20474,#20475);
#16592=AXIS2_PLACEMENT_3D('',#54520,#20477,#20478);
#16593=AXIS2_PLACEMENT_3D('',#54521,#20479,#20480);
#16594=AXIS2_PLACEMENT_3D('',#54524,#20481,#20482);
#16595=AXIS2_PLACEMENT_3D('',#54526,#20483,#20484);
#16596=AXIS2_PLACEMENT_3D('',#54527,#20485,#20486);
#16597=AXIS2_PLACEMENT_3D('',#54528,#20487,#20488);
#16598=AXIS2_PLACEMENT_3D('',#54531,#20489,#20490);
#16599=AXIS2_PLACEMENT_3D('',#54535,#20492,#20493);
#16600=AXIS2_PLACEMENT_3D('',#54537,#20495,#20496);
#16601=AXIS2_PLACEMENT_3D('',#54539,#20497,#20498);
#16602=AXIS2_PLACEMENT_3D('',#54543,#20500,#20501);
#16603=AXIS2_PLACEMENT_3D('',#54545,#20503,#20504);
#16604=AXIS2_PLACEMENT_3D('',#54547,#20505,#20506);
#16605=AXIS2_PLACEMENT_3D('',#54548,#20507,#20508);
#16606=AXIS2_PLACEMENT_3D('',#54549,#20509,#20510);
#16607=AXIS2_PLACEMENT_3D('',#54552,#20511,#20512);
#16608=AXIS2_PLACEMENT_3D('',#54555,#20515,#20516);
#16609=AXIS2_PLACEMENT_3D('',#54557,#20517,#20518);
#16610=AXIS2_PLACEMENT_3D('',#54558,#20519,#20520);
#16611=AXIS2_PLACEMENT_3D('',#54559,#20521,#20522);
#16612=AXIS2_PLACEMENT_3D('',#54561,#20523,#20524);
#16613=AXIS2_PLACEMENT_3D('',#54564,#20526,#20527);
#16614=AXIS2_PLACEMENT_3D('',#54565,#20528,#20529);
#16615=AXIS2_PLACEMENT_3D('',#54691,#20531,#20532);
#16616=AXIS2_PLACEMENT_3D('',#54693,#20534,#20535);
#16617=AXIS2_PLACEMENT_3D('',#54694,#20536,#20537);
#16618=AXIS2_PLACEMENT_3D('',#54966,#20540,#20541);
#16619=AXIS2_PLACEMENT_3D('',#54968,#20542,#20543);
#16620=AXIS2_PLACEMENT_3D('',#54970,#20545,#20546);
#16621=AXIS2_PLACEMENT_3D('',#54973,#20548,#20549);
#16622=AXIS2_PLACEMENT_3D('',#54974,#20550,#20551);
#16623=AXIS2_PLACEMENT_3D('',#54978,#20553,#20554);
#16624=AXIS2_PLACEMENT_3D('',#54980,#20556,#20557);
#16625=AXIS2_PLACEMENT_3D('',#54982,#20558,#20559);
#16626=AXIS2_PLACEMENT_3D('',#54985,#20561,#20562);
#16627=AXIS2_PLACEMENT_3D('',#54986,#20563,#20564);
#16628=AXIS2_PLACEMENT_3D('',#55000,#20566,#20567);
#16629=AXIS2_PLACEMENT_3D('',#55001,#20568,#20569);
#16630=AXIS2_PLACEMENT_3D('',#55003,#20570,#20571);
#16631=AXIS2_PLACEMENT_3D('',#55006,#20573,#20574);
#16632=AXIS2_PLACEMENT_3D('',#55007,#20575,#20576);
#16633=AXIS2_PLACEMENT_3D('',#55009,#20577,#20578);
#16634=AXIS2_PLACEMENT_3D('',#55010,#20579,#20580);
#16635=AXIS2_PLACEMENT_3D('',#55011,#20581,#20582);
#16636=AXIS2_PLACEMENT_3D('',#55014,#20584,#20585);
#16637=AXIS2_PLACEMENT_3D('',#55015,#20586,#20587);
#16638=AXIS2_PLACEMENT_3D('',#55016,#20588,#20589);
#16639=AXIS2_PLACEMENT_3D('',#55017,#20590,#20591);
#16640=AXIS2_PLACEMENT_3D('',#55019,#20592,#20593);
#16641=AXIS2_PLACEMENT_3D('',#55022,#20595,#20596);
#16642=AXIS2_PLACEMENT_3D('',#55023,#20597,#20598);
#16643=AXIS2_PLACEMENT_3D('',#55025,#20599,#20600);
#16644=AXIS2_PLACEMENT_3D('',#55028,#20602,#20603);
#16645=AXIS2_PLACEMENT_3D('',#55029,#20604,#20605);
#16646=AXIS2_PLACEMENT_3D('',#55030,#20606,#20607);
#16647=AXIS2_PLACEMENT_3D('',#55031,#20608,#20609);
#16648=AXIS2_PLACEMENT_3D('',#55032,#20610,#20611);
#16649=AXIS2_PLACEMENT_3D('',#55103,#20613,#20614);
#16650=AXIS2_PLACEMENT_3D('',#55104,#20615,#20616);
#16651=AXIS2_PLACEMENT_3D('',#55118,#20618,#20619);
#16652=AXIS2_PLACEMENT_3D('',#55119,#20620,#20621);
#16653=AXIS2_PLACEMENT_3D('',#55125,#20625,#20626);
#16654=AXIS2_PLACEMENT_3D('',#55129,#20628,#20629);
#16655=AXIS2_PLACEMENT_3D('',#55130,#20630,#20631);
#16656=AXIS2_PLACEMENT_3D('',#55131,#20632,#20633);
#16657=AXIS2_PLACEMENT_3D('',#55134,#20634,#20635);
#16658=AXIS2_PLACEMENT_3D('',#55139,#20638,#20639);
#16659=AXIS2_PLACEMENT_3D('',#55141,#20641,#20642);
#16660=AXIS2_PLACEMENT_3D('',#55145,#20645,#20646);
#16661=AXIS2_PLACEMENT_3D('',#55148,#20648,#20649);
#16662=AXIS2_PLACEMENT_3D('',#55149,#20650,#20651);
#16663=AXIS2_PLACEMENT_3D('',#55153,#20654,#20655);
#16664=AXIS2_PLACEMENT_3D('',#55156,#20657,#20658);
#16665=AXIS2_PLACEMENT_3D('',#55157,#20659,#20660);
#16666=AXIS2_PLACEMENT_3D('',#55243,#20662,#20663);
#16667=AXIS2_PLACEMENT_3D('',#55353,#20664,#20665);
#16668=AXIS2_PLACEMENT_3D('',#55618,#20666,#20667);
#16669=AXIS2_PLACEMENT_3D('',#55632,#20668,#20669);
#16670=AXIS2_PLACEMENT_3D('',#55776,#20670,#20671);
#16671=AXIS2_PLACEMENT_3D('',#55883,#20672,#20673);
#16672=AXIS2_PLACEMENT_3D('',#55884,#20674,#20675);
#16673=AXIS2_PLACEMENT_3D('',#55885,#20676,#20677);
#16674=AXIS2_PLACEMENT_3D('',#56054,#20678,#20679);
#16675=AXIS2_PLACEMENT_3D('',#56055,#20680,#20681);
#16676=AXIS2_PLACEMENT_3D('',#56056,#20682,#20683);
#16677=AXIS2_PLACEMENT_3D('',#56058,#20684,#20685);
#16678=AXIS2_PLACEMENT_3D('',#56060,#20686,#20687);
#16679=AXIS2_PLACEMENT_3D('',#56061,#20688,#20689);
#16680=AXIS2_PLACEMENT_3D('',#56062,#20690,#20691);
#16681=AXIS2_PLACEMENT_3D('',#56065,#20692,#20693);
#16682=AXIS2_PLACEMENT_3D('',#56067,#20694,#20695);
#16683=AXIS2_PLACEMENT_3D('',#56068,#20696,#20697);
#16684=AXIS2_PLACEMENT_3D('',#56069,#20698,#20699);
#16685=AXIS2_PLACEMENT_3D('',#56072,#20702,#20703);
#16686=AXIS2_PLACEMENT_3D('',#56075,#20704,#20705);
#16687=AXIS2_PLACEMENT_3D('',#56078,#20708,#20709);
#16688=AXIS2_PLACEMENT_3D('',#56081,#20710,#20711);
#16689=AXIS2_PLACEMENT_3D('',#56083,#20712,#20713);
#16690=AXIS2_PLACEMENT_3D('',#56084,#20714,#20715);
#16691=AXIS2_PLACEMENT_3D('',#56085,#20716,#20717);
#16692=AXIS2_PLACEMENT_3D('',#56088,#20718,#20719);
#16693=AXIS2_PLACEMENT_3D('',#56091,#20722,#20723);
#16694=AXIS2_PLACEMENT_3D('',#56094,#20724,#20725);
#16695=AXIS2_PLACEMENT_3D('',#56097,#20728,#20729);
#16696=AXIS2_PLACEMENT_3D('',#56099,#20730,#20731);
#16697=AXIS2_PLACEMENT_3D('',#56100,#20732,#20733);
#16698=AXIS2_PLACEMENT_3D('',#56101,#20734,#20735);
#16699=AXIS2_PLACEMENT_3D('',#56104,#20736,#20737);
#16700=AXIS2_PLACEMENT_3D('',#56107,#20740,#20741);
#16701=AXIS2_PLACEMENT_3D('',#56110,#20742,#20743);
#16702=AXIS2_PLACEMENT_3D('',#56113,#20746,#20747);
#16703=AXIS2_PLACEMENT_3D('',#56115,#20748,#20749);
#16704=AXIS2_PLACEMENT_3D('',#56116,#20750,#20751);
#16705=AXIS2_PLACEMENT_3D('',#56117,#20752,#20753);
#16706=AXIS2_PLACEMENT_3D('',#56120,#20754,#20755);
#16707=AXIS2_PLACEMENT_3D('',#56123,#20758,#20759);
#16708=AXIS2_PLACEMENT_3D('',#56127,#20761,#20762);
#16709=AXIS2_PLACEMENT_3D('',#56129,#20764,#20765);
#16710=AXIS2_PLACEMENT_3D('',#56132,#20766,#20767);
#16711=AXIS2_PLACEMENT_3D('',#56134,#20768,#20769);
#16712=AXIS2_PLACEMENT_3D('',#56135,#20770,#20771);
#16713=AXIS2_PLACEMENT_3D('',#56136,#20772,#20773);
#16714=AXIS2_PLACEMENT_3D('',#56139,#20776,#20777);
#16715=AXIS2_PLACEMENT_3D('',#56142,#20778,#20779);
#16716=AXIS2_PLACEMENT_3D('',#56144,#20781,#20782);
#16717=AXIS2_PLACEMENT_3D('',#56146,#20784,#20785);
#16718=AXIS2_PLACEMENT_3D('',#56148,#20786,#20787);
#16719=AXIS2_PLACEMENT_3D('',#56149,#20788,#20789);
#16720=AXIS2_PLACEMENT_3D('',#56150,#20790,#20791);
#16721=AXIS2_PLACEMENT_3D('',#56153,#20794,#20795);
#16722=AXIS2_PLACEMENT_3D('',#56157,#20797,#20798);
#16723=AXIS2_PLACEMENT_3D('',#56159,#20800,#20801);
#16724=AXIS2_PLACEMENT_3D('',#56161,#20802,#20803);
#16725=AXIS2_PLACEMENT_3D('',#56164,#20806,#20807);
#16726=AXIS2_PLACEMENT_3D('',#56165,#20808,#20809);
#16727=AXIS2_PLACEMENT_3D('',#56166,#20810,#20811);
#16728=AXIS2_PLACEMENT_3D('',#56169,#20814,#20815);
#16729=AXIS2_PLACEMENT_3D('',#56173,#20817,#20818);
#16730=AXIS2_PLACEMENT_3D('',#56175,#20820,#20821);
#16731=AXIS2_PLACEMENT_3D('',#56176,#20822,#20823);
#16732=AXIS2_PLACEMENT_3D('',#56180,#20825,#20826);
#16733=AXIS2_PLACEMENT_3D('',#56182,#20828,#20829);
#16734=AXIS2_PLACEMENT_3D('',#56184,#20830,#20831);
#16735=AXIS2_PLACEMENT_3D('',#56185,#20832,#20833);
#16736=AXIS2_PLACEMENT_3D('',#56186,#20834,#20835);
#16737=AXIS2_PLACEMENT_3D('',#56188,#20836,#20837);
#16738=AXIS2_PLACEMENT_3D('',#56191,#20840,#20841);
#16739=AXIS2_PLACEMENT_3D('',#56194,#20844,#20845);
#16740=AXIS2_PLACEMENT_3D('',#56197,#20848,#20849);
#16741=AXIS2_PLACEMENT_3D('',#56201,#20851,#20852);
#16742=AXIS2_PLACEMENT_3D('',#56203,#20854,#20855);
#16743=AXIS2_PLACEMENT_3D('',#56205,#20857,#20858);
#16744=AXIS2_PLACEMENT_3D('',#56213,#20863,#20864);
#16745=AXIS2_PLACEMENT_3D('',#56214,#20865,#20866);
#16746=AXIS2_PLACEMENT_3D('',#56220,#20870,#20871);
#16747=AXIS2_PLACEMENT_3D('',#56225,#20873,#20874);
#16748=AXIS2_PLACEMENT_3D('',#56229,#20876,#20877);
#16749=AXIS2_PLACEMENT_3D('',#56232,#20880,#20881);
#16750=AXIS2_PLACEMENT_3D('',#56234,#20882,#20883);
#16751=AXIS2_PLACEMENT_3D('',#56236,#20884,#20885);
#16752=AXIS2_PLACEMENT_3D('',#56240,#20888,#20889);
#16753=AXIS2_PLACEMENT_3D('',#56246,#20890,#20891);
#16754=AXIS2_PLACEMENT_3D('',#56247,#20892,#20893);
#16755=AXIS2_PLACEMENT_3D('',#56253,#20897,#20898);
#16756=AXIS2_PLACEMENT_3D('',#56257,#20901,#20902);
#16757=AXIS2_PLACEMENT_3D('',#56258,#20903,#20904);
#16758=AXIS2_PLACEMENT_3D('',#56259,#20905,#20906);
#16759=AXIS2_PLACEMENT_3D('',#56260,#20907,#20908);
#16760=AXIS2_PLACEMENT_3D('',#56261,#20909,#20910);
#16761=AXIS2_PLACEMENT_3D('',#56262,#20911,#20912);
#16762=AXIS2_PLACEMENT_3D('',#56264,#20913,#20914);
#16763=AXIS2_PLACEMENT_3D('',#56266,#20915,#20916);
#16764=AXIS2_PLACEMENT_3D('',#56267,#20917,#20918);
#16765=AXIS2_PLACEMENT_3D('',#56395,#20919,#20920);
#16766=AXIS2_PLACEMENT_3D('',#56397,#20921,#20922);
#16767=AXIS2_PLACEMENT_3D('',#56405,#20924,#20925);
#16768=AXIS2_PLACEMENT_3D('',#56442,#20926,#20927);
#16769=AXIS2_PLACEMENT_3D('',#56443,#20928,#20929);
#16770=AXIS2_PLACEMENT_3D('',#56444,#20930,#20931);
#16771=AXIS2_PLACEMENT_3D('',#56445,#20932,#20933);
#16772=AXIS2_PLACEMENT_3D('',#56447,#20934,#20935);
#16773=AXIS2_PLACEMENT_3D('',#56449,#20936,#20937);
#16774=AXIS2_PLACEMENT_3D('',#56450,#20938,#20939);
#16775=AXIS2_PLACEMENT_3D('',#56451,#20940,#20941);
#16776=AXIS2_PLACEMENT_3D('',#56453,#20943,#20944);
#16777=AXIS2_PLACEMENT_3D('',#56455,#20946,#20947);
#16778=AXIS2_PLACEMENT_3D('',#56457,#20949,#20950);
#16779=AXIS2_PLACEMENT_3D('',#56458,#20951,#20952);
#16780=AXIS2_PLACEMENT_3D('',#56461,#20955,#20956);
#16781=AXIS2_PLACEMENT_3D('',#56462,#20957,#20958);
#16782=AXIS2_PLACEMENT_3D('',#56466,#20960,#20961);
#16783=AXIS2_PLACEMENT_3D('',#56468,#20963,#20964);
#16784=AXIS2_PLACEMENT_3D('',#56471,#20967,#20968);
#16785=AXIS2_PLACEMENT_3D('',#56961,#20969,#20970);
#16786=AXIS2_PLACEMENT_3D('',#57046,#20971,#20972);
#16787=AXIS2_PLACEMENT_3D('',#57273,#20975,#20976);
#16788=AXIS2_PLACEMENT_3D('',#58841,#20977,#20978);
#16789=AXIS2_PLACEMENT_3D('',#58850,#20979,#20980);
#16790=AXIS2_PLACEMENT_3D('',#58851,#20981,#20982);
#16791=AXIS2_PLACEMENT_3D('',#58854,#20985,#20986);
#16792=AXIS2_PLACEMENT_3D('',#58855,#20987,#20988);
#16793=AXIS2_PLACEMENT_3D('',#58858,#20990,#20991);
#16794=AXIS2_PLACEMENT_3D('',#58859,#20992,#20993);
#16795=AXIS2_PLACEMENT_3D('',#58861,#20994,#20995);
#16796=AXIS2_PLACEMENT_3D('',#58992,#20997,#20998);
#16797=AXIS2_PLACEMENT_3D('',#58993,#20999,#21000);
#16798=AXIS2_PLACEMENT_3D('',#58998,#21004,#21005);
#16799=AXIS2_PLACEMENT_3D('',#59004,#21009,#21010);
#16800=AXIS2_PLACEMENT_3D('',#59011,#21014,#21015);
#16801=AXIS2_PLACEMENT_3D('',#59014,#21017,#21018);
#16802=AXIS2_PLACEMENT_3D('',#59015,#21019,#21020);
#16803=AXIS2_PLACEMENT_3D('',#59016,#21021,#21022);
#16804=AXIS2_PLACEMENT_3D('',#59017,#21023,#21024);
#16805=AXIS2_PLACEMENT_3D('',#59023,#21028,#21029);
#16806=AXIS2_PLACEMENT_3D('',#59024,#21030,#21031);
#16807=AXIS2_PLACEMENT_3D('',#59025,#21032,#21033);
#16808=AXIS2_PLACEMENT_3D('',#59027,#21035,#21036);
#16809=AXIS2_PLACEMENT_3D('',#59028,#21037,#21038);
#16810=AXIS2_PLACEMENT_3D('',#59029,#21039,#21040);
#16811=AXIS2_PLACEMENT_3D('',#59033,#21042,#21043);
#16812=AXIS2_PLACEMENT_3D('',#59035,#21045,#21046);
#16813=AXIS2_PLACEMENT_3D('',#59036,#21047,#21048);
#16814=AXIS2_PLACEMENT_3D('',#59041,#21052,#21053);
#16815=AXIS2_PLACEMENT_3D('',#59052,#21056,#21057);
#16816=AXIS2_PLACEMENT_3D('',#59661,#21058,#21059);
#16817=AXIS2_PLACEMENT_3D('',#59662,#21060,#21061);
#16818=AXIS2_PLACEMENT_3D('',#59663,#21062,#21063);
#16819=AXIS2_PLACEMENT_3D('',#59664,#21064,#21065);
#16820=AXIS2_PLACEMENT_3D('',#59673,#21066,#21067);
#16821=AXIS2_PLACEMENT_3D('',#59674,#21068,#21069);
#16822=AXIS2_PLACEMENT_3D('',#59675,#21070,#21071);
#16823=AXIS2_PLACEMENT_3D('',#59770,#21072,#21073);
#16824=AXIS2_PLACEMENT_3D('',#59771,#21074,#21075);
#16825=AXIS2_PLACEMENT_3D('',#60708,#21076,#21077);
#16826=AXIS2_PLACEMENT_3D('',#60709,#21078,#21079);
#16827=AXIS2_PLACEMENT_3D('',#60710,#21080,#21081);
#16828=AXIS2_PLACEMENT_3D('',#60711,#21082,#21083);
#16829=AXIS2_PLACEMENT_3D('',#60726,#21085,#21086);
#16830=AXIS2_PLACEMENT_3D('',#60727,#21087,#21088);
#16831=AXIS2_PLACEMENT_3D('',#60728,#21089,#21090);
#16832=AXIS2_PLACEMENT_3D('',#60729,#21091,#21092);
#16833=AXIS2_PLACEMENT_3D('',#60730,#21093,#21094);
#16834=AXIS2_PLACEMENT_3D('',#60731,#21095,#21096);
#16835=AXIS2_PLACEMENT_3D('',#60732,#21097,#21098);
#16836=AXIS2_PLACEMENT_3D('',#60733,#21099,#21100);
#16837=AXIS2_PLACEMENT_3D('',#60734,#21101,#21102);
#16838=AXIS2_PLACEMENT_3D('',#60735,#21103,#21104);
#16839=AXIS2_PLACEMENT_3D('',#60736,#21105,#21106);
#16840=AXIS2_PLACEMENT_3D('',#60737,#21107,#21108);
#16841=AXIS2_PLACEMENT_3D('',#61909,#21109,#21110);
#16842=AXIS2_PLACEMENT_3D('',#61910,#21111,#21112);
#16843=AXIS2_PLACEMENT_3D('',#62259,#21113,#21114);
#16844=AXIS2_PLACEMENT_3D('',#62296,#21115,#21116);
#16845=AXIS2_PLACEMENT_3D('',#62603,#21117,#21118);
#16846=AXIS2_PLACEMENT_3D('',#62626,#21119,#21120);
#16847=AXIS2_PLACEMENT_3D('',#62627,#21121,#21122);
#16848=AXIS2_PLACEMENT_3D('',#62628,#21123,#21124);
#16849=AXIS2_PLACEMENT_3D('',#62629,#21125,#21126);
#16850=AXIS2_PLACEMENT_3D('',#62631,#21128,#21129);
#16851=AXIS2_PLACEMENT_3D('',#62632,#21130,#21131);
#16852=AXIS2_PLACEMENT_3D('',#62636,#21133,#21134);
#16853=AXIS2_PLACEMENT_3D('',#62638,#21136,#21137);
#16854=AXIS2_PLACEMENT_3D('',#62639,#21138,#21139);
#16855=AXIS2_PLACEMENT_3D('',#62640,#21140,#21141);
#16856=AXIS2_PLACEMENT_3D('',#62641,#21142,#21143);
#16857=AXIS2_PLACEMENT_3D('',#62642,#21144,#21145);
#16858=AXIS2_PLACEMENT_3D('',#62644,#21146,#21147);
#16859=AXIS2_PLACEMENT_3D('',#62647,#21149,#21150);
#16860=AXIS2_PLACEMENT_3D('',#62648,#21151,#21152);
#16861=AXIS2_PLACEMENT_3D('',#62650,#21153,#21154);
#16862=AXIS2_PLACEMENT_3D('',#62653,#21156,#21157);
#16863=AXIS2_PLACEMENT_3D('',#62654,#21158,#21159);
#16864=AXIS2_PLACEMENT_3D('',#62655,#21160,#21161);
#16865=AXIS2_PLACEMENT_3D('',#62656,#21162,#21163);
#16866=AXIS2_PLACEMENT_3D('',#62657,#21164,#21165);
#16867=AXIS2_PLACEMENT_3D('',#62660,#21166,#21167);
#16868=AXIS2_PLACEMENT_3D('',#62673,#21168,#21169);
#16869=AXIS2_PLACEMENT_3D('',#62684,#21170,#21171);
#16870=AXIS2_PLACEMENT_3D('',#62687,#21172,#21173);
#16871=AXIS2_PLACEMENT_3D('',#62700,#21174,#21175);
#16872=AXIS2_PLACEMENT_3D('',#62711,#21176,#21177);
#16873=AXIS2_PLACEMENT_3D('',#62714,#21178,#21179);
#16874=AXIS2_PLACEMENT_3D('',#62727,#21180,#21181);
#16875=AXIS2_PLACEMENT_3D('',#62738,#21182,#21183);
#16876=AXIS2_PLACEMENT_3D('',#62741,#21184,#21185);
#16877=AXIS2_PLACEMENT_3D('',#62754,#21186,#21187);
#16878=AXIS2_PLACEMENT_3D('',#62765,#21188,#21189);
#16879=AXIS2_PLACEMENT_3D('',#62768,#21192,#21193);
#16880=AXIS2_PLACEMENT_3D('',#62771,#21196,#21197);
#16881=AXIS2_PLACEMENT_3D('',#62774,#21200,#21201);
#16882=AXIS2_PLACEMENT_3D('',#62777,#21204,#21205);
#16883=AXIS2_PLACEMENT_3D('',#62778,#21206,#21207);
#16884=AXIS2_PLACEMENT_3D('',#62779,#21208,#21209);
#16885=AXIS2_PLACEMENT_3D('',#62780,#21210,#21211);
#16886=AXIS2_PLACEMENT_3D('',#62785,#21213,#21214);
#16887=AXIS2_PLACEMENT_3D('',#62787,#21215,#21216);
#16888=AXIS2_PLACEMENT_3D('',#62789,#21217,#21218);
#16889=AXIS2_PLACEMENT_3D('',#62791,#21219,#21220);
#16890=AXIS2_PLACEMENT_3D('',#62793,#21221,#21222);
#16891=AXIS2_PLACEMENT_3D('',#62794,#21223,#21224);
#16892=AXIS2_PLACEMENT_3D('',#62795,#21225,#21226);
#16893=AXIS2_PLACEMENT_3D('',#62801,#21227,#21228);
#16894=AXIS2_PLACEMENT_3D('',#62802,#21229,#21230);
#16895=AXIS2_PLACEMENT_3D('',#62804,#21231,#21232);
#16896=AXIS2_PLACEMENT_3D('',#62806,#21233,#21234);
#16897=AXIS2_PLACEMENT_3D('',#62808,#21235,#21236);
#16898=AXIS2_PLACEMENT_3D('',#62809,#21237,#21238);
#16899=AXIS2_PLACEMENT_3D('',#62810,#21239,#21240);
#16900=AXIS2_PLACEMENT_3D('',#62813,#21242,#21243);
#16901=AXIS2_PLACEMENT_3D('',#62814,#21244,#21245);
#16902=AXIS2_PLACEMENT_3D('',#62816,#21246,#21247);
#16903=AXIS2_PLACEMENT_3D('',#62818,#21248,#21249);
#16904=AXIS2_PLACEMENT_3D('',#62820,#21250,#21251);
#16905=AXIS2_PLACEMENT_3D('',#62821,#21252,#21253);
#16906=AXIS2_PLACEMENT_3D('',#62822,#21254,#21255);
#16907=AXIS2_PLACEMENT_3D('',#62826,#21257,#21258);
#16908=AXIS2_PLACEMENT_3D('',#62827,#21259,#21260);
#16909=AXIS2_PLACEMENT_3D('',#62828,#21261,#21262);
#16910=AXIS2_PLACEMENT_3D('',#62830,#21263,#21264);
#16911=AXIS2_PLACEMENT_3D('',#62832,#21265,#21266);
#16912=AXIS2_PLACEMENT_3D('',#62833,#21267,#21268);
#16913=AXIS2_PLACEMENT_3D('',#62834,#21269,#21270);
#16914=AXIS2_PLACEMENT_3D('',#62837,#21272,#21273);
#16915=AXIS2_PLACEMENT_3D('',#62838,#21274,#21275);
#16916=AXIS2_PLACEMENT_3D('',#62840,#21277,#21278);
#16917=AXIS2_PLACEMENT_3D('',#62841,#21279,#21280);
#16918=AXIS2_PLACEMENT_3D('',#62847,#21281,#21282);
#16919=AXIS2_PLACEMENT_3D('',#62848,#21283,#21284);
#16920=AXIS2_PLACEMENT_3D('',#62854,#21285,#21286);
#16921=AXIS2_PLACEMENT_3D('',#62855,#21287,#21288);
#16922=AXIS2_PLACEMENT_3D('',#62861,#21289,#21290);
#16923=AXIS2_PLACEMENT_3D('',#62862,#21291,#21292);
#16924=AXIS2_PLACEMENT_3D('',#62866,#21295,#21296);
#16925=AXIS2_PLACEMENT_3D('',#62872,#21297,#21298);
#16926=AXIS2_PLACEMENT_3D('',#62873,#21299,#21300);
#16927=AXIS2_PLACEMENT_3D('',#62879,#21301,#21302);
#16928=AXIS2_PLACEMENT_3D('',#62880,#21303,#21304);
#16929=AXIS2_PLACEMENT_3D('',#62884,#21307,#21308);
#16930=AXIS2_PLACEMENT_3D('',#62888,#21311,#21312);
#16931=AXIS2_PLACEMENT_3D('',#62889,#21313,#21314);
#16932=AXIS2_PLACEMENT_3D('',#62896,#21319,#21320);
#16933=AXIS2_PLACEMENT_3D('',#62901,#21324,#21325);
#16934=AXIS2_PLACEMENT_3D('',#62908,#21330,#21331);
#16935=AXIS2_PLACEMENT_3D('',#62916,#21337,#21338);
#16936=AXIS2_PLACEMENT_3D('',#62923,#21343,#21344);
#16937=AXIS2_PLACEMENT_3D('',#62928,#21349,#21350);
#16938=AXIS2_PLACEMENT_3D('',#62929,#21351,#21352);
#16939=AXIS2_PLACEMENT_3D('',#62930,#21353,#21354);
#16940=AXIS2_PLACEMENT_3D('',#62931,#21355,#21356);
#16941=AXIS2_PLACEMENT_3D('',#62932,#21357,#21358);
#16942=AXIS2_PLACEMENT_3D('',#62933,#21359,#21360);
#16943=AXIS2_PLACEMENT_3D('',#62934,#21361,#21362);
#16944=AXIS2_PLACEMENT_3D('',#62935,#21363,#21364);
#16945=AXIS2_PLACEMENT_3D('',#62936,#21365,#21366);
#16946=AXIS2_PLACEMENT_3D('',#62937,#21367,#21368);
#16947=AXIS2_PLACEMENT_3D('',#62938,#21369,#21370);
#16948=AXIS2_PLACEMENT_3D('',#62939,#21371,#21372);
#16949=AXIS2_PLACEMENT_3D('',#62940,#21373,#21374);
#16950=AXIS2_PLACEMENT_3D('',#62941,#21375,#21376);
#16951=AXIS2_PLACEMENT_3D('',#62942,#21377,#21378);
#16952=AXIS2_PLACEMENT_3D('',#62943,#21379,#21380);
#16953=AXIS2_PLACEMENT_3D('',#62944,#21381,#21382);
#16954=AXIS2_PLACEMENT_3D('',#62945,#21383,#21384);
#16955=AXIS2_PLACEMENT_3D('',#62946,#21385,#21386);
#16956=DIRECTION('axis',(0.,0.,1.));
#16957=DIRECTION('refdir',(1.,0.,0.));
#16958=DIRECTION('axis',(0.,0.,1.));
#16959=DIRECTION('refdir',(1.,0.,0.));
#16960=DIRECTION('center_axis',(-0.430981504924197,-0.768119965562791,0.473546894105632));
#16961=DIRECTION('ref_axis',(-0.513559013416071,0.640299002836773,0.571204277562193));
#16962=DIRECTION('center_axis',(0.430981504924197,0.768119965562791,-0.473546894105632));
#16963=DIRECTION('ref_axis',(0.51355901341607,-0.640299002836773,-0.571204277562193));
#16964=DIRECTION('center_axis',(-0.741965014102678,0.00298420341975994,
-0.670431959543668));
#16965=DIRECTION('ref_axis',(0.51355901341607,-0.640299002836773,-0.571204277562193));
#16966=DIRECTION('center_axis',(-0.430981504924197,-0.768119965562791,0.473546894105632));
#16967=DIRECTION('ref_axis',(-0.51355901341607,0.640299002836773,0.571204277562193));
#16968=DIRECTION('center_axis',(0.430981504924197,0.768119965562791,-0.473546894105632));
#16969=DIRECTION('ref_axis',(-0.51355901341607,0.640299002836773,0.571204277562193));
#16970=DIRECTION('',(-0.430981504924197,-0.768119965562791,0.473546894105632));
#16971=DIRECTION('center_axis',(0.430981504924197,0.768119965562791,-0.473546894105632));
#16972=DIRECTION('ref_axis',(0.51355901341607,-0.640299002836773,-0.571204277562193));
#16973=DIRECTION('center_axis',(0.430981504924197,0.768119965562791,-0.473546894105632));
#16974=DIRECTION('ref_axis',(-0.51355901341607,0.640299002836773,0.571204277562193));
#16975=DIRECTION('center_axis',(-0.430981504924197,-0.768119965562791,0.473546894105632));
#16976=DIRECTION('ref_axis',(-0.51355901341607,0.640299002836773,0.571204277562193));
#16977=DIRECTION('',(-0.430981504924197,-0.768119965562791,0.473546894105632));
#16978=DIRECTION('center_axis',(0.430981504924197,0.768119965562791,-0.473546894105632));
#16979=DIRECTION('ref_axis',(-0.51355901341607,0.640299002836773,0.571204277562193));
#16980=DIRECTION('center_axis',(0.430981504924197,0.768119965562791,-0.473546894105632));
#16981=DIRECTION('ref_axis',(-0.51355901341607,0.640299002836773,0.571204277562193));
#16982=DIRECTION('',(0.430981504924197,0.768119965562791,-0.473546894105632));
#16983=DIRECTION('center_axis',(-0.430981504924197,-0.768119965562791,0.473546894105632));
#16984=DIRECTION('ref_axis',(0.51355901341607,-0.640299002836773,-0.571204277562193));
#16985=DIRECTION('center_axis',(0.741965014102678,-0.00298420341976004,
0.670431959543668));
#16986=DIRECTION('ref_axis',(0.51355901341607,-0.640299002836774,-0.571204277562193));
#16987=DIRECTION('center_axis',(0.741965014102678,-0.00298420341976,0.670431959543668));
#16988=DIRECTION('ref_axis',(0.51355901341607,-0.640299002836774,-0.571204277562193));
#16989=DIRECTION('',(0.741965014102678,-0.00298420341976004,0.670431959543668));
#16990=DIRECTION('center_axis',(0.741965014102678,-0.00298420341976,0.670431959543668));
#16991=DIRECTION('ref_axis',(0.51355901341607,-0.640299002836774,-0.571204277562193));
#16992=DIRECTION('center_axis',(0.430981504924197,0.768119965562791,-0.473546894105632));
#16993=DIRECTION('ref_axis',(0.51355901341607,-0.640299002836773,-0.571204277562193));
#16994=DIRECTION('center_axis',(-0.430981504924197,-0.768119965562791,0.473546894105632));
#16995=DIRECTION('ref_axis',(-0.51355901341607,0.640299002836773,0.571204277562193));
#16996=DIRECTION('',(-0.307737294542031,-0.889938771903478,0.336610665028428));
#16997=DIRECTION('center_axis',(-0.430981504924197,-0.768119965562791,0.473546894105632));
#16998=DIRECTION('ref_axis',(-0.51355901341607,0.640299002836773,0.571204277562193));
#16999=DIRECTION('center_axis',(-0.430981504924197,-0.768119965562791,0.473546894105632));
#17000=DIRECTION('ref_axis',(-0.51355901341607,0.640299002836773,0.571204277562193));
#17001=DIRECTION('center_axis',(-0.430981504924197,-0.768119965562791,0.473546894105632));
#17002=DIRECTION('ref_axis',(0.51355901341607,-0.640299002836773,-0.571204277562193));
#17003=DIRECTION('center_axis',(0.430981504924197,0.768119965562791,-0.473546894105632));
#17004=DIRECTION('ref_axis',(-0.51355901341607,0.640299002836773,0.571204277562193));
#17005=DIRECTION('',(0.430981504924197,0.768119965562791,-0.473546894105632));
#17006=DIRECTION('center_axis',(0.430981504924197,0.768119965562791,-0.473546894105632));
#17007=DIRECTION('ref_axis',(-0.51355901341607,0.640299002836773,0.571204277562193));
#17008=DIRECTION('',(0.430981504924197,0.768119965562791,-0.473546894105632));
#17009=DIRECTION('center_axis',(-0.430981504924197,-0.768119965562791,0.473546894105632));
#17010=DIRECTION('ref_axis',(0.741965014102678,-0.00298420341976045,0.670431959543668));
#17011=DIRECTION('center_axis',(0.829398437573064,0.541032685939668,0.139218764885589));
#17012=DIRECTION('ref_axis',(0.219898548181541,-0.545252986894079,0.808915204944706));
#17013=DIRECTION('center_axis',(0.219898548176702,-0.54525298688807,0.808915204950072));
#17014=DIRECTION('ref_axis',(-0.541205761680708,0.621711011172037,0.566190552827446));
#17015=DIRECTION('center_axis',(0.430981504924197,0.768119965562791,-0.473546894105632));
#17016=DIRECTION('ref_axis',(0.51355901341607,-0.640299002836773,-0.571204277562193));
#17017=DIRECTION('center_axis',(0.219898548178344,-0.545252986890155,0.80891520494822));
#17018=DIRECTION('ref_axis',(0.513561985737025,-0.64029706392645,-0.571203778640348));
#17019=DIRECTION('center_axis',(0.829398437573076,0.541032685939656,0.139218764885566));
#17020=DIRECTION('ref_axis',(0.219898548177576,-0.545252986889121,0.808915204949126));
#17021=DIRECTION('center_axis',(-0.741965014102678,0.00298420341976004,
-0.670431959543668));
#17022=DIRECTION('ref_axis',(-0.51355901341607,0.640299002836773,0.571204277562193));
#17023=DIRECTION('center_axis',(0.741965014102678,-0.00298420341976004,
0.670431959543668));
#17024=DIRECTION('ref_axis',(-0.51355901341607,0.640299002836773,0.571204277562193));
#17025=DIRECTION('',(0.741965014102678,-0.00298420341976004,0.670431959543668));
#17026=DIRECTION('center_axis',(-0.741965014102678,0.00298420341976,-0.670431959543668));
#17027=DIRECTION('ref_axis',(-0.430981504924197,-0.768119965562791,0.473546894105632));
#17028=DIRECTION('center_axis',(-0.741965014102678,0.00298420341976,-0.670431959543668));
#17029=DIRECTION('ref_axis',(0.430981504924197,0.768119965562791,-0.473546894105632));
#17030=DIRECTION('center_axis',(-0.741965014102678,0.00298420341976,-0.670431959543668));
#17031=DIRECTION('ref_axis',(-0.51355901341607,0.640299002836773,0.571204277562193));
#17032=DIRECTION('',(0.741965014102678,-0.00298420341976,0.670431959543668));
#17033=DIRECTION('center_axis',(0.219900418845594,-0.545253383109838,0.808914429342689));
#17034=DIRECTION('ref_axis',(0.829406037148494,0.541023543918342,0.139209017192382));
#17035=DIRECTION('center_axis',(0.219898716470999,-0.545251260610337,0.808916322803073));
#17036=DIRECTION('ref_axis',(0.829390297200403,0.541043168290232,0.139226523896475));
#17037=DIRECTION('center_axis',(-0.741965014102678,0.00298420341976004,
-0.670431959543668));
#17038=DIRECTION('ref_axis',(-0.51355901341607,0.640299002836773,0.571204277562193));
#17039=DIRECTION('center_axis',(0.741965014102678,-0.00298420341976004,
0.670431959543668));
#17040=DIRECTION('ref_axis',(-0.51355901341607,0.640299002836773,0.571204277562193));
#17041=DIRECTION('',(0.741965014102678,-0.00298420341976004,0.670431959543668));
#17042=DIRECTION('center_axis',(0.741965014102678,-0.00298420341976004,
0.670431959543668));
#17043=DIRECTION('ref_axis',(-0.51355901341607,0.640299002836773,0.571204277562193));
#17044=DIRECTION('center_axis',(0.741965014102678,-0.00298420341976004,
0.670431959543668));
#17045=DIRECTION('ref_axis',(-0.51355901341607,0.640299002836773,0.571204277562193));
#17046=DIRECTION('',(-0.902360417214314,0.367323754862617,-0.225430558173548));
#17047=DIRECTION('center_axis',(0.741965014102678,-0.00298420341976004,
0.670431959543668));
#17048=DIRECTION('ref_axis',(-0.51355901341607,0.640299002836773,0.571204277562193));
#17049=DIRECTION('center_axis',(-0.430981504924197,-0.768119965562791,0.473546894105632));
#17050=DIRECTION('ref_axis',(0.513559013416073,-0.640299002836773,-0.57120427756219));
#17051=DIRECTION('center_axis',(-0.430981504924197,-0.768119965562791,0.473546894105632));
#17052=DIRECTION('ref_axis',(-0.513559013416073,0.640299002836773,0.57120427756219));
#17053=DIRECTION('',(-0.430981504924197,-0.768119965562791,0.473546894105632));
#17054=DIRECTION('center_axis',(-0.430981504924197,-0.768119965562791,0.473546894105632));
#17055=DIRECTION('ref_axis',(-0.513559013416073,0.640299002836773,0.57120427756219));
#17056=DIRECTION('center_axis',(-0.430981504924197,-0.768119965562791,0.473546894105632));
#17057=DIRECTION('ref_axis',(0.513559013416073,-0.640299002836773,-0.57120427756219));
#17058=DIRECTION('center_axis',(0.430981504924197,0.768119965562791,-0.473546894105632));
#17059=DIRECTION('ref_axis',(-0.513559013416073,0.640299002836773,0.57120427756219));
#17060=DIRECTION('',(-0.430981504924197,-0.768119965562791,0.473546894105632));
#17061=DIRECTION('center_axis',(0.430981504924197,0.768119965562791,-0.473546894105632));
#17062=DIRECTION('ref_axis',(-0.513559013416073,0.640299002836773,0.57120427756219));
#17063=DIRECTION('center_axis',(0.430981504924197,0.768119965562791,-0.473546894105632));
#17064=DIRECTION('ref_axis',(-0.51355901341607,0.640299002836773,0.571204277562193));
#17065=DIRECTION('center_axis',(-0.430981504924197,-0.768119965562791,0.473546894105632));
#17066=DIRECTION('ref_axis',(-0.51355901341607,0.640299002836773,0.571204277562193));
#17067=DIRECTION('',(0.430981504924197,0.768119965562791,-0.473546894105632));
#17068=DIRECTION('center_axis',(-0.430981504924197,-0.768119965562791,0.473546894105632));
#17069=DIRECTION('ref_axis',(-0.51355901341607,0.640299002836773,0.571204277562193));
#17070=DIRECTION('center_axis',(-0.430981504924197,-0.768119965562791,0.473546894105632));
#17071=DIRECTION('ref_axis',(-0.51355901341607,0.640299002836774,0.571204277562193));
#17072=DIRECTION('center_axis',(-0.430981504924197,-0.768119965562791,0.473546894105632));
#17073=DIRECTION('ref_axis',(-0.51355901341607,0.640299002836773,0.571204277562193));
#17074=DIRECTION('center_axis',(0.741965014102678,-0.00298420341976022,
0.670431959543668));
#17075=DIRECTION('ref_axis',(0.51355901341607,-0.640299002836773,-0.571204277562193));
#17076=DIRECTION('center_axis',(-0.430981504924197,-0.768119965562791,0.473546894105632));
#17077=DIRECTION('ref_axis',(-0.51355901341607,0.640299002836773,0.571204277562193));
#17078=DIRECTION('center_axis',(0.430981504924197,0.768119965562791,-0.473546894105632));
#17079=DIRECTION('ref_axis',(-0.51355901341607,0.640299002836773,0.571204277562193));
#17080=DIRECTION('center_axis',(-0.430981504924197,-0.768119965562791,0.473546894105632));
#17081=DIRECTION('ref_axis',(-0.51355901341607,0.640299002836773,0.571204277562193));
#17082=DIRECTION('',(-0.430981504924197,-0.768119965562791,0.473546894105632));
#17083=DIRECTION('center_axis',(-0.430981504924197,-0.768119965562791,0.473546894105632));
#17084=DIRECTION('ref_axis',(-0.51355901341607,0.640299002836773,0.571204277562193));
#17085=DIRECTION('center_axis',(-0.430981504924197,-0.768119965562791,0.473546894105632));
#17086=DIRECTION('ref_axis',(-0.51355901341607,0.640299002836773,0.571204277562193));
#17087=DIRECTION('center_axis',(-0.430981504924197,-0.768119965562791,0.473546894105632));
#17088=DIRECTION('ref_axis',(-0.51355901341607,0.640299002836773,0.571204277562193));
#17089=DIRECTION('',(-0.0583911162280923,0.995902603307094,0.0690541980750679));
#17090=DIRECTION('center_axis',(0.430981504924197,0.768119965562791,-0.473546894105632));
#17091=DIRECTION('ref_axis',(-0.51355901341607,0.640299002836773,0.571204277562193));
#17092=DIRECTION('center_axis',(-0.430981504924197,-0.768119965562791,0.473546894105632));
#17093=DIRECTION('ref_axis',(-0.51355901341607,0.640299002836773,0.571204277562193));
#17094=DIRECTION('',(0.430981504924197,0.768119965562791,-0.473546894105632));
#17095=DIRECTION('center_axis',(-0.430981504924197,-0.768119965562791,0.473546894105632));
#17096=DIRECTION('ref_axis',(-0.51355901341607,0.640299002836773,0.571204277562193));
#17097=DIRECTION('center_axis',(-0.430981504924197,-0.768119965562791,0.473546894105632));
#17098=DIRECTION('ref_axis',(-0.51355901341607,0.640299002836773,0.571204277562193));
#17099=DIRECTION('center_axis',(0.430981504924197,0.768119965562791,-0.473546894105632));
#17100=DIRECTION('ref_axis',(0.741965014102678,-0.00298420341976002,0.670431959543668));
#17101=DIRECTION('center_axis',(-0.430981504924197,-0.768119965562791,0.473546894105632));
#17102=DIRECTION('ref_axis',(-0.51355901341607,0.640299002836773,0.571204277562193));
#17103=DIRECTION('center_axis',(0.430981504924197,0.768119965562791,-0.473546894105632));
#17104=DIRECTION('ref_axis',(0.741965014102678,-0.00298420341976002,0.670431959543668));
#17105=DIRECTION('center_axis',(-0.430981504924197,-0.768119965562791,0.473546894105632));
#17106=DIRECTION('ref_axis',(-0.51355901341607,0.640299002836773,0.571204277562193));
#17107=DIRECTION('center_axis',(-0.741965014102678,0.00298420341976008,
-0.670431959543668));
#17108=DIRECTION('ref_axis',(-0.51355901341607,0.640299002836773,0.571204277562193));
#17109=DIRECTION('',(-0.430981504924197,-0.768119965562791,0.473546894105632));
#17110=DIRECTION('',(0.51355901341607,-0.640299002836773,-0.571204277562193));
#17111=DIRECTION('',(0.430981504924197,0.768119965562791,-0.473546894105632));
#17112=DIRECTION('',(-0.51355901341607,0.640299002836773,0.571204277562193));
#17113=DIRECTION('center_axis',(0.430981504924197,0.768119965562791,-0.473546894105632));
#17114=DIRECTION('ref_axis',(0.741965014102678,-0.00298420341976002,0.670431959543668));
#17115=DIRECTION('',(0.51355901341607,-0.640299002836773,-0.571204277562193));
#17116=DIRECTION('',(-0.741965014102678,0.00298420341976,-0.670431959543668));
#17117=DIRECTION('',(-0.741965014102678,0.00298420341976,-0.670431959543668));
#17118=DIRECTION('center_axis',(-0.51355901341607,0.640299002836773,0.571204277562193));
#17119=DIRECTION('ref_axis',(-0.741965014102678,0.00298420341975993,-0.670431959543668));
#17120=DIRECTION('',(0.430981504924197,0.768119965562791,-0.473546894105632));
#17121=DIRECTION('',(-0.741965014102678,0.00298420341976,-0.670431959543668));
#17122=DIRECTION('center_axis',(-0.430981504924197,-0.768119965562791,0.473546894105632));
#17123=DIRECTION('ref_axis',(-0.51355901341607,0.640299002836773,0.571204277562193));
#17124=DIRECTION('',(-0.51355901341607,0.640299002836773,0.571204277562193));
#17125=DIRECTION('',(-0.741965014102678,0.00298420341976,-0.670431959543668));
#17126=DIRECTION('center_axis',(-0.741965014102678,0.00298420341976008,
-0.670431959543668));
#17127=DIRECTION('ref_axis',(-0.51355901341607,0.640299002836773,0.571204277562193));
#17128=DIRECTION('',(-0.430981504924197,-0.768119965562791,0.473546894105632));
#17129=DIRECTION('',(0.51355901341607,-0.640299002836773,-0.571204277562193));
#17130=DIRECTION('',(0.430981504924197,0.768119965562791,-0.473546894105632));
#17131=DIRECTION('',(-0.51355901341607,0.640299002836773,0.571204277562193));
#17132=DIRECTION('center_axis',(-0.51355901341607,0.640299002836773,0.571204277562193));
#17133=DIRECTION('ref_axis',(0.430981504924197,0.768119965562791,-0.473546894105632));
#17134=DIRECTION('',(0.430981504924197,0.768119965562791,-0.473546894105632));
#17135=DIRECTION('',(0.219898548177292,-0.545252986888779,0.808915204949433));
#17136=DIRECTION('',(-0.741965014102678,0.00298420341976,-0.670431959543668));
#17137=DIRECTION('',(-0.741965014102678,0.00298420341976,-0.670431959543668));
#17138=DIRECTION('center_axis',(-0.430981504924197,-0.768119965562791,0.473546894105632));
#17139=DIRECTION('ref_axis',(-0.51355901341607,0.640299002836773,0.571204277562193));
#17140=DIRECTION('',(0.51355901341607,-0.640299002836773,-0.571204277562193));
#17141=DIRECTION('',(-0.741965014102678,0.00298420341976,-0.670431959543668));
#17142=DIRECTION('center_axis',(0.51355901341607,-0.640299002836773,-0.571204277562193));
#17143=DIRECTION('ref_axis',(-0.430981504924197,-0.768119965562791,0.473546894105632));
#17144=DIRECTION('',(-0.741965014102678,0.00298420341976,-0.670431959543668));
#17145=DIRECTION('',(-0.430981504924197,-0.768119965562791,0.473546894105632));
#17146=DIRECTION('',(-0.741965014102678,0.00298420341976,-0.670431959543668));
#17147=DIRECTION('',(-0.430981504924197,-0.768119965562791,0.473546894105632));
#17148=DIRECTION('center_axis',(0.430981504924197,0.768119965562791,-0.473546894105632));
#17149=DIRECTION('ref_axis',(0.741965014102678,-0.00298420341976002,0.670431959543668));
#17150=DIRECTION('',(-0.741965014102678,0.00298420341976,-0.670431959543668));
#17151=DIRECTION('',(0.51355901341607,-0.640299002836773,-0.571204277562193));
#17152=DIRECTION('',(0.51355901341607,-0.640299002836773,-0.571204277562193));
#17153=DIRECTION('center_axis',(-0.51355901341607,0.640299002836773,0.571204277562193));
#17154=DIRECTION('ref_axis',(-0.741965014102678,0.00298420341975993,-0.670431959543668));
#17155=DIRECTION('',(-0.741965014102678,0.00298420341976,-0.670431959543668));
#17156=DIRECTION('',(0.430981504924197,0.768119965562791,-0.473546894105632));
#17157=DIRECTION('',(0.430981504924197,0.768119965562791,-0.473546894105632));
#17158=DIRECTION('center_axis',(-0.164240744208196,0.580034296524335,-0.79786289097655));
#17159=DIRECTION('ref_axis',(0.51355901341607,-0.640299002836773,-0.571204277562193));
#17160=DIRECTION('',(-0.981729594100533,-0.0173310113105418,0.18949047499586));
#17161=DIRECTION('',(-0.51355901341607,0.640299002836773,0.571204277562193));
#17162=DIRECTION('',(-0.364106245973748,-0.787376134856833,-0.497459007256696));
#17163=DIRECTION('center_axis',(-0.1615074319492,-0.450649616418314,-0.877969403024502));
#17164=DIRECTION('ref_axis',(-0.430981504924197,-0.768119965562791,0.473546894105632));
#17165=DIRECTION('',(-0.528205843253997,0.790965038292377,-0.308825023842745));
#17166=DIRECTION('',(0.430981504924197,0.768119965562791,-0.473546894105632));
#17167=DIRECTION('center_axis',(-0.430981504924197,-0.768119965562791,0.473546894105632));
#17168=DIRECTION('ref_axis',(-0.51355901341607,0.640299002836773,0.571204277562193));
#17169=DIRECTION('',(-0.51355901341607,0.640299002836773,0.571204277562193));
#17170=DIRECTION('',(-0.51355901341607,0.640299002836773,0.571204277562193));
#17171=DIRECTION('center_axis',(-0.812934017119492,-0.576104073118877,-0.0851021782671007));
#17172=DIRECTION('ref_axis',(-0.51355901341607,0.640299002836773,0.571204277562193));
#17173=DIRECTION('',(0.51355901341607,-0.640299002836773,-0.571204277562193));
#17174=DIRECTION('',(-0.51355901341607,0.640299002836773,0.571204277562193));
#17175=DIRECTION('',(0.51355901341607,-0.640299002836773,-0.571204277562193));
#17176=DIRECTION('',(0.0894175048727878,0.0209199147460851,-0.995774506095301));
#17177=DIRECTION('center_axis',(-0.887789553801152,0.454869917367419,-0.0701645668105232));
#17178=DIRECTION('ref_axis',(0.430981504924197,0.768119965562791,-0.473546894105632));
#17179=DIRECTION('',(-0.430981504924197,-0.768119965562791,0.473546894105632));
#17180=DIRECTION('center_axis',(-0.430981504924197,-0.768119965562791,0.473546894105632));
#17181=DIRECTION('ref_axis',(-0.51355901341607,0.640299002836773,0.571204277562193));
#17182=DIRECTION('',(-0.51355901341607,0.640299002836773,0.571204277562193));
#17183=DIRECTION('',(-0.741965014102678,0.00298420341976007,-0.670431959543668));
#17184=DIRECTION('',(-0.741965014102678,0.00298420341976007,-0.670431959543668));
#17185=DIRECTION('center_axis',(-0.51355901341607,0.640299002836773,0.571204277562193));
#17186=DIRECTION('ref_axis',(0.741965014102678,-0.00298420341976001,0.670431959543668));
#17187=DIRECTION('',(0.430981504924197,0.768119965562791,-0.473546894105632));
#17188=DIRECTION('',(-0.741965014102678,0.00298420341976007,-0.670431959543668));
#17189=DIRECTION('center_axis',(0.430981504924197,0.768119965562791,-0.473546894105632));
#17190=DIRECTION('ref_axis',(0.741965014102678,-0.00298420341976002,0.670431959543668));
#17191=DIRECTION('',(0.51355901341607,-0.640299002836773,-0.571204277562193));
#17192=DIRECTION('',(-0.741965014102678,0.00298420341976007,-0.670431959543668));
#17193=DIRECTION('center_axis',(0.51355901341607,-0.640299002836773,-0.571204277562193));
#17194=DIRECTION('ref_axis',(-0.430981504924197,-0.768119965562791,0.473546894105632));
#17195=DIRECTION('',(-0.430981504924197,-0.768119965562791,0.473546894105632));
#17196=DIRECTION('center_axis',(0.741965014102678,-0.00298420341976011,
0.670431959543668));
#17197=DIRECTION('ref_axis',(0.51355901341607,-0.640299002836773,-0.571204277562193));
#17198=DIRECTION('center_axis',(-0.741965014102678,0.00298420341976008,
-0.670431959543668));
#17199=DIRECTION('ref_axis',(-0.51355901341607,0.640299002836773,0.571204277562193));
#17200=DIRECTION('',(0.51355901341607,-0.640299002836773,-0.571204277562193));
#17201=DIRECTION('',(0.430981504924197,0.768119965562791,-0.473546894105632));
#17202=DIRECTION('',(-0.51355901341607,0.640299002836773,0.571204277562193));
#17203=DIRECTION('',(-0.430981504924197,-0.768119965562791,0.473546894105632));
#17204=DIRECTION('center_axis',(-0.430981504924197,-0.768119965562791,0.473546894105632));
#17205=DIRECTION('ref_axis',(-0.51355901341607,0.640299002836773,0.571204277562193));
#17206=DIRECTION('',(0.741965014102678,-0.00298420341976,0.670431959543668));
#17207=DIRECTION('',(0.51355901341607,-0.640299002836773,-0.571204277562193));
#17208=DIRECTION('',(0.741965014102678,-0.00298420341976,0.670431959543668));
#17209=DIRECTION('',(0.51355901341607,-0.640299002836773,-0.571204277562193));
#17210=DIRECTION('center_axis',(0.51355901341607,-0.640299002836773,-0.571204277562193));
#17211=DIRECTION('ref_axis',(-0.430981504924197,-0.768119965562791,0.473546894105632));
#17212=DIRECTION('',(0.219898548177293,-0.545252986888779,0.808915204949433));
#17213=DIRECTION('',(0.430981504924197,0.768119965562791,-0.473546894105632));
#17214=DIRECTION('',(-0.829398437573059,-0.541032685939674,-0.139218764885593));
#17215=DIRECTION('',(0.741965014102678,-0.00298420341976,0.670431959543668));
#17216=DIRECTION('',(0.430981504924197,0.768119965562791,-0.473546894105632));
#17217=DIRECTION('center_axis',(0.51355901341607,-0.640299002836773,-0.571204277562193));
#17218=DIRECTION('ref_axis',(-0.430981504924197,-0.768119965562791,0.473546894105632));
#17219=DIRECTION('',(-0.430981504924197,-0.768119965562791,0.473546894105632));
#17220=DIRECTION('center_axis',(-0.1615074319492,-0.450649616418314,-0.877969403024502));
#17221=DIRECTION('ref_axis',(-0.430981504924197,-0.768119965562791,0.473546894105632));
#17222=DIRECTION('',(-0.476049847378258,0.814874001184978,-0.330691555688864));
#17223=DIRECTION('',(-0.430981504924197,-0.768119965562791,0.473546894105632));
#17224=DIRECTION('',(0.973704423145728,0.0720745365902279,-0.21611329788273));
#17225=DIRECTION('center_axis',(0.430981504924197,0.768119965562791,-0.473546894105632));
#17226=DIRECTION('ref_axis',(0.741965014102678,-0.00298420341976002,0.670431959543668));
#17227=DIRECTION('',(-0.51355901341607,0.640299002836773,0.571204277562193));
#17228=DIRECTION('',(0.741965014102678,-0.00298420341976,0.670431959543668));
#17229=DIRECTION('',(-0.51355901341607,0.640299002836773,0.571204277562193));
#17230=DIRECTION('center_axis',(-0.829398437573059,-0.541032685939675,-0.139218764885592));
#17231=DIRECTION('ref_axis',(-0.51355901341607,0.640299002836773,0.571204277562193));
#17232=DIRECTION('',(-0.219898548177293,0.545252986888779,-0.808915204949433));
#17233=DIRECTION('',(-0.116957021902796,-0.0755203978856573,0.990261442514461));
#17234=DIRECTION('',(0.51355901341607,-0.640299002836773,-0.571204277562193));
#17235=DIRECTION('center_axis',(-0.219898548177292,0.54525298688878,-0.808915204949433));
#17236=DIRECTION('ref_axis',(0.51355901341607,-0.640299002836773,-0.571204277562193));
#17237=DIRECTION('',(-0.51355901341607,0.640299002836773,0.571204277562193));
#17238=DIRECTION('',(-0.380697553864674,-0.811428139889548,-0.443456588942866));
#17239=DIRECTION('',(0.829398437573059,0.541032685939674,0.139218764885593));
#17240=DIRECTION('center_axis',(-0.741965014102678,0.00298420341976008,
-0.670431959543668));
#17241=DIRECTION('ref_axis',(-0.51355901341607,0.640299002836773,0.571204277562193));
#17242=DIRECTION('',(-0.430981504924197,-0.768119965562791,0.473546894105632));
#17243=DIRECTION('',(-0.51355901341607,0.640299002836773,0.571204277562193));
#17244=DIRECTION('center_axis',(-0.51355901341607,0.640299002836773,0.571204277562193));
#17245=DIRECTION('ref_axis',(-0.741965014102678,0.00298420341975993,-0.670431959543668));
#17246=DIRECTION('',(-0.430981504924197,-0.768119965562791,0.473546894105632));
#17247=DIRECTION('',(-0.430981504924197,-0.768119965562791,0.473546894105632));
#17248=DIRECTION('center_axis',(0.829398437573059,0.541032685939674,0.139218764885593));
#17249=DIRECTION('ref_axis',(-0.219898548177292,0.54525298688878,-0.808915204949433));
#17250=DIRECTION('',(-0.219898548177292,0.54525298688878,-0.808915204949433));
#17251=DIRECTION('center_axis',(-0.741965014102678,0.00298420341976008,
-0.670431959543668));
#17252=DIRECTION('ref_axis',(-0.51355901341607,0.640299002836773,0.571204277562193));
#17253=DIRECTION('',(-0.51355901341607,0.640299002836773,0.571204277562193));
#17254=DIRECTION('',(0.51355901341607,-0.640299002836773,-0.571204277562193));
#17255=DIRECTION('',(0.430981504924197,0.768119965562791,-0.473546894105632));
#17256=DIRECTION('center_axis',(0.887789553801152,-0.454869917367419,0.0701645668105237));
#17257=DIRECTION('ref_axis',(-0.161507431949199,-0.450649616418315,-0.877969403024502));
#17258=DIRECTION('',(0.116957021902797,0.0755203978856587,-0.990261442514461));
#17259=DIRECTION('',(0.380697553864674,0.811428139889549,0.443456588942865));
#17260=DIRECTION('center_axis',(0.219898548177294,-0.545252986888779,0.808915204949433));
#17261=DIRECTION('ref_axis',(0.51355901341607,-0.640299002836773,-0.571204277562193));
#17262=DIRECTION('',(0.973704423145727,0.0720745365902286,-0.216113297882731));
#17263=DIRECTION('',(-0.51355901341607,0.640299002836773,0.571204277562193));
#17264=DIRECTION('center_axis',(0.829398437573059,0.541032685939674,0.139218764885593));
#17265=DIRECTION('ref_axis',(-0.219898548177292,0.54525298688878,-0.808915204949433));
#17266=DIRECTION('',(-0.476049847378257,0.814874001184979,-0.330691555688864));
#17267=DIRECTION('center_axis',(0.51355901341607,-0.640299002836773,-0.571204277562193));
#17268=DIRECTION('ref_axis',(-0.430981504924197,-0.768119965562791,0.473546894105632));
#17269=DIRECTION('',(-0.741965014102678,0.00298420341976,-0.670431959543668));
#17270=DIRECTION('center_axis',(0.1615074319492,0.450649616418314,0.877969403024502));
#17271=DIRECTION('ref_axis',(0.430981504924197,0.768119965562791,-0.473546894105632));
#17272=DIRECTION('center_axis',(-0.741965014102678,0.00298420341976008,
-0.670431959543668));
#17273=DIRECTION('ref_axis',(-0.51355901341607,0.640299002836773,0.571204277562193));
#17274=DIRECTION('center_axis',(0.765578497613709,-0.033471246755464,0.642471197511742));
#17275=DIRECTION('ref_axis',(0.477644749164911,-0.63943052331309,-0.602481617521014));
#17276=DIRECTION('center_axis',(-0.716668115383597,-0.0275096106575757,
-0.69687160489863));
#17277=DIRECTION('ref_axis',(0.548308083841373,-0.639714733162591,-0.538630954707318));
#17278=DIRECTION('center_axis',(-0.430981504924197,-0.768119965562791,0.473546894105632));
#17279=DIRECTION('ref_axis',(0.513559013416073,-0.640299002836773,-0.57120427756219));
#17280=DIRECTION('center_axis',(-0.430981504924197,-0.768119965562791,0.473546894105632));
#17281=DIRECTION('ref_axis',(-0.513559013416071,0.640299002836773,0.571204277562192));
#17282=DIRECTION('center_axis',(0.430981504924197,0.768119965562791,-0.473546894105632));
#17283=DIRECTION('ref_axis',(0.51355901341607,-0.640299002836773,-0.571204277562193));
#17284=DIRECTION('',(0.430981504924197,0.768119965562791,-0.473546894105632));
#17285=DIRECTION('center_axis',(0.430981504924197,0.768119965562791,-0.473546894105632));
#17286=DIRECTION('ref_axis',(0.513559013416071,-0.640299002836773,-0.571204277562193));
#17287=DIRECTION('',(0.430981504924197,0.768119965562791,-0.473546894105632));
#17288=DIRECTION('center_axis',(0.741965014102679,-0.00298420341976144,
0.670431959543667));
#17289=DIRECTION('ref_axis',(0.513559013416068,-0.640299002836773,-0.571204277562195));
#17290=DIRECTION('',(0.513559013416069,-0.640299002836773,-0.571204277562194));
#17291=DIRECTION('',(0.513559013416069,-0.640299002836773,-0.571204277562194));
#17292=DIRECTION('',(0.430981504924197,0.768119965562791,-0.473546894105632));
#17293=DIRECTION('center_axis',(-0.430981504924197,-0.768119965562791,0.473546894105632));
#17294=DIRECTION('ref_axis',(0.51355901341607,-0.640299002836773,-0.571204277562193));
#17295=DIRECTION('center_axis',(0.430981504924197,0.768119965562791,-0.473546894105632));
#17296=DIRECTION('ref_axis',(-0.51355901341607,0.640299002836773,0.571204277562193));
#17297=DIRECTION('center_axis',(0.430981504924197,0.768119965562791,-0.473546894105632));
#17298=DIRECTION('ref_axis',(-0.51355901341607,0.640299002836773,0.571204277562193));
#17299=DIRECTION('',(0.430981504924197,0.768119965562791,-0.473546894105632));
#17300=DIRECTION('center_axis',(-0.430981504924197,-0.768119965562791,0.473546894105632));
#17301=DIRECTION('ref_axis',(-0.51355901341607,0.640299002836773,0.571204277562193));
#17302=DIRECTION('center_axis',(0.741965014102678,-0.00298420341976019,
0.670431959543668));
#17303=DIRECTION('ref_axis',(0.51355901341607,-0.640299002836773,-0.571204277562193));
#17304=DIRECTION('',(0.51355901341607,-0.640299002836773,-0.571204277562193));
#17305=DIRECTION('',(0.430981504924197,0.768119965562791,-0.473546894105632));
#17306=DIRECTION('',(0.51355901341607,-0.640299002836773,-0.571204277562193));
#17307=DIRECTION('',(0.430981504924197,0.768119965562791,-0.473546894105632));
#17308=DIRECTION('center_axis',(-0.51355901341607,0.640299002836773,0.571204277562193));
#17309=DIRECTION('ref_axis',(-0.741965014102678,0.00298420341975993,-0.670431959543668));
#17310=DIRECTION('',(0.741965014102678,-0.00298420341976,0.670431959543668));
#17311=DIRECTION('',(0.741965014102678,-0.00298420341976,0.670431959543668));
#17312=DIRECTION('center_axis',(0.51355901341607,-0.640299002836773,-0.571204277562193));
#17313=DIRECTION('ref_axis',(-0.741965014102678,0.00298420341975985,-0.670431959543668));
#17314=DIRECTION('',(-0.741965014102678,0.00298420341975983,-0.670431959543668));
#17315=DIRECTION('',(-0.741965014102678,0.00298420341975983,-0.670431959543668));
#17316=DIRECTION('center_axis',(0.430981504924197,0.768119965562791,-0.473546894105632));
#17317=DIRECTION('ref_axis',(0.741965014102678,-0.00298420341976002,0.670431959543668));
#17318=DIRECTION('center_axis',(-0.741965014102677,0.00298420341975833,
-0.67043195954367));
#17319=DIRECTION('ref_axis',(-0.513559013416072,0.640299002836773,0.571204277562191));
#17320=DIRECTION('',(-0.513559013416072,0.640299002836773,0.571204277562191));
#17321=DIRECTION('',(-0.513559013416072,0.640299002836773,0.571204277562191));
#17322=DIRECTION('center_axis',(0.430981504924197,0.768119965562791,-0.473546894105632));
#17323=DIRECTION('ref_axis',(0.741965014102678,-0.00298420341976002,0.670431959543668));
#17324=DIRECTION('center_axis',(0.741965014102678,-0.00298420341976016,
0.670431959543668));
#17325=DIRECTION('ref_axis',(0.430981504924197,0.768119965562791,-0.473546894105632));
#17326=DIRECTION('center_axis',(-0.430981504924197,-0.768119965562791,0.473546894105632));
#17327=DIRECTION('ref_axis',(-0.51355901341607,0.640299002836773,0.571204277562193));
#17328=DIRECTION('center_axis',(0.430981504924197,0.768119965562791,-0.473546894105632));
#17329=DIRECTION('ref_axis',(0.741965014102678,-0.00298420341976002,0.670431959543668));
#17330=DIRECTION('center_axis',(-0.741965014102678,0.00298420341976011,
-0.670431959543668));
#17331=DIRECTION('ref_axis',(-0.51355901341607,0.640299002836773,0.571204277562193));
#17332=DIRECTION('center_axis',(-0.430981504924197,-0.768119965562791,0.473546894105632));
#17333=DIRECTION('ref_axis',(-0.51355901341607,0.640299002836773,0.571204277562193));
#17334=DIRECTION('',(-0.51355901341607,0.640299002836773,0.571204277562193));
#17335=DIRECTION('',(-0.741965014102678,0.00298420341976,-0.670431959543668));
#17336=DIRECTION('',(-0.51355901341607,0.640299002836773,0.571204277562193));
#17337=DIRECTION('',(-0.741965014102678,0.00298420341976,-0.670431959543668));
#17338=DIRECTION('center_axis',(-0.51355901341607,0.640299002836773,0.571204277562193));
#17339=DIRECTION('ref_axis',(-0.741965014102678,0.00298420341975993,-0.670431959543668));
#17340=DIRECTION('',(0.430981504924197,0.768119965562791,-0.473546894105632));
#17341=DIRECTION('',(0.430981504924197,0.768119965562791,-0.473546894105632));
#17342=DIRECTION('',(-0.741965014102678,0.00298420341976,-0.670431959543668));
#17343=DIRECTION('center_axis',(0.741965014102678,-0.00298420341976016,
0.670431959543668));
#17344=DIRECTION('ref_axis',(0.430981504924197,0.768119965562791,-0.473546894105632));
#17345=DIRECTION('',(0.51355901341607,-0.640299002836773,-0.571204277562193));
#17346=DIRECTION('',(-0.430981504924197,-0.768119965562791,0.473546894105632));
#17347=DIRECTION('center_axis',(-0.430981504924197,-0.768119965562791,0.473546894105632));
#17348=DIRECTION('ref_axis',(-0.51355901341607,0.640299002836773,0.571204277562193));
#17349=DIRECTION('center_axis',(0.51355901341607,-0.640299002836773,-0.571204277562193));
#17350=DIRECTION('ref_axis',(-0.430981504924197,-0.768119965562791,0.473546894105632));
#17351=DIRECTION('',(-0.741965014102678,0.00298420341976,-0.670431959543668));
#17352=DIRECTION('',(-0.430981504924197,-0.768119965562791,0.473546894105632));
#17353=DIRECTION('center_axis',(0.741965014102678,-0.00298420341976016,
0.670431959543668));
#17354=DIRECTION('ref_axis',(0.430981504924197,0.768119965562791,-0.473546894105632));
#17355=DIRECTION('',(0.51355901341607,-0.640299002836773,-0.571204277562193));
#17356=DIRECTION('center_axis',(0.430981504924197,0.768119965562791,-0.473546894105632));
#17357=DIRECTION('ref_axis',(0.741965014102678,-0.00298420341976002,0.670431959543668));
#17358=DIRECTION('center_axis',(-0.887789553801152,0.454869917367419,-0.0701645668105238));
#17359=DIRECTION('ref_axis',(0.430981504924197,0.768119965562791,-0.473546894105632));
#17360=DIRECTION('axis',(0.,0.,1.));
#17361=DIRECTION('refdir',(1.,0.,0.));
#17362=DIRECTION('center_axis',(0.4309815049242,0.768119965562789,-0.473546894105633));
#17363=DIRECTION('ref_axis',(0.473546894105632,0.254189745109286,0.843291712614434));
#17364=DIRECTION('center_axis',(-0.4309815049242,-0.768119965562789,0.473546894105633));
#17365=DIRECTION('ref_axis',(0.473546894105632,0.254189745109287,0.843291712614434));
#17366=DIRECTION('',(-0.4309815049242,-0.768119965562789,0.473546894105633));
#17367=DIRECTION('center_axis',(-0.4309815049242,-0.768119965562789,0.473546894105633));
#17368=DIRECTION('ref_axis',(0.473546894105632,0.254189745109287,0.843291712614434));
#17369=DIRECTION('center_axis',(-0.473546894105632,-0.254189745109287,-0.843291712614434));
#17370=DIRECTION('ref_axis',(-0.768119965562789,0.587689792309766,0.254189745109285));
#17371=DIRECTION('center_axis',(-0.76811996556279,0.587689792309766,0.254189745109285));
#17372=DIRECTION('ref_axis',(0.473546894105632,0.254189745109286,0.843291712614434));
#17373=DIRECTION('center_axis',(0.473546894105632,0.254189745109287,0.843291712614434));
#17374=DIRECTION('ref_axis',(0.4309815049242,0.768119965562789,-0.473546894105633));
#17375=DIRECTION('center_axis',(-0.901241018937803,0.340275210200539,-0.268286054626271));
#17376=DIRECTION('ref_axis',(-0.044939606108901,0.542406212931598,0.838913542610905));
#17377=DIRECTION('center_axis',(0.825384593743779,-0.123480199588392,0.550901908437453));
#17378=DIRECTION('ref_axis',(0.364685089938824,-0.628286844373994,-0.687212067969474));
#17379=DIRECTION('center_axis',(-0.76811996556279,0.587689792309766,0.254189745109285));
#17380=DIRECTION('ref_axis',(0.473546894105632,0.254189745109287,0.843291712614434));
#17381=DIRECTION('center_axis',(0.473546894105632,0.254189745109287,0.843291712614434));
#17382=DIRECTION('ref_axis',(0.4309815049242,0.768119965562789,-0.473546894105633));
#17383=DIRECTION('center_axis',(0.76811996556279,-0.587689792309766,-0.254189745109285));
#17384=DIRECTION('ref_axis',(-0.473546894105632,-0.254189745109286,-0.843291712614434));
#17385=DIRECTION('center_axis',(-0.0449396061089009,0.542406212931599,0.838913542610905));
#17386=DIRECTION('ref_axis',(0.901241018937803,-0.340275210200539,0.268286054626271));
#17387=DIRECTION('center_axis',(0.364685089938824,-0.628286844373994,-0.687212067969474));
#17388=DIRECTION('ref_axis',(-0.825384593743779,0.123480199588392,-0.550901908437453));
#17389=DIRECTION('center_axis',(0.473546894105632,0.254189745109287,0.843291712614434));
#17390=DIRECTION('ref_axis',(0.4309815049242,0.768119965562789,-0.473546894105633));
#17391=DIRECTION('center_axis',(0.76811996556279,-0.587689792309766,-0.254189745109285));
#17392=DIRECTION('ref_axis',(-0.473546894105632,-0.254189745109287,-0.843291712614434));
#17393=DIRECTION('center_axis',(-0.473546894105632,-0.254189745109287,-0.843291712614434));
#17394=DIRECTION('ref_axis',(-0.4309815049242,-0.768119965562789,0.473546894105633));
#17395=DIRECTION('center_axis',(0.901241018937803,-0.340275210200539,0.268286054626271));
#17396=DIRECTION('ref_axis',(0.0449396061089008,-0.542406212931599,-0.838913542610904));
#17397=DIRECTION('center_axis',(-0.825384593743779,0.123480199588392,-0.550901908437453));
#17398=DIRECTION('ref_axis',(-0.364685089938825,0.628286844373993,0.687212067969474));
#17399=DIRECTION('center_axis',(0.76811996556279,-0.587689792309766,-0.254189745109285));
#17400=DIRECTION('ref_axis',(-0.473546894105632,-0.254189745109286,-0.843291712614434));
#17401=DIRECTION('center_axis',(-0.473546894105632,-0.254189745109287,-0.843291712614434));
#17402=DIRECTION('ref_axis',(-0.4309815049242,-0.768119965562789,0.473546894105633));
#17403=DIRECTION('center_axis',(-0.76811996556279,0.587689792309766,0.254189745109285));
#17404=DIRECTION('ref_axis',(0.473546894105632,0.254189745109287,0.843291712614434));
#17405=DIRECTION('center_axis',(0.0449396061089009,-0.542406212931599,-0.838913542610905));
#17406=DIRECTION('ref_axis',(-0.901241018937802,0.34027521020054,-0.268286054626271));
#17407=DIRECTION('center_axis',(-0.364685089938824,0.628286844373994,0.687212067969474));
#17408=DIRECTION('ref_axis',(0.825384593743779,-0.123480199588392,0.550901908437452));
#17409=DIRECTION('center_axis',(-0.473546894105632,-0.254189745109287,-0.843291712614434));
#17410=DIRECTION('ref_axis',(-0.4309815049242,-0.768119965562789,0.473546894105633));
#17411=DIRECTION('center_axis',(-0.4309815049242,-0.768119965562789,0.473546894105633));
#17412=DIRECTION('ref_axis',(0.473546894105633,0.254189745109285,0.843291712614434));
#17413=DIRECTION('center_axis',(0.4309815049242,0.768119965562789,-0.473546894105633));
#17414=DIRECTION('ref_axis',(0.473546894105631,0.254189745109287,0.843291712614434));
#17415=DIRECTION('center_axis',(-0.768119965562789,0.587689792309766,0.254189745109285));
#17416=DIRECTION('ref_axis',(-0.473546894105632,-0.254189745109286,-0.843291712614434));
#17417=DIRECTION('center_axis',(-0.4309815049242,-0.768119965562789,0.473546894105633));
#17418=DIRECTION('ref_axis',(0.473546894105632,0.254189745109287,0.843291712614434));
#17419=DIRECTION('center_axis',(-0.4309815049242,-0.768119965562789,0.473546894105633));
#17420=DIRECTION('ref_axis',(0.473546894105632,0.254189745109287,0.843291712614434));
#17421=DIRECTION('',(0.441541276070288,0.773651966662426,-0.454427041455041));
#17422=DIRECTION('center_axis',(-0.4309815049242,-0.768119965562789,0.473546894105633));
#17423=DIRECTION('ref_axis',(0.473546894105631,0.254189745109287,0.843291712614434));
#17424=DIRECTION('center_axis',(-0.4309815049242,-0.768119965562789,0.473546894105633));
#17425=DIRECTION('ref_axis',(0.473546894105631,0.254189745109287,0.843291712614434));
#17426=DIRECTION('center_axis',(0.4309815049242,0.768119965562789,-0.473546894105633));
#17427=DIRECTION('ref_axis',(-0.473546894105631,-0.254189745109287,-0.843291712614434));
#17428=DIRECTION('center_axis',(-0.4309815049242,-0.768119965562789,0.473546894105633));
#17429=DIRECTION('ref_axis',(0.473546894105632,0.254189745109286,0.843291712614434));
#17430=DIRECTION('',(-0.517128186590923,-0.803475292167847,0.29496761433923));
#17431=DIRECTION('center_axis',(-0.4309815049242,-0.768119965562789,0.473546894105633));
#17432=DIRECTION('ref_axis',(0.473546894105632,0.254189745109286,0.843291712614434));
#17433=DIRECTION('center_axis',(0.4309815049242,0.768119965562789,-0.473546894105633));
#17434=DIRECTION('ref_axis',(0.47354689410563,0.254189745109288,0.843291712614435));
#17435=DIRECTION('center_axis',(-0.4309815049242,-0.768119965562789,0.473546894105633));
#17436=DIRECTION('ref_axis',(0.47354689410563,0.254189745109288,0.843291712614435));
#17437=DIRECTION('',(-0.4309815049242,-0.768119965562789,0.473546894105633));
#17438=DIRECTION('center_axis',(0.4309815049242,0.768119965562789,-0.473546894105633));
#17439=DIRECTION('ref_axis',(-0.76811996556279,0.587689792309766,0.254189745109285));
#17440=DIRECTION('center_axis',(0.4309815049242,0.768119965562789,-0.473546894105633));
#17441=DIRECTION('ref_axis',(-0.76811996556279,0.587689792309766,0.254189745109285));
#17442=DIRECTION('center_axis',(-0.76811996556279,0.587689792309766,0.254189745109285));
#17443=DIRECTION('ref_axis',(0.4309815049242,0.768119965562789,-0.473546894105633));
#17444=DIRECTION('',(0.4309815049242,0.768119965562789,-0.473546894105633));
#17445=DIRECTION('',(0.473546894105632,0.254189745109287,0.843291712614434));
#17446=DIRECTION('',(0.4309815049242,0.768119965562789,-0.473546894105633));
#17447=DIRECTION('center_axis',(0.473546894105632,0.254189745109286,0.843291712614434));
#17448=DIRECTION('ref_axis',(0.4309815049242,0.768119965562789,-0.473546894105633));
#17449=DIRECTION('',(0.76811996556279,-0.587689792309766,-0.254189745109284));
#17450=DIRECTION('',(-0.4309815049242,-0.768119965562789,0.473546894105633));
#17451=DIRECTION('',(0.4309815049242,0.768119965562789,-0.473546894105633));
#17452=DIRECTION('center_axis',(-0.76811996556279,0.587689792309766,0.254189745109285));
#17453=DIRECTION('ref_axis',(0.4309815049242,0.768119965562789,-0.473546894105633));
#17454=DIRECTION('',(0.4309815049242,0.768119965562789,-0.473546894105633));
#17455=DIRECTION('',(0.473546894105632,0.254189745109287,0.843291712614434));
#17456=DIRECTION('center_axis',(-0.473546894105632,-0.254189745109286,-0.843291712614434));
#17457=DIRECTION('ref_axis',(0.76811996556279,-0.587689792309766,-0.254189745109285));
#17458=DIRECTION('',(0.4309815049242,0.768119965562789,-0.473546894105633));
#17459=DIRECTION('',(-0.76811996556279,0.587689792309766,0.254189745109284));
#17460=DIRECTION('center_axis',(-0.364685089938824,0.628286844373993,0.687212067969474));
#17461=DIRECTION('ref_axis',(0.4309815049242,0.768119965562789,-0.473546894105633));
#17462=DIRECTION('',(0.4309815049242,0.768119965562789,-0.473546894105633));
#17463=DIRECTION('',(0.825384593743779,-0.123480199588392,0.550901908437453));
#17464=DIRECTION('center_axis',(0.0449396061089009,-0.542406212931599,-0.838913542610905));
#17465=DIRECTION('ref_axis',(0.901241018937803,-0.340275210200539,0.268286054626271));
#17466=DIRECTION('',(-0.4309815049242,-0.768119965562789,0.473546894105633));
#17467=DIRECTION('',(-0.901241018937803,0.340275210200539,-0.268286054626271));
#17468=DIRECTION('center_axis',(-0.76811996556279,0.587689792309766,0.254189745109285));
#17469=DIRECTION('ref_axis',(0.4309815049242,0.768119965562789,-0.473546894105633));
#17470=DIRECTION('',(0.473546894105632,0.254189745109287,0.843291712614434));
#17471=DIRECTION('',(0.4309815049242,0.768119965562789,-0.473546894105633));
#17472=DIRECTION('center_axis',(-0.473546894105632,-0.254189745109286,-0.843291712614434));
#17473=DIRECTION('ref_axis',(0.76811996556279,-0.587689792309766,-0.254189745109285));
#17474=DIRECTION('',(0.4309815049242,0.768119965562789,-0.473546894105633));
#17475=DIRECTION('',(-0.76811996556279,0.587689792309766,0.254189745109284));
#17476=DIRECTION('center_axis',(0.76811996556279,-0.587689792309766,-0.254189745109285));
#17477=DIRECTION('ref_axis',(-0.473546894105632,-0.254189745109287,-0.843291712614434));
#17478=DIRECTION('',(0.4309815049242,0.768119965562789,-0.473546894105633));
#17479=DIRECTION('',(-0.473546894105632,-0.254189745109287,-0.843291712614434));
#17480=DIRECTION('center_axis',(-0.825384593743779,0.123480199588392,-0.550901908437453));
#17481=DIRECTION('ref_axis',(-0.4309815049242,-0.768119965562789,0.473546894105633));
#17482=DIRECTION('',(0.4309815049242,0.768119965562789,-0.473546894105633));
#17483=DIRECTION('',(-0.364685089938824,0.628286844373994,0.687212067969474));
#17484=DIRECTION('center_axis',(0.901241018937803,-0.340275210200539,0.268286054626271));
#17485=DIRECTION('ref_axis',(-0.4309815049242,-0.768119965562789,0.473546894105633));
#17486=DIRECTION('',(-0.4309815049242,-0.768119965562789,0.473546894105633));
#17487=DIRECTION('',(0.0449396061089009,-0.542406212931599,-0.838913542610905));
#17488=DIRECTION('center_axis',(-0.473546894105632,-0.254189745109286,-0.843291712614434));
#17489=DIRECTION('ref_axis',(0.76811996556279,-0.587689792309766,-0.254189745109285));
#17490=DIRECTION('',(-0.76811996556279,0.587689792309766,0.254189745109284));
#17491=DIRECTION('',(0.4309815049242,0.768119965562789,-0.473546894105633));
#17492=DIRECTION('center_axis',(0.76811996556279,-0.587689792309766,-0.254189745109285));
#17493=DIRECTION('ref_axis',(-0.473546894105632,-0.254189745109287,-0.843291712614434));
#17494=DIRECTION('',(0.4309815049242,0.768119965562789,-0.473546894105633));
#17495=DIRECTION('',(-0.473546894105632,-0.254189745109287,-0.843291712614434));
#17496=DIRECTION('center_axis',(0.473546894105632,0.254189745109286,0.843291712614434));
#17497=DIRECTION('ref_axis',(0.4309815049242,0.768119965562789,-0.473546894105633));
#17498=DIRECTION('',(0.4309815049242,0.768119965562789,-0.473546894105633));
#17499=DIRECTION('',(0.76811996556279,-0.587689792309766,-0.254189745109284));
#17500=DIRECTION('center_axis',(0.364685089938824,-0.628286844373994,-0.687212067969474));
#17501=DIRECTION('ref_axis',(-0.825384593743779,0.123480199588392,-0.550901908437453));
#17502=DIRECTION('',(0.4309815049242,0.768119965562789,-0.473546894105633));
#17503=DIRECTION('',(-0.825384593743779,0.123480199588392,-0.550901908437453));
#17504=DIRECTION('center_axis',(-0.0449396061089009,0.542406212931599,0.838913542610905));
#17505=DIRECTION('ref_axis',(0.4309815049242,0.768119965562789,-0.473546894105633));
#17506=DIRECTION('',(-0.4309815049242,-0.768119965562789,0.473546894105633));
#17507=DIRECTION('',(0.901241018937803,-0.340275210200539,0.268286054626271));
#17508=DIRECTION('center_axis',(0.76811996556279,-0.587689792309766,-0.254189745109285));
#17509=DIRECTION('ref_axis',(-0.473546894105632,-0.254189745109287,-0.843291712614434));
#17510=DIRECTION('',(-0.473546894105632,-0.254189745109287,-0.843291712614434));
#17511=DIRECTION('',(0.4309815049242,0.768119965562789,-0.473546894105633));
#17512=DIRECTION('center_axis',(0.473546894105632,0.254189745109286,0.843291712614434));
#17513=DIRECTION('ref_axis',(0.4309815049242,0.768119965562789,-0.473546894105633));
#17514=DIRECTION('',(0.76811996556279,-0.587689792309766,-0.254189745109284));
#17515=DIRECTION('center_axis',(0.4309815049242,0.768119965562789,-0.473546894105633));
#17516=DIRECTION('ref_axis',(0.76811996556279,-0.587689792309766,-0.254189745109285));
#17517=DIRECTION('',(-0.0449396061089009,0.542406212931599,0.838913542610905));
#17518=DIRECTION('',(0.364685089938824,-0.628286844373994,-0.687212067969474));
#17519=DIRECTION('center_axis',(0.825384593743779,-0.123480199588392,0.550901908437453));
#17520=DIRECTION('ref_axis',(-0.4309815049242,-0.768119965562789,0.473546894105633));
#17521=DIRECTION('',(0.4309815049242,0.768119965562789,-0.473546894105633));
#17522=DIRECTION('center_axis',(-0.901241018937803,0.340275210200539,-0.268286054626271));
#17523=DIRECTION('ref_axis',(-0.4309815049242,-0.768119965562789,0.473546894105633));
#17524=DIRECTION('axis',(0.,0.,1.));
#17525=DIRECTION('refdir',(1.,0.,0.));
#17526=DIRECTION('center_axis',(3.88843322550999E-16,0.978147600733806,
-0.207911690817759));
#17527=DIRECTION('ref_axis',(-5.50265365050884E-13,0.207911690817759,0.978147600733806));
#17528=DIRECTION('',(0.,-0.978147600733805,0.20791169081776));
#17529=DIRECTION('center_axis',(-3.43097049309705E-16,0.978147600733805,
-0.20791169081776));
#17530=DIRECTION('ref_axis',(3.33622364636221E-13,0.20791169081776,0.978147600733805));
#17531=DIRECTION('center_axis',(2.9543986082272E-15,0.978147600733806,-0.20791169081776));
#17532=DIRECTION('ref_axis',(1.67939778347642E-14,0.20791169081776,0.978147600733806));
#17533=DIRECTION('center_axis',(-9.14925464825879E-17,0.978147600733805,
-0.20791169081776));
#17534=DIRECTION('ref_axis',(-7.57549072892314E-14,0.20791169081776,0.978147600733805));
#17535=DIRECTION('',(0.,-0.978147600733805,0.20791169081776));
#17536=DIRECTION('center_axis',(-6.86194098619411E-16,0.978147600733806,
-0.207911690817759));
#17537=DIRECTION('ref_axis',(-2.36047899524434E-14,0.207911690817759,0.978147600733806));
#17538=DIRECTION('center_axis',(-1.85321367243343E-14,0.978147600733805,
-0.207911690817761));
#17539=DIRECTION('ref_axis',(4.13512095738825E-13,0.207911690817761,0.978147600733805));
#17540=DIRECTION('center_axis',(1.E-15,0.978147600733805,-0.20791169081776));
#17541=DIRECTION('ref_axis',(2.24944215683689E-31,0.20791169081776,0.978147600733806));
#17542=DIRECTION('center_axis',(-1.E-15,-0.978147600733805,0.20791169081776));
#17543=DIRECTION('ref_axis',(2.00292312395533E-31,0.20791169081776,0.978147600733806));
#17544=DIRECTION('center_axis',(-1.E-15,-0.978147600733805,0.20791169081776));
#17545=DIRECTION('ref_axis',(2.00292312395533E-31,0.20791169081776,0.978147600733806));
#17546=DIRECTION('center_axis',(-1.E-15,-0.978147600733805,0.20791169081776));
#17547=DIRECTION('ref_axis',(2.00292312395533E-31,0.20791169081776,0.978147600733806));
#17548=DIRECTION('',(-1.E-15,-0.978147600733806,0.20791169081776));
#17549=DIRECTION('center_axis',(-1.E-15,-0.978147600733805,0.20791169081776));
#17550=DIRECTION('ref_axis',(2.00292312395533E-31,0.20791169081776,0.978147600733806));
#17551=DIRECTION('center_axis',(-1.E-15,-0.978147600733805,0.20791169081776));
#17552=DIRECTION('ref_axis',(2.00292312395533E-31,0.20791169081776,0.978147600733806));
#17553=DIRECTION('center_axis',(-1.E-15,-0.978147600733805,0.20791169081776));
#17554=DIRECTION('ref_axis',(2.00292312395533E-31,0.20791169081776,0.978147600733806));
#17555=DIRECTION('center_axis',(-1.48029736616688E-16,-0.20791169081776,
-0.978147600733806));
#17556=DIRECTION('ref_axis',(-1.,1.1842378929335E-15,-2.08166817117217E-16));
#17557=DIRECTION('center_axis',(-1.,9.78147600733805E-16,-2.0791169081776E-16));
#17558=DIRECTION('ref_axis',(-3.70646524662632E-31,0.20791169081776,0.978147600733806));
#17559=DIRECTION('center_axis',(0.,0.20791169081776,0.978147600733805));
#17560=DIRECTION('ref_axis',(1.01403901935241E-15,0.978147600733806,-0.20791169081776));
#17561=DIRECTION('center_axis',(-0.824041924199368,-0.117787965463444,-0.55414880885353));
#17562=DIRECTION('ref_axis',(-0.566528822887065,0.171327949765011,0.80603463105968));
#17563=DIRECTION('center_axis',(0.566528822887065,0.171327949765011,0.80603463105968));
#17564=DIRECTION('ref_axis',(0.824041924199368,-0.117787965463446,-0.554148808853529));
#17565=DIRECTION('center_axis',(-1.,9.78147600733805E-16,-2.0791169081776E-16));
#17566=DIRECTION('ref_axis',(-7.79618225341413E-32,0.20791169081776,0.978147600733805));
#17567=DIRECTION('center_axis',(0.,0.20791169081776,0.978147600733805));
#17568=DIRECTION('ref_axis',(1.04747777942724E-15,0.978147600733805,-0.20791169081776));
#17569=DIRECTION('center_axis',(1.,-9.78147600733805E-16,2.0791169081776E-16));
#17570=DIRECTION('ref_axis',(4.19950331238945E-31,-0.20791169081776,-0.978147600733806));
#17571=DIRECTION('center_axis',(-0.566528822887065,0.171327949765012,0.80603463105968));
#17572=DIRECTION('ref_axis',(0.824041924199368,0.117787965463444,0.55414880885353));
#17573=DIRECTION('center_axis',(0.824041924199368,-0.117787965463446,-0.554148808853529));
#17574=DIRECTION('ref_axis',(-0.566528822887065,-0.17132794976501,-0.80603463105968));
#17575=DIRECTION('center_axis',(0.,0.20791169081776,0.978147600733805));
#17576=DIRECTION('ref_axis',(1.01403901935241E-15,0.978147600733806,-0.20791169081776));
#17577=DIRECTION('center_axis',(1.,-9.78147600733805E-16,2.0791169081776E-16));
#17578=DIRECTION('ref_axis',(2.21166036268998E-31,-0.20791169081776,-0.978147600733805));
#17579=DIRECTION('center_axis',(0.,-0.20791169081776,-0.978147600733805));
#17580=DIRECTION('ref_axis',(-1.01403901935241E-15,-0.978147600733806,0.20791169081776));
#17581=DIRECTION('center_axis',(0.824041924199368,0.117787965463444,0.55414880885353));
#17582=DIRECTION('ref_axis',(0.566528822887065,-0.171327949765011,-0.80603463105968));
#17583=DIRECTION('center_axis',(-0.566528822887065,-0.171327949765011,-0.80603463105968));
#17584=DIRECTION('ref_axis',(-0.824041924199368,0.117787965463446,0.554148808853529));
#17585=DIRECTION('center_axis',(1.,-9.78147600733805E-16,2.0791169081776E-16));
#17586=DIRECTION('ref_axis',(4.19950331238945E-31,-0.20791169081776,-0.978147600733806));
#17587=DIRECTION('center_axis',(0.,-0.20791169081776,-0.978147600733805));
#17588=DIRECTION('ref_axis',(-1.04747777942724E-15,-0.978147600733805,0.20791169081776));
#17589=DIRECTION('center_axis',(-1.,9.78147600733805E-16,-2.0791169081776E-16));
#17590=DIRECTION('ref_axis',(-7.79618225341413E-32,0.20791169081776,0.978147600733805));
#17591=DIRECTION('center_axis',(0.566528822887065,-0.171327949765012,-0.80603463105968));
#17592=DIRECTION('ref_axis',(-0.824041924199368,-0.117787965463444,-0.55414880885353));
#17593=DIRECTION('center_axis',(-0.824041924199368,0.117787965463446,0.554148808853529));
#17594=DIRECTION('ref_axis',(0.566528822887065,0.17132794976501,0.80603463105968));
#17595=DIRECTION('center_axis',(0.,-0.20791169081776,-0.978147600733805));
#17596=DIRECTION('ref_axis',(-1.01403901935241E-15,-0.978147600733806,0.20791169081776));
#17597=DIRECTION('center_axis',(1.,0.,0.));
#17598=DIRECTION('ref_axis',(0.,0.20791169081776,0.978147600733805));
#17599=DIRECTION('center_axis',(-1.,5.98922883417366E-17,-1.27304988804691E-17));
#17600=DIRECTION('ref_axis',(6.12303176911189E-17,0.978147600733805,-0.20791169081776));
#17601=DIRECTION('',(-1.,0.,0.));
#17602=DIRECTION('center_axis',(-1.,0.,0.));
#17603=DIRECTION('ref_axis',(0.,-0.20791169081776,-0.978147600733805));
#17604=DIRECTION('',(-1.,0.,0.));
#17605=DIRECTION('',(-1.,0.,0.));
#17606=DIRECTION('',(-1.,0.,0.));
#17607=DIRECTION('center_axis',(-1.,0.,0.));
#17608=DIRECTION('ref_axis',(0.,-0.20791169081776,-0.978147600733805));
#17609=DIRECTION('',(-1.,0.,0.));
#17610=DIRECTION('center_axis',(-1.,5.98922883417366E-17,-1.27304988804691E-17));
#17611=DIRECTION('ref_axis',(6.12303176911189E-17,0.978147600733805,-0.20791169081776));
#17612=DIRECTION('center_axis',(-1.,0.,0.));
#17613=DIRECTION('ref_axis',(0.,-0.20791169081776,-0.978147600733805));
#17614=DIRECTION('',(-1.,0.,0.));
#17615=DIRECTION('',(-1.,0.,0.));
#17616=DIRECTION('',(-1.,0.,0.));
#17617=DIRECTION('center_axis',(-1.,0.,0.));
#17618=DIRECTION('ref_axis',(0.,-0.20791169081776,-0.978147600733805));
#17619=DIRECTION('center_axis',(-1.,0.,0.));
#17620=DIRECTION('ref_axis',(0.,-0.20791169081776,-0.978147600733805));
#17621=DIRECTION('',(-1.,0.,0.));
#17622=DIRECTION('',(-1.,0.,0.));
#17623=DIRECTION('',(-1.,0.,0.));
#17624=DIRECTION('center_axis',(-1.,0.,0.));
#17625=DIRECTION('ref_axis',(0.,-0.20791169081776,-0.978147600733805));
#17626=DIRECTION('',(-1.,0.,0.));
#17627=DIRECTION('',(-1.,0.,0.));
#17628=DIRECTION('',(-1.,0.,0.));
#17629=DIRECTION('center_axis',(-1.,0.,0.));
#17630=DIRECTION('ref_axis',(0.,0.20791169081776,0.978147600733805));
#17631=DIRECTION('',(-1.,0.,0.));
#17632=DIRECTION('center_axis',(-1.,0.,0.));
#17633=DIRECTION('ref_axis',(0.,0.20791169081776,0.978147600733805));
#17634=DIRECTION('',(-1.,0.,0.));
#17635=DIRECTION('center_axis',(-1.,0.,0.));
#17636=DIRECTION('ref_axis',(0.,-0.20791169081776,-0.978147600733805));
#17637=DIRECTION('',(-1.,0.,0.));
#17638=DIRECTION('',(-1.,0.,0.));
#17639=DIRECTION('',(-1.,0.,0.));
#17640=DIRECTION('',(-1.,0.,0.));
#17641=DIRECTION('',(-1.,0.,0.));
#17642=DIRECTION('center_axis',(-1.,0.,0.));
#17643=DIRECTION('ref_axis',(0.,-0.20791169081776,-0.978147600733805));
#17644=DIRECTION('',(-1.,0.,0.));
#17645=DIRECTION('',(-1.,0.,0.));
#17646=DIRECTION('',(-1.,0.,0.));
#17647=DIRECTION('',(-1.,0.,0.));
#17648=DIRECTION('',(-1.,0.,0.));
#17649=DIRECTION('center_axis',(-1.48029736616688E-16,-0.20791169081776,
-0.978147600733806));
#17650=DIRECTION('ref_axis',(-1.,1.1842378929335E-15,-2.08166817117217E-16));
#17651=DIRECTION('center_axis',(-1.E-15,-0.978147600733805,0.20791169081776));
#17652=DIRECTION('ref_axis',(2.00292312395533E-31,0.20791169081776,0.978147600733806));
#17653=DIRECTION('center_axis',(-1.,9.78147600733805E-16,-2.0791169081776E-16));
#17654=DIRECTION('ref_axis',(-3.70646524662632E-31,0.20791169081776,0.978147600733806));
#17655=DIRECTION('center_axis',(0.,0.20791169081776,0.978147600733805));
#17656=DIRECTION('ref_axis',(1.01403901935241E-15,0.978147600733806,-0.20791169081776));
#17657=DIRECTION('center_axis',(-0.824041924199368,-0.117787965463444,-0.55414880885353));
#17658=DIRECTION('ref_axis',(-0.566528822887065,0.171327949765011,0.80603463105968));
#17659=DIRECTION('center_axis',(0.566528822887065,0.171327949765011,0.80603463105968));
#17660=DIRECTION('ref_axis',(0.824041924199368,-0.117787965463446,-0.554148808853529));
#17661=DIRECTION('center_axis',(-1.,9.78147600733805E-16,-2.0791169081776E-16));
#17662=DIRECTION('ref_axis',(-7.79618225341413E-32,0.20791169081776,0.978147600733805));
#17663=DIRECTION('center_axis',(0.,0.20791169081776,0.978147600733805));
#17664=DIRECTION('ref_axis',(1.04747777942724E-15,0.978147600733805,-0.20791169081776));
#17665=DIRECTION('center_axis',(1.,-9.78147600733805E-16,2.0791169081776E-16));
#17666=DIRECTION('ref_axis',(4.19950331238945E-31,-0.20791169081776,-0.978147600733806));
#17667=DIRECTION('center_axis',(-0.566528822887065,0.171327949765012,0.80603463105968));
#17668=DIRECTION('ref_axis',(0.824041924199368,0.117787965463444,0.55414880885353));
#17669=DIRECTION('center_axis',(0.824041924199368,-0.117787965463446,-0.554148808853529));
#17670=DIRECTION('ref_axis',(-0.566528822887065,-0.17132794976501,-0.80603463105968));
#17671=DIRECTION('center_axis',(0.,0.20791169081776,0.978147600733805));
#17672=DIRECTION('ref_axis',(1.01403901935241E-15,0.978147600733806,-0.20791169081776));
#17673=DIRECTION('center_axis',(1.,-9.78147600733805E-16,2.0791169081776E-16));
#17674=DIRECTION('ref_axis',(2.21166036268998E-31,-0.20791169081776,-0.978147600733805));
#17675=DIRECTION('center_axis',(0.,-0.20791169081776,-0.978147600733805));
#17676=DIRECTION('ref_axis',(-1.01403901935241E-15,-0.978147600733806,0.20791169081776));
#17677=DIRECTION('center_axis',(0.824041924199368,0.117787965463444,0.55414880885353));
#17678=DIRECTION('ref_axis',(0.566528822887065,-0.171327949765011,-0.80603463105968));
#17679=DIRECTION('center_axis',(-0.566528822887065,-0.171327949765011,-0.80603463105968));
#17680=DIRECTION('ref_axis',(-0.824041924199368,0.117787965463446,0.554148808853529));
#17681=DIRECTION('center_axis',(1.,-9.78147600733805E-16,2.0791169081776E-16));
#17682=DIRECTION('ref_axis',(4.19950331238945E-31,-0.20791169081776,-0.978147600733806));
#17683=DIRECTION('center_axis',(0.,-0.20791169081776,-0.978147600733805));
#17684=DIRECTION('ref_axis',(-1.04747777942724E-15,-0.978147600733805,0.20791169081776));
#17685=DIRECTION('center_axis',(-1.,9.78147600733805E-16,-2.0791169081776E-16));
#17686=DIRECTION('ref_axis',(-7.79618225341413E-32,0.20791169081776,0.978147600733805));
#17687=DIRECTION('center_axis',(0.566528822887065,-0.171327949765012,-0.80603463105968));
#17688=DIRECTION('ref_axis',(-0.824041924199368,-0.117787965463444,-0.55414880885353));
#17689=DIRECTION('center_axis',(-0.824041924199368,0.117787965463446,0.554148808853529));
#17690=DIRECTION('ref_axis',(0.566528822887065,0.17132794976501,0.80603463105968));
#17691=DIRECTION('center_axis',(0.,-0.20791169081776,-0.978147600733805));
#17692=DIRECTION('ref_axis',(-1.01403901935241E-15,-0.978147600733806,0.20791169081776));
#17693=DIRECTION('center_axis',(1.E-15,0.978147600733805,-0.20791169081776));
#17694=DIRECTION('ref_axis',(2.24944215683689E-31,0.20791169081776,0.978147600733806));
#17695=DIRECTION('center_axis',(-1.E-15,-0.978147600733805,0.20791169081776));
#17696=DIRECTION('ref_axis',(2.00292312395533E-31,0.20791169081776,0.978147600733806));
#17697=DIRECTION('center_axis',(-1.E-15,-0.978147600733805,0.20791169081776));
#17698=DIRECTION('ref_axis',(2.00292312395533E-31,0.20791169081776,0.978147600733806));
#17699=DIRECTION('center_axis',(-1.E-15,-0.978147600733805,0.20791169081776));
#17700=DIRECTION('ref_axis',(2.00292312395533E-31,0.20791169081776,0.978147600733806));
#17701=DIRECTION('',(-1.E-15,-0.978147600733806,0.20791169081776));
#17702=DIRECTION('center_axis',(-1.E-15,-0.978147600733805,0.20791169081776));
#17703=DIRECTION('ref_axis',(2.00292312395533E-31,0.20791169081776,0.978147600733806));
#17704=DIRECTION('center_axis',(-1.E-15,-0.978147600733805,0.20791169081776));
#17705=DIRECTION('ref_axis',(2.00292312395533E-31,0.20791169081776,0.978147600733806));
#17706=DIRECTION('center_axis',(0.,-0.978147600733806,0.20791169081776));
#17707=DIRECTION('ref_axis',(0.,-0.20791169081776,-0.978147600733805));
#17708=DIRECTION('center_axis',(-4.56588875816933E-15,0.978147600733806,
-0.207911690817759));
#17709=DIRECTION('ref_axis',(-4.8480728466622E-14,0.207911690817759,0.978147600733806));
#17710=DIRECTION('',(-7.52746977976284E-33,0.20791169081776,0.978147600733805));
#17711=DIRECTION('center_axis',(0.,-0.978147600733806,0.20791169081776));
#17712=DIRECTION('ref_axis',(0.,-0.20791169081776,-0.978147600733805));
#17713=DIRECTION('',(-7.52746977976284E-33,0.20791169081776,0.978147600733805));
#17714=DIRECTION('center_axis',(0.,0.978147600733806,-0.20791169081776));
#17715=DIRECTION('ref_axis',(0.,0.20791169081776,0.978147600733805));
#17716=DIRECTION('center_axis',(1.28919211995368E-14,0.978147600733805,
-0.20791169081776));
#17717=DIRECTION('ref_axis',(-1.52730138049065E-13,0.20791169081776,0.978147600733805));
#17718=DIRECTION('',(-7.52746977976284E-33,-0.20791169081776,-0.978147600733805));
#17719=DIRECTION('center_axis',(1.E-15,0.978147600733805,-0.20791169081776));
#17720=DIRECTION('ref_axis',(-1.,9.78147600733805E-16,-2.0791169081776E-16));
#17721=DIRECTION('center_axis',(-0.824041924199368,-0.117787965463444,-0.55414880885353));
#17722=DIRECTION('ref_axis',(-9.98343400872365E-16,-0.978147600733805,0.20791169081776));
#17723=DIRECTION('',(-1.E-15,-0.978147600733805,0.20791169081776));
#17724=DIRECTION('',(-0.566528822887065,0.171327949765012,0.80603463105968));
#17725=DIRECTION('',(1.E-15,0.978147600733805,-0.20791169081776));
#17726=DIRECTION('center_axis',(0.566528822887065,0.171327949765011,0.80603463105968));
#17727=DIRECTION('ref_axis',(-9.8574048948753E-16,-0.978147600733805,0.20791169081776));
#17728=DIRECTION('',(0.824041924199368,-0.117787965463446,-0.554148808853529));
#17729=DIRECTION('',(1.E-15,0.978147600733805,-0.20791169081776));
#17730=DIRECTION('center_axis',(1.06123031769112E-15,0.978147600733805,
-0.20791169081776));
#17731=DIRECTION('ref_axis',(1.,-1.03803988907554E-15,2.20642189698229E-16));
#17732=DIRECTION('',(1.,-1.03803988907554E-15,2.20642189698229E-16));
#17733=DIRECTION('',(0.,0.20791169081776,0.978147600733805));
#17734=DIRECTION('',(-1.,1.03803988907554E-15,-2.20642189698229E-16));
#17735=DIRECTION('',(0.566528822887065,0.17132794976501,0.80603463105968));
#17736=DIRECTION('',(-0.824041924199368,-0.117787965463444,-0.55414880885353));
#17737=DIRECTION('',(0.,0.20791169081776,0.978147600733805));
#17738=DIRECTION('',(-1.,1.03803988907554E-15,-2.20642189698229E-16));
#17739=DIRECTION('',(0.,-0.20791169081776,-0.978147600733805));
#17740=DIRECTION('',(-0.824041924199368,0.117787965463446,0.554148808853529));
#17741=DIRECTION('',(0.566528822887065,-0.171327949765012,-0.80603463105968));
#17742=DIRECTION('',(-1.,1.03803988907554E-15,-2.20642189698229E-16));
#17743=DIRECTION('',(0.,-0.20791169081776,-0.978147600733805));
#17744=DIRECTION('',(1.,-1.03803988907554E-15,2.20642189698229E-16));
#17745=DIRECTION('',(-0.566528822887065,-0.17132794976501,-0.80603463105968));
#17746=DIRECTION('',(0.824041924199368,0.117787965463444,0.55414880885353));
#17747=DIRECTION('',(0.,-0.20791169081776,-0.978147600733805));
#17748=DIRECTION('',(1.,-1.03803988907554E-15,2.20642189698229E-16));
#17749=DIRECTION('',(0.,0.20791169081776,0.978147600733805));
#17750=DIRECTION('center_axis',(-2.46519032881566E-32,0.20791169081776,
0.978147600733805));
#17751=DIRECTION('ref_axis',(1.E-15,0.978147600733805,-0.20791169081776));
#17752=DIRECTION('',(1.E-15,0.978147600733805,-0.20791169081776));
#17753=DIRECTION('',(1.E-15,0.978147600733805,-0.20791169081776));
#17754=DIRECTION('center_axis',(1.,-9.78147600733805E-16,2.0791169081776E-16));
#17755=DIRECTION('ref_axis',(2.70889472931338E-32,-0.20791169081776,-0.978147600733805));
#17756=DIRECTION('',(-1.E-15,-0.978147600733805,0.20791169081776));
#17757=DIRECTION('center_axis',(-0.566528822887065,0.171327949765012,0.80603463105968));
#17758=DIRECTION('ref_axis',(1.0068127165452E-15,0.978147600733805,-0.20791169081776));
#17759=DIRECTION('',(1.E-15,0.978147600733805,-0.20791169081776));
#17760=DIRECTION('center_axis',(0.824041924199368,-0.117787965463446,-0.554148808853529));
#17761=DIRECTION('ref_axis',(-0.566528822887065,-0.171327949765011,-0.80603463105968));
#17762=DIRECTION('',(1.E-15,0.978147600733805,-0.20791169081776));
#17763=DIRECTION('center_axis',(-2.46519032881566E-32,0.20791169081776,
0.978147600733805));
#17764=DIRECTION('ref_axis',(1.E-15,0.978147600733805,-0.20791169081776));
#17765=DIRECTION('',(1.E-15,0.978147600733805,-0.20791169081776));
#17766=DIRECTION('center_axis',(1.,-9.78147600733805E-16,2.0791169081776E-16));
#17767=DIRECTION('ref_axis',(2.70889472931338E-32,-0.20791169081776,-0.978147600733805));
#17768=DIRECTION('',(1.E-15,0.978147600733805,-0.20791169081776));
#17769=DIRECTION('center_axis',(2.46519032881566E-32,-0.20791169081776,
-0.978147600733805));
#17770=DIRECTION('ref_axis',(1.,-9.78147600733805E-16,2.0791169081776E-16));
#17771=DIRECTION('',(-1.E-15,-0.978147600733805,0.20791169081776));
#17772=DIRECTION('center_axis',(0.824041924199368,0.117787965463444,0.55414880885353));
#17773=DIRECTION('ref_axis',(-9.98343400872365E-16,-0.978147600733805,0.20791169081776));
#17774=DIRECTION('',(1.E-15,0.978147600733805,-0.20791169081776));
#17775=DIRECTION('center_axis',(-0.566528822887065,-0.171327949765011,-0.80603463105968));
#17776=DIRECTION('ref_axis',(-9.8574048948753E-16,-0.978147600733805,0.20791169081776));
#17777=DIRECTION('',(1.E-15,0.978147600733805,-0.20791169081776));
#17778=DIRECTION('center_axis',(1.,-9.78147600733805E-16,2.0791169081776E-16));
#17779=DIRECTION('ref_axis',(2.70889472931338E-32,-0.20791169081776,-0.978147600733805));
#17780=DIRECTION('',(1.E-15,0.978147600733805,-0.20791169081776));
#17781=DIRECTION('center_axis',(2.46519032881566E-32,-0.20791169081776,
-0.978147600733805));
#17782=DIRECTION('ref_axis',(1.,-9.78147600733805E-16,2.0791169081776E-16));
#17783=DIRECTION('',(1.E-15,0.978147600733805,-0.20791169081776));
#17784=DIRECTION('center_axis',(-1.,9.78147600733805E-16,-2.0791169081776E-16));
#17785=DIRECTION('ref_axis',(1.E-15,0.978147600733805,-0.20791169081776));
#17786=DIRECTION('',(-1.E-15,-0.978147600733805,0.20791169081776));
#17787=DIRECTION('center_axis',(0.566528822887065,-0.171327949765012,-0.80603463105968));
#17788=DIRECTION('ref_axis',(0.824041924199368,0.117787965463444,0.55414880885353));
#17789=DIRECTION('',(1.E-15,0.978147600733805,-0.20791169081776));
#17790=DIRECTION('center_axis',(-0.824041924199368,0.117787965463446,0.554148808853529));
#17791=DIRECTION('ref_axis',(1.00985717000555E-15,0.978147600733805,-0.20791169081776));
#17792=DIRECTION('',(1.E-15,0.978147600733805,-0.20791169081776));
#17793=DIRECTION('center_axis',(2.46519032881566E-32,-0.20791169081776,
-0.978147600733805));
#17794=DIRECTION('ref_axis',(1.,-9.78147600733805E-16,2.0791169081776E-16));
#17795=DIRECTION('',(1.E-15,0.978147600733805,-0.20791169081776));
#17796=DIRECTION('center_axis',(-1.,9.78147600733805E-16,-2.0791169081776E-16));
#17797=DIRECTION('ref_axis',(1.E-15,0.978147600733805,-0.20791169081776));
#17798=DIRECTION('',(1.E-15,0.978147600733805,-0.20791169081776));
#17799=DIRECTION('center_axis',(-2.46519032881566E-32,0.20791169081776,
0.978147600733805));
#17800=DIRECTION('ref_axis',(1.E-15,0.978147600733805,-0.20791169081776));
#17801=DIRECTION('center_axis',(-1.,9.78147600733805E-16,-2.0791169081776E-16));
#17802=DIRECTION('ref_axis',(1.E-15,0.978147600733805,-0.20791169081776));
#17803=DIRECTION('center_axis',(1.E-15,0.978147600733805,-0.20791169081776));
#17804=DIRECTION('ref_axis',(-1.,9.78147600733805E-16,-2.0791169081776E-16));
#17805=DIRECTION('center_axis',(0.,0.978147600733805,-0.20791169081776));
#17806=DIRECTION('ref_axis',(1.,0.,0.));
#17807=DIRECTION('',(0.,-0.20791169081776,-0.978147600733805));
#17808=DIRECTION('center_axis',(0.,0.978147600733805,-0.20791169081776));
#17809=DIRECTION('ref_axis',(1.,0.,0.));
#17810=DIRECTION('center_axis',(-1.,5.98922883417366E-17,-1.27304988804691E-17));
#17811=DIRECTION('ref_axis',(-1.59425458228076E-33,0.20791169081776,0.978147600733805));
#17812=DIRECTION('center_axis',(1.,0.,0.));
#17813=DIRECTION('ref_axis',(0.,0.978147600733805,-0.20791169081776));
#17814=DIRECTION('',(-7.52746977976284E-33,-0.20791169081776,-0.978147600733805));
#17815=DIRECTION('center_axis',(1.,0.,0.));
#17816=DIRECTION('ref_axis',(0.,0.978147600733805,-0.20791169081776));
#17817=DIRECTION('center_axis',(-1.,5.98922883417366E-17,-1.27304988804691E-17));
#17818=DIRECTION('ref_axis',(-1.59425458228076E-33,0.20791169081776,0.978147600733805));
#17819=DIRECTION('center_axis',(0.,0.978147600733805,-0.20791169081776));
#17820=DIRECTION('ref_axis',(1.,0.,0.));
#17821=DIRECTION('',(0.,-0.20791169081776,-0.978147600733805));
#17822=DIRECTION('center_axis',(1.,0.,0.));
#17823=DIRECTION('ref_axis',(0.,0.978147600733805,-0.20791169081776));
#17824=DIRECTION('center_axis',(1.,0.,0.));
#17825=DIRECTION('ref_axis',(0.,0.978147600733805,-0.20791169081776));
#17826=DIRECTION('center_axis',(1.,0.,0.));
#17827=DIRECTION('ref_axis',(0.,-0.978147600733805,0.20791169081776));
#17828=DIRECTION('',(0.,0.20791169081776,0.978147600733805));
#17829=DIRECTION('center_axis',(0.,-0.978147600733805,0.20791169081776));
#17830=DIRECTION('ref_axis',(1.,0.,0.));
#17831=DIRECTION('',(0.,0.20791169081776,0.978147600733805));
#17832=DIRECTION('center_axis',(1.,0.,0.));
#17833=DIRECTION('ref_axis',(0.,-0.978147600733805,0.20791169081776));
#17834=DIRECTION('center_axis',(0.,0.978147600733806,-0.20791169081776));
#17835=DIRECTION('ref_axis',(0.,0.20791169081776,0.978147600733805));
#17836=DIRECTION('center_axis',(1.06123031769112E-15,0.978147600733805,
-0.20791169081776));
#17837=DIRECTION('ref_axis',(1.,-1.03803988907554E-15,2.20642189698229E-16));
#17838=DIRECTION('',(-0.566528822887065,0.171327949765012,0.80603463105968));
#17839=DIRECTION('',(1.,-1.03803988907554E-15,2.20642189698229E-16));
#17840=DIRECTION('',(0.,0.20791169081776,0.978147600733805));
#17841=DIRECTION('',(-1.,1.03803988907554E-15,-2.20642189698229E-16));
#17842=DIRECTION('',(0.566528822887065,0.17132794976501,0.80603463105968));
#17843=DIRECTION('',(-0.824041924199368,-0.117787965463444,-0.55414880885353));
#17844=DIRECTION('',(0.,0.20791169081776,0.978147600733805));
#17845=DIRECTION('',(-1.,1.03803988907554E-15,-2.20642189698229E-16));
#17846=DIRECTION('',(0.,-0.20791169081776,-0.978147600733805));
#17847=DIRECTION('',(-0.824041924199368,0.117787965463446,0.554148808853529));
#17848=DIRECTION('',(0.566528822887065,-0.171327949765012,-0.80603463105968));
#17849=DIRECTION('',(-1.,1.03803988907554E-15,-2.20642189698229E-16));
#17850=DIRECTION('',(0.,-0.20791169081776,-0.978147600733805));
#17851=DIRECTION('',(1.,-1.03803988907554E-15,2.20642189698229E-16));
#17852=DIRECTION('',(-0.566528822887065,-0.17132794976501,-0.80603463105968));
#17853=DIRECTION('',(0.824041924199368,0.117787965463444,0.55414880885353));
#17854=DIRECTION('',(0.,-0.20791169081776,-0.978147600733805));
#17855=DIRECTION('',(1.,-1.03803988907554E-15,2.20642189698229E-16));
#17856=DIRECTION('',(0.,0.20791169081776,0.978147600733805));
#17857=DIRECTION('',(0.824041924199368,-0.117787965463446,-0.554148808853529));
#17858=DIRECTION('center_axis',(-1.,9.78147600733805E-16,-2.0791169081776E-16));
#17859=DIRECTION('ref_axis',(1.E-15,0.978147600733805,-0.20791169081776));
#17860=DIRECTION('',(1.E-15,0.978147600733805,-0.20791169081776));
#17861=DIRECTION('',(1.E-15,0.978147600733805,-0.20791169081776));
#17862=DIRECTION('center_axis',(2.46519032881566E-32,-0.20791169081776,
-0.978147600733805));
#17863=DIRECTION('ref_axis',(1.,-9.78147600733805E-16,2.0791169081776E-16));
#17864=DIRECTION('',(1.E-15,0.978147600733805,-0.20791169081776));
#17865=DIRECTION('center_axis',(-0.824041924199368,0.117787965463446,0.554148808853529));
#17866=DIRECTION('ref_axis',(1.00985717000555E-15,0.978147600733805,-0.20791169081776));
#17867=DIRECTION('',(1.E-15,0.978147600733805,-0.20791169081776));
#17868=DIRECTION('center_axis',(0.566528822887065,-0.171327949765012,-0.80603463105968));
#17869=DIRECTION('ref_axis',(0.824041924199368,0.117787965463444,0.55414880885353));
#17870=DIRECTION('',(-1.E-15,-0.978147600733805,0.20791169081776));
#17871=DIRECTION('center_axis',(-1.,9.78147600733805E-16,-2.0791169081776E-16));
#17872=DIRECTION('ref_axis',(1.E-15,0.978147600733805,-0.20791169081776));
#17873=DIRECTION('',(1.E-15,0.978147600733805,-0.20791169081776));
#17874=DIRECTION('center_axis',(2.46519032881566E-32,-0.20791169081776,
-0.978147600733805));
#17875=DIRECTION('ref_axis',(1.,-9.78147600733805E-16,2.0791169081776E-16));
#17876=DIRECTION('',(1.E-15,0.978147600733805,-0.20791169081776));
#17877=DIRECTION('center_axis',(1.,-9.78147600733805E-16,2.0791169081776E-16));
#17878=DIRECTION('ref_axis',(2.70889472931338E-32,-0.20791169081776,-0.978147600733805));
#17879=DIRECTION('',(1.E-15,0.978147600733805,-0.20791169081776));
#17880=DIRECTION('center_axis',(-0.566528822887065,-0.171327949765011,-0.80603463105968));
#17881=DIRECTION('ref_axis',(-9.8574048948753E-16,-0.978147600733805,0.20791169081776));
#17882=DIRECTION('',(1.E-15,0.978147600733805,-0.20791169081776));
#17883=DIRECTION('center_axis',(0.824041924199368,0.117787965463444,0.55414880885353));
#17884=DIRECTION('ref_axis',(-9.98343400872365E-16,-0.978147600733805,0.20791169081776));
#17885=DIRECTION('',(-1.E-15,-0.978147600733805,0.20791169081776));
#17886=DIRECTION('center_axis',(2.46519032881566E-32,-0.20791169081776,
-0.978147600733805));
#17887=DIRECTION('ref_axis',(1.,-9.78147600733805E-16,2.0791169081776E-16));
#17888=DIRECTION('',(1.E-15,0.978147600733805,-0.20791169081776));
#17889=DIRECTION('center_axis',(1.,-9.78147600733805E-16,2.0791169081776E-16));
#17890=DIRECTION('ref_axis',(2.70889472931338E-32,-0.20791169081776,-0.978147600733805));
#17891=DIRECTION('',(1.E-15,0.978147600733805,-0.20791169081776));
#17892=DIRECTION('center_axis',(-2.46519032881566E-32,0.20791169081776,
0.978147600733805));
#17893=DIRECTION('ref_axis',(1.E-15,0.978147600733805,-0.20791169081776));
#17894=DIRECTION('',(1.E-15,0.978147600733805,-0.20791169081776));
#17895=DIRECTION('center_axis',(0.824041924199368,-0.117787965463446,-0.554148808853529));
#17896=DIRECTION('ref_axis',(-0.566528822887065,-0.171327949765011,-0.80603463105968));
#17897=DIRECTION('',(1.E-15,0.978147600733805,-0.20791169081776));
#17898=DIRECTION('center_axis',(-0.566528822887065,0.171327949765012,0.80603463105968));
#17899=DIRECTION('ref_axis',(1.0068127165452E-15,0.978147600733805,-0.20791169081776));
#17900=DIRECTION('',(-1.E-15,-0.978147600733805,0.20791169081776));
#17901=DIRECTION('center_axis',(1.,-9.78147600733805E-16,2.0791169081776E-16));
#17902=DIRECTION('ref_axis',(2.70889472931338E-32,-0.20791169081776,-0.978147600733805));
#17903=DIRECTION('',(1.E-15,0.978147600733805,-0.20791169081776));
#17904=DIRECTION('center_axis',(-2.46519032881566E-32,0.20791169081776,
0.978147600733805));
#17905=DIRECTION('ref_axis',(1.E-15,0.978147600733805,-0.20791169081776));
#17906=DIRECTION('',(1.E-15,0.978147600733805,-0.20791169081776));
#17907=DIRECTION('center_axis',(-1.,9.78147600733805E-16,-2.0791169081776E-16));
#17908=DIRECTION('ref_axis',(1.E-15,0.978147600733805,-0.20791169081776));
#17909=DIRECTION('',(1.E-15,0.978147600733805,-0.20791169081776));
#17910=DIRECTION('center_axis',(0.566528822887065,0.171327949765011,0.80603463105968));
#17911=DIRECTION('ref_axis',(-9.8574048948753E-16,-0.978147600733805,0.20791169081776));
#17912=DIRECTION('',(1.E-15,0.978147600733805,-0.20791169081776));
#17913=DIRECTION('center_axis',(-0.824041924199368,-0.117787965463444,-0.55414880885353));
#17914=DIRECTION('ref_axis',(-9.98343400872365E-16,-0.978147600733805,0.20791169081776));
#17915=DIRECTION('',(-1.E-15,-0.978147600733805,0.20791169081776));
#17916=DIRECTION('center_axis',(-2.46519032881566E-32,0.20791169081776,
0.978147600733805));
#17917=DIRECTION('ref_axis',(1.E-15,0.978147600733805,-0.20791169081776));
#17918=DIRECTION('center_axis',(1.E-15,0.978147600733805,-0.20791169081776));
#17919=DIRECTION('ref_axis',(-1.,9.78147600733805E-16,-2.0791169081776E-16));
#17920=DIRECTION('center_axis',(1.E-15,0.978147600733805,-0.20791169081776));
#17921=DIRECTION('ref_axis',(-1.,9.78147600733805E-16,-2.0791169081776E-16));
#17922=DIRECTION('center_axis',(0.,0.978147600733805,-0.20791169081776));
#17923=DIRECTION('ref_axis',(1.,0.,0.));
#17924=DIRECTION('center_axis',(5.03209005654235E-16,0.978147600733805,
-0.207911690817761));
#17925=DIRECTION('ref_axis',(-4.65508415806216E-13,0.207911690817761,0.978147600733805));
#17926=DIRECTION('center_axis',(0.,0.978147600733805,-0.20791169081776));
#17927=DIRECTION('ref_axis',(1.,0.,0.));
#17928=DIRECTION('center_axis',(-4.57462732412941E-16,0.978147600733806,
-0.207911690817759));
#17929=DIRECTION('ref_axis',(-2.42086334163375E-13,0.207911690817759,0.978147600733806));
#17930=DIRECTION('center_axis',(0.,0.978147600733805,-0.20791169081776));
#17931=DIRECTION('ref_axis',(1.,0.,0.));
#17932=DIRECTION('center_axis',(-2.49317189165052E-15,0.978147600733805,
-0.207911690817763));
#17933=DIRECTION('ref_axis',(1.26498082100614E-13,0.207911690817763,0.978147600733805));
#17934=DIRECTION('center_axis',(7.77686645101999E-16,0.978147600733806,
-0.207911690817759));
#17935=DIRECTION('ref_axis',(1.70927684112078E-13,0.207911690817759,0.978147600733806));
#17936=DIRECTION('center_axis',(0.,0.978147600733805,-0.20791169081776));
#17937=DIRECTION('ref_axis',(1.,0.,0.));
#17938=DIRECTION('axis',(0.,0.,1.));
#17939=DIRECTION('refdir',(1.,0.,0.));
#17940=DIRECTION('center_axis',(1.,0.,0.));
#17941=DIRECTION('ref_axis',(0.,0.393919298579167,0.919145030018058));
#17942=DIRECTION('center_axis',(-1.,0.,0.));
#17943=DIRECTION('ref_axis',(0.,0.906392585430544,-0.422436363345457));
#17944=DIRECTION('center_axis',(-1.,0.,0.));
#17945=DIRECTION('ref_axis',(0.,0.906392585430544,-0.422436363345457));
#17946=DIRECTION('center_axis',(-1.,0.,0.));
#17947=DIRECTION('ref_axis',(0.,0.906392585430544,-0.422436363345457));
#17948=DIRECTION('',(-1.,0.,0.));
#17949=DIRECTION('center_axis',(-1.,0.,0.));
#17950=DIRECTION('ref_axis',(0.,0.906392585430544,-0.422436363345457));
#17951=DIRECTION('',(-1.,0.,0.));
#17952=DIRECTION('center_axis',(1.,0.,0.));
#17953=DIRECTION('ref_axis',(0.,0.393919298579167,0.919145030018058));
#17954=DIRECTION('center_axis',(1.,0.,0.));
#17955=DIRECTION('ref_axis',(0.,0.393919298579167,0.919145030018058));
#17956=DIRECTION('',(1.,0.,0.));
#17957=DIRECTION('center_axis',(1.,0.,0.));
#17958=DIRECTION('ref_axis',(0.,0.393919298579167,0.919145030018058));
#17959=DIRECTION('center_axis',(1.,0.,0.));
#17960=DIRECTION('ref_axis',(0.,-0.919145030018058,0.393919298579167));
#17961=DIRECTION('center_axis',(1.,0.,0.));
#17962=DIRECTION('ref_axis',(0.,0.919145030018058,-0.393919298579167));
#17963=DIRECTION('',(-1.,0.,0.));
#17964=DIRECTION('center_axis',(1.,0.,0.));
#17965=DIRECTION('ref_axis',(0.,0.919145030018058,-0.393919298579167));
#17966=DIRECTION('',(-1.,0.,0.));
#17967=DIRECTION('center_axis',(1.,0.,0.));
#17968=DIRECTION('ref_axis',(0.,0.919145030018058,-0.393919298579167));
#17969=DIRECTION('center_axis',(1.,0.,0.));
#17970=DIRECTION('ref_axis',(0.,-0.919145030018058,0.393919298579167));
#17971=DIRECTION('',(-1.,0.,0.));
#17972=DIRECTION('center_axis',(1.,0.,0.));
#17973=DIRECTION('ref_axis',(0.,-0.919145030018058,0.393919298579167));
#17974=DIRECTION('',(-1.,0.,0.));
#17975=DIRECTION('center_axis',(1.,0.,0.));
#17976=DIRECTION('ref_axis',(0.,0.393919298579167,0.919145030018058));
#17977=DIRECTION('center_axis',(-1.,0.,0.));
#17978=DIRECTION('ref_axis',(0.,-0.919145030018058,0.393919298579167));
#17979=DIRECTION('',(-1.,0.,0.));
#17980=DIRECTION('center_axis',(-1.,0.,0.));
#17981=DIRECTION('ref_axis',(0.,-0.919145030018058,0.393919298579167));
#17982=DIRECTION('center_axis',(-1.,0.,0.));
#17983=DIRECTION('ref_axis',(0.,-0.919145030018058,0.393919298579167));
#17984=DIRECTION('',(-1.,0.,0.));
#17985=DIRECTION('center_axis',(-1.04183445162406E-32,0.745459602640149,
0.666550808889758));
#17986=DIRECTION('ref_axis',(1.,2.2658674387795E-32,-9.71086045191213E-33));
#17987=DIRECTION('',(-1.,-2.2658674387795E-32,9.71086045191211E-33));
#17988=DIRECTION('',(3.69778549322349E-32,-0.666550808889758,0.745459602640149));
#17989=DIRECTION('',(-1.,-2.2658674387795E-32,9.71086045191211E-33));
#17990=DIRECTION('',(3.69778549322349E-32,-0.666550808889758,0.745459602640149));
#17991=DIRECTION('center_axis',(-1.,-2.46476191160893E-32,2.75654970442689E-32));
#17992=DIRECTION('ref_axis',(-3.35133178729961E-32,0.919145030018058,-0.393919298579167));
#17993=DIRECTION('',(0.,-0.745459602640149,-0.666550808889759));
#17994=DIRECTION('',(0.,-0.745459602640149,-0.666550808889759));
#17995=DIRECTION('',(3.69778549322349E-32,-0.666550808889758,0.745459602640149));
#17996=DIRECTION('center_axis',(1.04183445162406E-32,-0.745459602640149,
-0.666550808889758));
#17997=DIRECTION('ref_axis',(4.49774480223914E-49,-0.666550808889758,0.745459602640149));
#17998=DIRECTION('',(1.,2.2658674387795E-32,-9.71086045191211E-33));
#17999=DIRECTION('',(1.,2.2658674387795E-32,-9.71086045191211E-33));
#18000=DIRECTION('',(3.69778549322349E-32,-0.666550808889758,0.745459602640149));
#18001=DIRECTION('center_axis',(0.,-0.666550808889759,0.745459602640149));
#18002=DIRECTION('ref_axis',(-1.,0.,0.));
#18003=DIRECTION('',(-4.93038065763132E-32,0.745459602640149,0.666550808889759));
#18004=DIRECTION('',(1.,2.2658674387795E-32,-9.71086045191211E-33));
#18005=DIRECTION('',(0.,-0.745459602640149,-0.666550808889759));
#18006=DIRECTION('',(-1.,1.17200666323663E-15,1.0479467789238E-15));
#18007=DIRECTION('center_axis',(1.04183445162406E-32,-0.745459602640149,
-0.666550808889758));
#18008=DIRECTION('ref_axis',(4.49774480223914E-49,-0.666550808889758,0.745459602640149));
#18009=DIRECTION('',(1.,2.2658674387795E-32,-9.71086045191211E-33));
#18010=DIRECTION('',(3.69778549322349E-32,-0.666550808889758,0.745459602640149));
#18011=DIRECTION('',(3.69778549322349E-32,-0.666550808889758,0.745459602640149));
#18012=DIRECTION('center_axis',(1.57219339463306E-15,0.745459602640149,
0.666550808889758));
#18013=DIRECTION('ref_axis',(1.,-3.41933578296442E-15,1.46542962127046E-15));
#18014=DIRECTION('',(-1.,1.17200666323663E-15,1.0479467789238E-15));
#18015=DIRECTION('',(3.69778549322349E-32,-0.666550808889758,0.745459602640149));
#18016=DIRECTION('',(3.69778549322349E-32,-0.666550808889758,0.745459602640149));
#18017=DIRECTION('center_axis',(0.,0.745459602640149,0.666550808889759));
#18018=DIRECTION('ref_axis',(1.,0.,0.));
#18019=DIRECTION('',(-1.,0.,0.));
#18020=DIRECTION('',(0.,0.666550808889759,-0.745459602640149));
#18021=DIRECTION('',(0.529728772330716,0.565346465888128,-0.632274308566145));
#18022=DIRECTION('',(0.,-0.666550808889759,0.745459602640149));
#18023=DIRECTION('center_axis',(1.,0.,0.));
#18024=DIRECTION('ref_axis',(0.,-0.393919298579167,-0.919145030018058));
#18025=DIRECTION('',(0.,0.745459602640149,0.666550808889759));
#18026=DIRECTION('',(0.,-0.666550808889759,0.745459602640149));
#18027=DIRECTION('',(0.,0.745459602640149,0.666550808889759));
#18028=DIRECTION('',(0.,0.666550808889759,-0.745459602640149));
#18029=DIRECTION('center_axis',(0.848167098963991,-0.353091141689218,0.39489140012871));
#18030=DIRECTION('ref_axis',(-0.492600338968907,-0.799891160660238,0.342810497425816));
#18031=DIRECTION('',(-0.468106510930722,-0.15062637763103,0.870739908805161));
#18032=DIRECTION('',(0.468106510930722,0.848535364894395,-0.246706361790292));
#18033=DIRECTION('',(0.529728772330716,0.565346465888128,-0.632274308566145));
#18034=DIRECTION('',(0.,0.745459602640149,0.666550808889759));
#18035=DIRECTION('center_axis',(0.,0.666550808889759,-0.745459602640149));
#18036=DIRECTION('ref_axis',(1.,0.,0.));
#18037=DIRECTION('',(0.707106781186548,-0.527119540127478,-0.471322596971327));
#18038=DIRECTION('',(-1.,0.,0.));
#18039=DIRECTION('',(0.,-0.745459602640149,-0.666550808889759));
#18040=DIRECTION('',(1.,0.,0.));
#18041=DIRECTION('',(-1.,0.,0.));
#18042=DIRECTION('',(-0.707106781186549,-0.527119540127477,-0.471322596971326));
#18043=DIRECTION('center_axis',(0.,-0.745459602640149,-0.666550808889759));
#18044=DIRECTION('ref_axis',(0.,-0.666550808889759,0.745459602640149));
#18045=DIRECTION('',(1.,0.,0.));
#18046=DIRECTION('',(0.,-0.666550808889759,0.745459602640149));
#18047=DIRECTION('',(0.,-0.666550808889759,0.745459602640149));
#18048=DIRECTION('center_axis',(0.,0.745459602640149,0.666550808889759));
#18049=DIRECTION('ref_axis',(1.,0.,0.));
#18050=DIRECTION('',(-1.,0.,0.));
#18051=DIRECTION('',(0.,-0.666550808889759,0.745459602640149));
#18052=DIRECTION('',(0.,-0.666550808889759,0.745459602640149));
#18053=DIRECTION('center_axis',(-6.83191888629751E-32,-0.666550808889759,
0.745459602640149));
#18054=DIRECTION('ref_axis',(-1.,6.92868844298358E-32,-2.96943790413582E-32));
#18055=DIRECTION('center_axis',(6.83191888629751E-32,0.666550808889759,
-0.745459602640149));
#18056=DIRECTION('ref_axis',(-3.90611085686253E-47,0.745459602640149,0.666550808889759));
#18057=DIRECTION('',(9.16407275022627E-16,-0.745459602640149,-0.666550808889759));
#18058=DIRECTION('',(9.16407275022627E-16,-0.745459602640149,-0.666550808889759));
#18059=DIRECTION('',(9.16407275022627E-16,-0.745459602640149,-0.666550808889759));
#18060=DIRECTION('',(9.16407275022627E-16,-0.745459602640149,-0.666550808889759));
#18061=DIRECTION('center_axis',(6.83191888629751E-32,0.666550808889759,
-0.745459602640149));
#18062=DIRECTION('ref_axis',(-8.13589634095566E-47,0.745459602640149,0.666550808889759));
#18063=DIRECTION('',(9.16407275022627E-16,-0.745459602640149,-0.666550808889759));
#18064=DIRECTION('center_axis',(-0.918412615811006,-0.26370342792269,0.294921632338166));
#18065=DIRECTION('ref_axis',(3.6676144219822E-17,0.745459602640148,0.66655080888976));
#18066=DIRECTION('',(-0.393983915184351,0.541825269129043,-0.742429829889162));
#18067=DIRECTION('',(9.16407275022627E-16,-0.745459602640149,-0.666550808889759));
#18068=DIRECTION('',(-0.395623896041664,0.612168671963385,-0.684639503642172));
#18069=DIRECTION('center_axis',(0.918412615811007,0.263703427922722,-0.294921632338134));
#18070=DIRECTION('ref_axis',(0.395623896041661,-0.61216867196347,0.684639503642098));
#18071=DIRECTION('center_axis',(0.91841261581104,0.26370342792224,-0.294921632338462));
#18072=DIRECTION('ref_axis',(0.395623896041585,-0.612168671941529,0.684639503661761));
#18073=DIRECTION('center_axis',(0.,0.666550808889759,-0.745459602640149));
#18074=DIRECTION('ref_axis',(1.,0.,0.));
#18075=DIRECTION('',(-1.,0.,0.));
#18076=DIRECTION('',(-3.46944695195361E-15,0.745459602640149,0.666550808889759));
#18077=DIRECTION('',(0.974370064785235,0.16769192358466,0.149941307233507));
#18078=DIRECTION('',(0.,-0.745459602640149,-0.666550808889759));
#18079=DIRECTION('',(-1.,0.,0.));
#18080=DIRECTION('',(0.,-0.745459602640149,-0.666550808889759));
#18081=DIRECTION('center_axis',(1.,-2.15204789668062E-15,-1.92424815673669E-15));
#18082=DIRECTION('ref_axis',(-2.61639632775514E-15,-0.393919298579167,-0.919145030018058));
#18083=DIRECTION('',(5.91645678915759E-31,-0.666550808889758,0.745459602640149));
#18084=DIRECTION('',(-1.22004564440084E-15,0.289055347086673,-0.957312387008861));
#18085=DIRECTION('',(2.88687393529957E-15,0.745459602640149,0.666550808889758));
#18086=DIRECTION('',(-1.22004564440084E-15,-0.919145030018058,0.393919298579168));
#18087=DIRECTION('',(5.91645678915759E-31,-0.666550808889758,0.745459602640149));
#18088=DIRECTION('',(2.88687393529957E-15,0.745459602640149,0.666550808889758));
#18089=DIRECTION('center_axis',(6.4557060863977E-15,0.745459602640149,0.666550808889758));
#18090=DIRECTION('ref_axis',(1.,-1.40404017094047E-14,6.0173150183163E-15));
#18091=DIRECTION('',(1.,-4.81246809392762E-15,-4.30305611384292E-15));
#18092=DIRECTION('',(5.91645678915759E-31,-0.666550808889758,0.745459602640149));
#18093=DIRECTION('',(-1.,4.81246809392762E-15,4.30305611384292E-15));
#18094=DIRECTION('center_axis',(6.73294499808335E-16,0.745459602640149,
0.666550808889758));
#18095=DIRECTION('ref_axis',(1.,-1.46433637460046E-15,6.27572731971625E-16));
#18096=DIRECTION('',(5.91645678915759E-31,-0.666550808889758,0.745459602640149));
#18097=DIRECTION('',(1.,-5.0191385028692E-16,-4.48784993468273E-16));
#18098=DIRECTION('',(5.91645678915759E-31,-0.666550808889758,0.745459602640149));
#18099=DIRECTION('',(-1.,5.01913850286919E-16,4.48784993468272E-16));
#18100=DIRECTION('center_axis',(-1.,3.2296864575908E-15,2.88781593683036E-15));
#18101=DIRECTION('ref_axis',(-3.92655748994937E-15,-0.393919298579167,-0.919145030018058));
#18102=DIRECTION('',(-4.33247683194691E-15,-0.745459602640149,-0.666550808889758));
#18103=DIRECTION('',(1.83098382774925E-15,-0.289055347086674,0.95731238700886));
#18104=DIRECTION('',(5.91645678915759E-31,-0.666550808889758,0.745459602640149));
#18105=DIRECTION('',(-4.33247683194691E-15,-0.745459602640149,-0.666550808889758));
#18106=DIRECTION('',(1.83098382774927E-15,0.919145030018059,-0.393919298579165));
#18107=DIRECTION('center_axis',(-5.85085669692213E-15,-0.393919298579168,
-0.919145030018058));
#18108=DIRECTION('ref_axis',(2.88250692241653E-32,-0.919145030018058,0.393919298579168));
#18109=DIRECTION('',(1.22004564440084E-15,0.919145030018058,-0.393919298579168));
#18110=DIRECTION('',(-1.,4.81246809392762E-15,4.30305611384292E-15));
#18111=DIRECTION('center_axis',(6.10212048145241E-16,0.957312387008861,
0.289055347086673));
#18112=DIRECTION('ref_axis',(1.,-3.73956028970675E-16,-8.72564067598243E-16));
#18113=DIRECTION('',(-1.,5.0191385028692E-16,4.48784993468273E-16));
#18114=DIRECTION('',(1.22004564440084E-15,-0.289055347086673,0.957312387008861));
#18115=DIRECTION('',(1.,-5.0191385028692E-16,-4.48784993468273E-16));
#18116=DIRECTION('center_axis',(-9.86076131526264E-31,0.666550808889758,
-0.745459602640149));
#18117=DIRECTION('ref_axis',(1.,-9.19114135003496E-31,-2.14459964834149E-30));
#18118=DIRECTION('',(-2.88687393529957E-15,-0.745459602640149,-0.666550808889758));
#18119=DIRECTION('center_axis',(-6.10212048145241E-16,-0.393919298579165,
-0.919145030018059));
#18120=DIRECTION('ref_axis',(1.,-2.4037430198993E-16,-5.60873371309838E-16));
#18121=DIRECTION('',(-1.22004564440084E-15,-0.919145030018059,0.393919298579165));
#18122=DIRECTION('',(-1.,5.0191385028692E-16,4.48784993468273E-16));
#18123=DIRECTION('center_axis',(6.10212048145256E-16,0.957312387008861,
0.289055347086674));
#18124=DIRECTION('ref_axis',(1.,-3.73956028970684E-16,-8.72564067598264E-16));
#18125=DIRECTION('',(-1.22004564440084E-15,0.289055347086674,-0.95731238700886));
#18126=DIRECTION('',(-1.,5.01913850286932E-16,4.48784993468284E-16));
#18127=DIRECTION('',(1.,-5.01913850286932E-16,-4.48784993468284E-16));
#18128=DIRECTION('center_axis',(-2.23422119153307E-32,0.666550808889759,
-0.745459602640149));
#18129=DIRECTION('ref_axis',(1.,-2.08250074432281E-32,-4.8591684034199E-32));
#18130=DIRECTION('',(0.,0.745459602640149,0.666550808889759));
#18131=DIRECTION('center_axis',(0.,0.666550808889759,-0.745459602640149));
#18132=DIRECTION('ref_axis',(0.,-0.745459602640149,-0.666550808889759));
#18133=DIRECTION('',(0.173648177666931,-0.656424404371193,0.734134396237418));
#18134=DIRECTION('center_axis',(0.,-0.666550808889759,0.745459602640149));
#18135=DIRECTION('ref_axis',(0.,0.745459602640149,0.666550808889759));
#18136=DIRECTION('',(0.,0.785872105893968,-0.618389062951294));
#18137=DIRECTION('center_axis',(0.,0.666550808889759,-0.745459602640149));
#18138=DIRECTION('ref_axis',(0.,0.745459602640149,0.666550808889759));
#18139=DIRECTION('center_axis',(2.46383476629014E-15,0.618389062951294,
0.785872105893968));
#18140=DIRECTION('ref_axis',(1.,-8.74982549805887E-15,3.74992521345379E-15));
#18141=DIRECTION('',(-1.,1.86502317861713E-15,1.66760573464032E-15));
#18142=DIRECTION('',(1.00410523453136E-15,0.785872105893969,-0.618389062951293));
#18143=DIRECTION('',(1.,-1.86502317861713E-15,-1.66760573464032E-15));
#18144=DIRECTION('center_axis',(-0.984807753012208,-0.115745333286125,0.129447701522776));
#18145=DIRECTION('ref_axis',(1.45875349239297E-18,0.74545960264015,0.666550808889758));
#18146=DIRECTION('',(1.80700362080917E-16,0.745459602640149,0.666550808889759));
#18147=DIRECTION('',(0.173648177666931,-0.656424404371193,0.734134396237418));
#18148=DIRECTION('',(-1.80700362080917E-16,-0.745459602640149,-0.666550808889759));
#18149=DIRECTION('center_axis',(0.,0.666550808889759,-0.745459602640149));
#18150=DIRECTION('ref_axis',(0.,-0.745459602640149,-0.666550808889759));
#18151=DIRECTION('center_axis',(0.,-0.666550808889759,0.745459602640149));
#18152=DIRECTION('ref_axis',(0.,0.745459602640149,0.666550808889759));
#18153=DIRECTION('',(0.173648177666932,0.656424404371191,-0.73413439623742));
#18154=DIRECTION('center_axis',(0.,0.666550808889759,-0.745459602640149));
#18155=DIRECTION('ref_axis',(0.,0.745459602640149,0.666550808889759));
#18156=DIRECTION('center_axis',(0.,0.666550808889758,-0.745459602640149));
#18157=DIRECTION('ref_axis',(0.,-0.745459602640149,-0.666550808889758));
#18158=DIRECTION('center_axis',(0.,0.666550808889758,-0.745459602640149));
#18159=DIRECTION('ref_axis',(0.,0.745459602640149,0.666550808889758));
#18160=DIRECTION('',(0.,-0.526976702848416,0.849879729523544));
#18161=DIRECTION('center_axis',(0.,-0.666550808889759,0.745459602640149));
#18162=DIRECTION('ref_axis',(0.,0.745459602640149,0.666550808889759));
#18163=DIRECTION('center_axis',(0.984807753012208,-0.115745333286128,0.129447701522774));
#18164=DIRECTION('ref_axis',(-0.157804207302256,-0.907628529662534,0.388983655569657));
#18165=DIRECTION('',(3.61400724161834E-15,0.745459602640149,0.666550808889759));
#18166=DIRECTION('',(0.173648177666931,0.656424404371193,-0.734134396237418));
#18167=DIRECTION('',(-3.61400724161834E-15,-0.745459602640149,-0.666550808889759));
#18168=DIRECTION('center_axis',(-2.6834563621475E-15,-0.849879729523544,
-0.526976702848416));
#18169=DIRECTION('ref_axis',(-1.63031537087573E-31,-0.526976702848416,0.849879729523544));
#18170=DIRECTION('',(-1.,2.03126783609293E-15,1.81625297256125E-15));
#18171=DIRECTION('',(0.,-0.526976702848416,0.849879729523544));
#18172=DIRECTION('',(1.,-2.03126783609293E-15,-1.81625297256125E-15));
#18173=DIRECTION('center_axis',(-6.73294499808353E-16,-0.745459602640149,
-0.666550808889758));
#18174=DIRECTION('ref_axis',(2.12962857256229E-32,-0.666550808889758,0.745459602640149));
#18175=DIRECTION('',(5.91645678915759E-31,-0.666550808889758,0.745459602640149));
#18176=DIRECTION('',(1.,-5.01913850286932E-16,-4.48784993468284E-16));
#18177=DIRECTION('center_axis',(0.,0.66655080888976,-0.745459602640148));
#18178=DIRECTION('ref_axis',(0.,-0.745459602640148,-0.66655080888976));
#18179=DIRECTION('center_axis',(0.,-0.666550808889759,0.745459602640149));
#18180=DIRECTION('ref_axis',(0.,0.745459602640149,0.666550808889759));
#18181=DIRECTION('center_axis',(0.,0.66655080888976,-0.745459602640148));
#18182=DIRECTION('ref_axis',(0.,0.745459602640148,0.66655080888976));
#18183=DIRECTION('center_axis',(1.,6.14016151751146E-32,5.29799511051683E-33));
#18184=DIRECTION('ref_axis',(2.90569070563006E-32,-0.393919298579167,-0.919145030018058));
#18185=DIRECTION('',(-4.93038065763132E-32,0.745459602640149,0.666550808889759));
#18186=DIRECTION('center_axis',(0.,0.745459602640149,0.666550808889759));
#18187=DIRECTION('ref_axis',(1.,0.,0.));
#18188=DIRECTION('',(0.,-0.666550808889759,0.745459602640149));
#18189=DIRECTION('',(0.,-0.666550808889759,0.745459602640149));
#18190=DIRECTION('center_axis',(-0.707106781186546,0.527119540127479,0.471322596971328));
#18191=DIRECTION('ref_axis',(-6.76209254941581E-18,0.666550808889759,-0.745459602640149));
#18192=DIRECTION('center_axis',(0.707106781186548,0.527119540127479,0.471322596971327));
#18193=DIRECTION('ref_axis',(0.389281620635025,-0.846641755162944,0.362846466498404));
#18194=DIRECTION('center_axis',(0.,0.365017828521802,0.931000528926396));
#18195=DIRECTION('ref_axis',(-1.,0.,0.));
#18196=DIRECTION('',(0.,0.931000528926396,-0.365017828521802));
#18197=DIRECTION('',(-1.,0.,0.));
#18198=DIRECTION('',(0.,0.931000528926396,-0.365017828521802));
#18199=DIRECTION('',(0.,0.931000528926396,-0.365017828521802));
#18200=DIRECTION('',(0.,0.931000528926396,-0.365017828521802));
#18201=DIRECTION('center_axis',(0.,0.919145030018058,-0.393919298579167));
#18202=DIRECTION('ref_axis',(-1.,0.,0.));
#18203=DIRECTION('',(0.,-0.393919298579167,-0.919145030018058));
#18204=DIRECTION('',(0.,-0.393919298579167,-0.919145030018058));
#18205=DIRECTION('',(-1.,0.,0.));
#18206=DIRECTION('center_axis',(1.,0.,0.));
#18207=DIRECTION('ref_axis',(0.,0.3568432321356,-0.934164283024682));
#18208=DIRECTION('center_axis',(-1.,0.,0.));
#18209=DIRECTION('ref_axis',(0.,0.919145030018058,-0.393919298579167));
#18210=DIRECTION('center_axis',(-1.,0.,0.));
#18211=DIRECTION('ref_axis',(0.,0.919145030018058,-0.393919298579167));
#18212=DIRECTION('',(-1.,0.,0.));
#18213=DIRECTION('center_axis',(0.,-0.422436363345456,-0.906392585430544));
#18214=DIRECTION('ref_axis',(0.,-0.906392585430544,0.422436363345456));
#18215=DIRECTION('',(0.,-0.906392585430544,0.422436363345457));
#18216=DIRECTION('',(0.,-0.906392585430544,0.422436363345457));
#18217=DIRECTION('',(0.,-0.906392585430544,0.422436363345456));
#18218=DIRECTION('',(-1.,0.,0.));
#18219=DIRECTION('center_axis',(1.,0.,0.));
#18220=DIRECTION('ref_axis',(0.,0.393919298579167,0.919145030018058));
#18221=DIRECTION('center_axis',(-1.,0.,0.));
#18222=DIRECTION('ref_axis',(0.,0.919145030018058,-0.393919298579167));
#18223=DIRECTION('center_axis',(-1.,0.,0.));
#18224=DIRECTION('ref_axis',(0.,0.919145030018058,-0.393919298579167));
#18225=DIRECTION('',(-1.,0.,0.));
#18226=DIRECTION('center_axis',(1.,0.,0.));
#18227=DIRECTION('ref_axis',(0.,0.393919298579167,0.919145030018058));
#18228=DIRECTION('center_axis',(-1.,0.,0.));
#18229=DIRECTION('ref_axis',(0.,0.919145030018058,-0.393919298579167));
#18230=DIRECTION('',(-1.,0.,0.));
#18231=DIRECTION('center_axis',(-1.,0.,0.));
#18232=DIRECTION('ref_axis',(0.,0.919145030018058,-0.393919298579167));
#18233=DIRECTION('center_axis',(0.,-0.919145030018058,0.393919298579167));
#18234=DIRECTION('ref_axis',(0.,0.393919298579167,0.919145030018058));
#18235=DIRECTION('',(0.,0.393919298579167,0.919145030018058));
#18236=DIRECTION('',(0.,0.393919298579167,0.919145030018058));
#18237=DIRECTION('center_axis',(1.,0.,0.));
#18238=DIRECTION('ref_axis',(0.,0.393919298579168,0.919145030018058));
#18239=DIRECTION('center_axis',(-1.,0.,0.));
#18240=DIRECTION('ref_axis',(0.,0.919145030018059,-0.393919298579166));
#18241=DIRECTION('',(-1.,0.,0.));
#18242=DIRECTION('center_axis',(-1.,0.,0.));
#18243=DIRECTION('ref_axis',(0.,0.919145030018059,-0.393919298579166));
#18244=DIRECTION('center_axis',(1.,0.,0.));
#18245=DIRECTION('ref_axis',(0.,0.393919298579168,0.919145030018058));
#18246=DIRECTION('center_axis',(-1.,0.,0.));
#18247=DIRECTION('ref_axis',(0.,0.919145030018058,-0.393919298579167));
#18248=DIRECTION('center_axis',(-1.,0.,0.));
#18249=DIRECTION('ref_axis',(0.,0.919145030018058,-0.393919298579167));
#18250=DIRECTION('',(-1.,0.,0.));
#18251=DIRECTION('center_axis',(0.,-0.39391929857917,-0.919145030018057));
#18252=DIRECTION('ref_axis',(0.,-0.919145030018057,0.39391929857917));
#18253=DIRECTION('',(0.,-0.919145030018057,0.39391929857917));
#18254=DIRECTION('',(0.,-0.919145030018057,0.39391929857917));
#18255=DIRECTION('',(-1.,0.,0.));
#18256=DIRECTION('center_axis',(1.,0.,0.));
#18257=DIRECTION('ref_axis',(0.,0.393919298579168,0.919145030018058));
#18258=DIRECTION('center_axis',(-1.,0.,0.));
#18259=DIRECTION('ref_axis',(0.,0.919145030018058,-0.393919298579167));
#18260=DIRECTION('center_axis',(-1.,0.,0.));
#18261=DIRECTION('ref_axis',(0.,0.919145030018058,-0.393919298579167));
#18262=DIRECTION('center_axis',(1.,0.,0.));
#18263=DIRECTION('ref_axis',(0.,0.393919298579168,0.919145030018058));
#18264=DIRECTION('center_axis',(-1.,0.,0.));
#18265=DIRECTION('ref_axis',(0.,0.919145030018059,-0.393919298579166));
#18266=DIRECTION('center_axis',(-1.,0.,0.));
#18267=DIRECTION('ref_axis',(0.,0.919145030018059,-0.393919298579166));
#18268=DIRECTION('',(-1.,0.,0.));
#18269=DIRECTION('center_axis',(-1.,0.,0.));
#18270=DIRECTION('ref_axis',(0.,0.919145030018058,-0.393919298579167));
#18271=DIRECTION('',(0.,0.666550808889759,-0.745459602640149));
#18272=DIRECTION('center_axis',(-1.,0.,0.));
#18273=DIRECTION('ref_axis',(0.,0.919145030018058,-0.393919298579167));
#18274=DIRECTION('',(0.,0.919145030018057,-0.39391929857917));
#18275=DIRECTION('center_axis',(-1.,0.,0.));
#18276=DIRECTION('ref_axis',(0.,0.919145030018058,-0.393919298579167));
#18277=DIRECTION('',(0.,0.919145030018057,-0.39391929857917));
#18278=DIRECTION('center_axis',(0.,0.39391929857917,0.919145030018057));
#18279=DIRECTION('ref_axis',(0.,0.919145030018057,-0.39391929857917));
#18280=DIRECTION('center_axis',(0.,0.666550808889759,-0.745459602640149));
#18281=DIRECTION('ref_axis',(1.,0.,0.));
#18282=DIRECTION('',(0.,-0.745459602640149,-0.666550808889759));
#18283=DIRECTION('center_axis',(0.,-0.666550808889758,0.745459602640149));
#18284=DIRECTION('ref_axis',(0.,0.745459602640149,0.666550808889758));
#18285=DIRECTION('',(1.,0.,0.));
#18286=DIRECTION('',(0.,-0.745459602640149,-0.666550808889759));
#18287=DIRECTION('',(-1.,0.,0.));
#18288=DIRECTION('center_axis',(-1.,0.,0.));
#18289=DIRECTION('ref_axis',(0.,0.919145030018058,-0.393919298579167));
#18290=DIRECTION('',(0.,-0.666550808889758,0.745459602640149));
#18291=DIRECTION('center_axis',(0.,0.745459602640149,0.666550808889759));
#18292=DIRECTION('ref_axis',(1.,0.,0.));
#18293=DIRECTION('',(0.,0.666550808889759,-0.745459602640149));
#18294=DIRECTION('',(0.707106781186549,0.471322596971326,-0.527119540127477));
#18295=DIRECTION('',(1.,6.2631905706088E-16,-7.00465064591613E-16));
#18296=DIRECTION('',(0.,0.666550808889759,-0.745459602640149));
#18297=DIRECTION('',(0.,0.666550808889759,-0.745459602640149));
#18298=DIRECTION('',(-1.,0.,0.));
#18299=DIRECTION('center_axis',(-1.,0.,0.));
#18300=DIRECTION('ref_axis',(0.,0.919145030018058,-0.393919298579167));
#18301=DIRECTION('center_axis',(0.,0.666550808889759,-0.745459602640149));
#18302=DIRECTION('ref_axis',(1.,0.,0.));
#18303=DIRECTION('',(-0.974370064785235,0.16769192358466,0.149941307233508));
#18304=DIRECTION('',(3.46944695195361E-15,0.745459602640149,0.666550808889759));
#18305=DIRECTION('',(-1.,3.30366096032112E-16,-3.69476078026345E-16));
#18306=DIRECTION('',(0.,0.745459602640149,0.666550808889759));
#18307=DIRECTION('',(0.,-0.745459602640149,-0.666550808889759));
#18308=DIRECTION('center_axis',(0.,-0.745459602640149,-0.666550808889758));
#18309=DIRECTION('ref_axis',(0.,-0.666550808889758,0.745459602640149));
#18310=DIRECTION('',(0.707106781186547,0.471322596971327,-0.527119540127479));
#18311=DIRECTION('',(0.,0.666550808889758,-0.745459602640149));
#18312=DIRECTION('',(0.,-0.666550808889758,0.745459602640149));
#18313=DIRECTION('',(0.,-0.666550808889758,0.745459602640149));
#18314=DIRECTION('',(1.,1.92713556018732E-16,-2.15527712182035E-16));
#18315=DIRECTION('center_axis',(-1.,0.,0.));
#18316=DIRECTION('ref_axis',(0.,0.919145030018058,-0.393919298579167));
#18317=DIRECTION('',(0.,0.745459602640149,0.666550808889759));
#18318=DIRECTION('',(0.,-0.666550808889759,0.745459602640149));
#18319=DIRECTION('',(0.,-0.745459602640149,-0.666550808889759));
#18320=DIRECTION('',(0.,-0.666550808889759,0.745459602640149));
#18321=DIRECTION('',(0.,-0.745459602640149,-0.666550808889759));
#18322=DIRECTION('',(0.,-0.666550808889759,0.745459602640149));
#18323=DIRECTION('',(0.,-0.666550808889758,0.745459602640149));
#18324=DIRECTION('',(0.,-0.745459602640149,-0.666550808889759));
#18325=DIRECTION('center_axis',(-1.,0.,0.));
#18326=DIRECTION('ref_axis',(0.,0.919145030018058,-0.393919298579167));
#18327=DIRECTION('',(0.,-0.745459602640149,-0.666550808889759));
#18328=DIRECTION('',(0.,-0.745459602640149,-0.666550808889759));
#18329=DIRECTION('',(0.,-0.745459602640149,-0.666550808889759));
#18330=DIRECTION('center_axis',(-0.707106781186548,0.471322596971326,-0.527119540127479));
#18331=DIRECTION('ref_axis',(5.73427809096105E-17,-0.745459602640149,-0.666550808889758));
#18332=DIRECTION('',(0.,-0.745459602640149,-0.666550808889759));
#18333=DIRECTION('',(0.707106781186547,0.471322596971327,-0.527119540127479));
#18334=DIRECTION('',(0.,-0.745459602640149,-0.666550808889759));
#18335=DIRECTION('center_axis',(-1.,0.,0.));
#18336=DIRECTION('ref_axis',(0.,0.919145030018058,-0.393919298579167));
#18337=DIRECTION('',(0.,0.666550808889758,-0.745459602640149));
#18338=DIRECTION('center_axis',(-2.89120579329468E-16,0.666550808889759,
-0.745459602640149));
#18339=DIRECTION('ref_axis',(1.,-2.69487114317234E-16,-6.28803266740213E-16));
#18340=DIRECTION('',(1.,1.92713556018732E-16,-2.15527712182035E-16));
#18341=DIRECTION('center_axis',(7.85046229341889E-17,0.745459602640149,
0.666550808889758));
#18342=DIRECTION('ref_axis',(1.,-1.70738324714595E-16,7.31735677348263E-17));
#18343=DIRECTION('',(-1.,0.,0.));
#18344=DIRECTION('center_axis',(0.707106781186547,-0.471322596971327,0.527119540127479));
#18345=DIRECTION('ref_axis',(-0.671542934237819,-0.681054890267067,0.291880667257314));
#18346=DIRECTION('',(0.,0.745459602640149,0.666550808889759));
#18347=DIRECTION('',(0.707106781186549,0.471322596971326,-0.527119540127477));
#18348=DIRECTION('',(0.,0.745459602640149,0.666550808889759));
#18349=DIRECTION('center_axis',(1.,0.,0.));
#18350=DIRECTION('ref_axis',(0.,-0.393919298579167,-0.919145030018058));
#18351=DIRECTION('',(0.,0.666550808889759,-0.745459602640149));
#18352=DIRECTION('center_axis',(9.39641882820771E-16,-0.666550808889759,
0.745459602640149));
#18353=DIRECTION('ref_axis',(-1.,-9.52951280949986E-16,4.08407691835707E-16));
#18354=DIRECTION('',(1.,6.2631905706088E-16,-7.00465064591613E-16));
#18355=DIRECTION('center_axis',(0.,0.745459602640149,0.666550808889759));
#18356=DIRECTION('ref_axis',(1.,0.,0.));
#18357=DIRECTION('',(-1.,3.30366096032112E-16,-3.69476078026345E-16));
#18358=DIRECTION('',(-1.,3.30366096032112E-16,-3.69476078026345E-16));
#18359=DIRECTION('center_axis',(1.,-2.58633254618441E-15,-2.31256267222479E-15));
#18360=DIRECTION('ref_axis',(-3.14438678926613E-15,-0.393919298579167,-0.919145030018058));
#18361=DIRECTION('',(0.,-0.666550808889759,0.745459602640149));
#18362=DIRECTION('',(3.46944695195361E-15,0.745459602640149,0.666550808889759));
#18363=DIRECTION('',(0.,-0.666550808889759,0.745459602640149));
#18364=DIRECTION('',(3.46944695195361E-15,0.745459602640149,0.666550808889759));
#18365=DIRECTION('center_axis',(-2.45655217911417E-16,0.745459602640149,
0.666550808889759));
#18366=DIRECTION('ref_axis',(1.,5.34271216088195E-16,-2.28973378323512E-16));
#18367=DIRECTION('',(-1.,-1.83126041130723E-16,-1.63741684206845E-16));
#18368=DIRECTION('',(-1.,-1.83126041130723E-16,-1.63741684206845E-16));
#18369=DIRECTION('',(0.,-0.666550808889759,0.745459602640149));
#18370=DIRECTION('center_axis',(-1.,0.,0.));
#18371=DIRECTION('ref_axis',(0.,0.919145030018058,-0.393919298579167));
#18372=DIRECTION('',(0.,-0.745459602640149,-0.666550808889759));
#18373=DIRECTION('',(0.,-0.745459602640149,-0.666550808889759));
#18374=DIRECTION('',(0.,-0.666550808889759,0.745459602640149));
#18375=DIRECTION('',(0.,-0.745459602640149,-0.666550808889759));
#18376=DIRECTION('center_axis',(1.14639101691994E-15,0.745459602640149,
0.666550808889759));
#18377=DIRECTION('ref_axis',(1.,-2.49326567507823E-15,1.06854243217638E-15));
#18378=DIRECTION('',(-1.,8.54588191943377E-16,7.64127859631943E-16));
#18379=DIRECTION('',(-1.,8.54588191943377E-16,7.64127859631943E-16));
#18380=DIRECTION('',(0.,-0.666550808889759,0.745459602640149));
#18381=DIRECTION('center_axis',(0.,0.666550808889758,-0.745459602640149));
#18382=DIRECTION('ref_axis',(0.,0.745459602640149,0.666550808889758));
#18383=DIRECTION('center_axis',(0.,-0.666550808889758,0.745459602640149));
#18384=DIRECTION('ref_axis',(0.,-0.745459602640149,-0.666550808889758));
#18385=DIRECTION('center_axis',(0.,-0.666550808889758,0.745459602640149));
#18386=DIRECTION('ref_axis',(0.,-0.745459602640149,-0.666550808889758));
#18387=DIRECTION('center_axis',(0.,0.666550808889758,-0.745459602640149));
#18388=DIRECTION('ref_axis',(0.,0.745459602640149,0.666550808889758));
#18389=DIRECTION('center_axis',(0.,-0.666550808889758,0.745459602640149));
#18390=DIRECTION('ref_axis',(0.,0.745459602640149,0.666550808889758));
#18391=DIRECTION('',(0.,-0.666550808889759,0.745459602640149));
#18392=DIRECTION('center_axis',(0.,-0.745459602640149,-0.666550808889759));
#18393=DIRECTION('ref_axis',(0.,-0.666550808889759,0.745459602640149));
#18394=DIRECTION('',(1.,0.,0.));
#18395=DIRECTION('',(0.,-0.666550808889759,0.745459602640149));
#18396=DIRECTION('center_axis',(-1.,0.,0.));
#18397=DIRECTION('ref_axis',(0.,0.919145030018058,-0.393919298579167));
#18398=DIRECTION('',(0.,-0.745459602640149,-0.666550808889759));
#18399=DIRECTION('',(0.,-0.666550808889759,0.745459602640149));
#18400=DIRECTION('',(0.,-0.745459602640149,-0.666550808889759));
#18401=DIRECTION('center_axis',(9.16407275022628E-16,-0.745459602640149,
-0.666550808889759));
#18402=DIRECTION('ref_axis',(-5.31053524627771E-32,-0.666550808889759,0.745459602640149));
#18403=DIRECTION('',(1.,6.8314460309491E-16,6.10832010438791E-16));
#18404=DIRECTION('',(1.,6.8314460309491E-16,6.10832010438791E-16));
#18405=DIRECTION('',(0.,-0.666550808889759,0.745459602640149));
#18406=DIRECTION('center_axis',(1.,2.58633254618443E-15,2.31256267222479E-15));
#18407=DIRECTION('ref_axis',(1.46625164003621E-15,-0.919145030018058,0.393919298579167));
#18408=DIRECTION('',(-3.46944695195361E-15,0.745459602640149,0.666550808889759));
#18409=DIRECTION('',(-3.46944695195361E-15,0.745459602640149,0.666550808889759));
#18410=DIRECTION('',(0.,-0.666550808889759,0.745459602640149));
#18411=DIRECTION('center_axis',(0.224951054343865,-0.726353521319258,-0.649467154840565));
#18412=DIRECTION('ref_axis',(1.77259243224035E-17,-0.666550808889758,0.745459602640149));
#18413=DIRECTION('',(0.,-0.666550808889759,0.745459602640149));
#18414=DIRECTION('',(0.974370064785235,0.16769192358466,0.149941307233507));
#18415=DIRECTION('',(0.974370064785235,0.16769192358466,0.149941307233507));
#18416=DIRECTION('center_axis',(0.,-0.666550808889759,0.745459602640149));
#18417=DIRECTION('ref_axis',(-1.,0.,0.));
#18418=DIRECTION('',(1.23259516440783E-32,-0.745459602640149,-0.666550808889759));
#18419=DIRECTION('',(0.,0.745459602640149,0.666550808889759));
#18420=DIRECTION('center_axis',(0.,-0.666550808889759,0.745459602640149));
#18421=DIRECTION('ref_axis',(0.,0.745459602640149,0.666550808889759));
#18422=DIRECTION('',(-0.974370064785235,0.16769192358466,0.149941307233508));
#18423=DIRECTION('',(1.,4.50771793552549E-16,4.0305645343223E-16));
#18424=DIRECTION('center_axis',(0.,0.666550808889758,-0.745459602640149));
#18425=DIRECTION('ref_axis',(0.,0.745459602640149,0.666550808889758));
#18426=DIRECTION('center_axis',(0.,0.666550808889759,-0.745459602640149));
#18427=DIRECTION('ref_axis',(0.,0.745459602640149,0.666550808889759));
#18428=DIRECTION('',(0.,-0.666550808889759,0.745459602640149));
#18429=DIRECTION('center_axis',(0.,-0.666550808889759,0.745459602640149));
#18430=DIRECTION('ref_axis',(0.,0.745459602640149,0.666550808889759));
#18431=DIRECTION('center_axis',(0.,0.666550808889759,-0.745459602640149));
#18432=DIRECTION('ref_axis',(0.,0.745459602640149,0.666550808889759));
#18433=DIRECTION('center_axis',(0.918412615811027,0.263703427922986,-0.294921632337836));
#18434=DIRECTION('ref_axis',(0.395623896041616,-0.612168671944176,0.684639503659376));
#18435=DIRECTION('',(0.,-0.666550808889759,0.745459602640149));
#18436=DIRECTION('',(0.,-0.666550808889759,0.745459602640149));
#18437=DIRECTION('center_axis',(0.,-0.666550808889759,0.745459602640149));
#18438=DIRECTION('ref_axis',(-1.,0.,0.));
#18439=DIRECTION('center_axis',(0.,-0.666550808889759,0.745459602640149));
#18440=DIRECTION('ref_axis',(-1.,0.,0.));
#18441=DIRECTION('',(0.,0.745459602640149,0.666550808889759));
#18442=DIRECTION('',(1.23259516440783E-32,-0.745459602640149,-0.666550808889759));
#18443=DIRECTION('center_axis',(0.,0.666550808889758,-0.745459602640149));
#18444=DIRECTION('ref_axis',(0.,0.745459602640149,0.666550808889758));
#18445=DIRECTION('',(-1.,1.05200988229048E-32,8.90162208091945E-33));
#18446=DIRECTION('center_axis',(0.224951054343865,0.726353521319258,0.649467154840565));
#18447=DIRECTION('ref_axis',(0.877590614935324,-0.44064805168451,0.188849165007647));
#18448=DIRECTION('',(0.393983915184351,-0.677436825736628,0.621173101246256));
#18449=DIRECTION('',(-0.974370064785235,0.16769192358466,0.149941307233508));
#18450=DIRECTION('center_axis',(0.,-0.666550808889759,0.745459602640149));
#18451=DIRECTION('ref_axis',(-1.,0.,0.));
#18452=DIRECTION('',(9.16407275022627E-16,-0.745459602640149,-0.666550808889759));
#18453=DIRECTION('',(1.,4.50771793552549E-16,4.0305645343223E-16));
#18454=DIRECTION('',(3.25260651745651E-15,0.745459602640149,0.666550808889759));
#18455=DIRECTION('',(-1.,1.05200988229048E-32,8.90162208091945E-33));
#18456=DIRECTION('center_axis',(1.,0.,0.));
#18457=DIRECTION('ref_axis',(0.,-0.393919298579167,-0.919145030018058));
#18458=DIRECTION('center_axis',(0.,0.666550808889759,-0.745459602640149));
#18459=DIRECTION('ref_axis',(1.,0.,0.));
#18460=DIRECTION('center_axis',(1.,9.18849901475632E-33,8.21587303869647E-33));
#18461=DIRECTION('ref_axis',(5.20917225812029E-33,-0.919145030018058,0.393919298579167));
#18462=DIRECTION('',(0.,0.666550808889759,-0.745459602640149));
#18463=DIRECTION('center_axis',(0.,-0.666550808889758,0.745459602640149));
#18464=DIRECTION('ref_axis',(0.,-0.745459602640149,-0.666550808889758));
#18465=DIRECTION('',(0.,0.666550808889759,-0.745459602640149));
#18466=DIRECTION('center_axis',(0.918412615811012,0.263703427922711,-0.294921632338128));
#18467=DIRECTION('ref_axis',(0.39562389604165,-0.612168671963492,0.684639503642084));
#18468=DIRECTION('center_axis',(0.,-0.666550808889758,0.745459602640149));
#18469=DIRECTION('ref_axis',(0.,-0.745459602640149,-0.666550808889758));
#18470=DIRECTION('',(0.,0.666550808889759,-0.745459602640149));
#18471=DIRECTION('',(0.,0.666550808889759,-0.745459602640149));
#18472=DIRECTION('center_axis',(-1.37756920867255E-32,-0.745459602640149,
-0.666550808889759));
#18473=DIRECTION('ref_axis',(9.00587119577753E-49,-0.666550808889759,0.745459602640149));
#18474=DIRECTION('',(0.,0.666550808889759,-0.745459602640149));
#18475=DIRECTION('',(-1.,1.05200988229048E-32,8.90162208091945E-33));
#18476=DIRECTION('center_axis',(0.,-0.666550808889759,0.745459602640149));
#18477=DIRECTION('ref_axis',(-1.,0.,0.));
#18478=DIRECTION('center_axis',(-6.04689767166562E-16,0.745459602640149,
0.666550808889759));
#18479=DIRECTION('ref_axis',(1.,1.31512914729401E-15,-5.63626777411718E-16));
#18480=DIRECTION('',(0.395623896041664,-0.612168671963385,0.684639503642172));
#18481=DIRECTION('',(1.,4.50771793552549E-16,4.0305645343223E-16));
#18482=DIRECTION('',(0.,0.666550808889759,-0.745459602640149));
#18483=DIRECTION('center_axis',(-6.16297582203916E-33,0.666550808889759,
-0.745459602640149));
#18484=DIRECTION('ref_axis',(1.,-5.74446334377187E-33,-1.34037478021344E-32));
#18485=DIRECTION('',(3.25260651745651E-15,0.745459602640149,0.666550808889759));
#18486=DIRECTION('center_axis',(-1.,2.42468676204789E-15,2.16802750521074E-15));
#18487=DIRECTION('ref_axis',(-2.947862614937E-15,-0.393919298579167,-0.919145030018058));
#18488=DIRECTION('center_axis',(2.5018433889803E-15,0.745459602640149,0.666550808889759));
#18489=DIRECTION('ref_axis',(1.,-5.44121521723473E-15,2.33194937881488E-15));
#18490=DIRECTION('',(0.,0.666550808889759,-0.745459602640149));
#18491=DIRECTION('',(0.,0.666550808889759,-0.745459602640149));
#18492=DIRECTION('',(1.,-1.86502317861713E-15,-1.66760573464032E-15));
#18493=DIRECTION('center_axis',(0.,-0.666550808889759,0.745459602640149));
#18494=DIRECTION('ref_axis',(0.,-0.745459602640149,-0.666550808889759));
#18495=DIRECTION('',(0.,0.666550808889759,-0.745459602640149));
#18496=DIRECTION('center_axis',(0.,0.666550808889759,-0.745459602640149));
#18497=DIRECTION('ref_axis',(0.,0.745459602640149,0.666550808889759));
#18498=DIRECTION('center_axis',(1.,-2.69409640227544E-15,-2.40891945023415E-15));
#18499=DIRECTION('ref_axis',(-3.27540290548555E-15,-0.393919298579167,-0.919145030018058));
#18500=DIRECTION('',(0.,0.666550808889759,-0.745459602640149));
#18501=DIRECTION('',(-3.61400724161834E-15,-0.745459602640149,-0.666550808889759));
#18502=DIRECTION('center_axis',(0.,-0.666550808889759,0.745459602640149));
#18503=DIRECTION('ref_axis',(0.,-0.745459602640149,-0.666550808889759));
#18504=DIRECTION('',(0.,0.666550808889759,-0.745459602640149));
#18505=DIRECTION('center_axis',(0.,0.666550808889759,-0.745459602640149));
#18506=DIRECTION('ref_axis',(0.,0.745459602640149,0.666550808889759));
#18507=DIRECTION('center_axis',(-2.72485300195868E-15,-0.745459602640149,
-0.666550808889759));
#18508=DIRECTION('ref_axis',(1.46387489158228E-32,-0.666550808889759,0.745459602640149));
#18509=DIRECTION('',(0.,0.666550808889759,-0.745459602640149));
#18510=DIRECTION('',(-1.,2.03126783609293E-15,1.81625297256125E-15));
#18511=DIRECTION('center_axis',(0.,-0.666550808889759,0.745459602640149));
#18512=DIRECTION('ref_axis',(0.,-0.745459602640149,-0.666550808889759));
#18513=DIRECTION('',(0.,0.666550808889759,-0.745459602640149));
#18514=DIRECTION('center_axis',(0.,0.666550808889759,-0.745459602640149));
#18515=DIRECTION('ref_axis',(0.,0.745459602640149,0.666550808889759));
#18516=DIRECTION('center_axis',(0.,-0.666550808889759,0.745459602640149));
#18517=DIRECTION('ref_axis',(0.,-0.745459602640149,-0.666550808889759));
#18518=DIRECTION('',(0.,0.666550808889759,-0.745459602640149));
#18519=DIRECTION('center_axis',(0.,0.666550808889759,-0.745459602640149));
#18520=DIRECTION('ref_axis',(0.,-0.745459602640149,-0.666550808889759));
#18521=DIRECTION('center_axis',(-0.918412615811006,-0.26370342792269,0.294921632338166));
#18522=DIRECTION('ref_axis',(3.6676144219822E-17,0.745459602640148,0.66655080888976));
#18523=DIRECTION('center_axis',(1.,9.18849901475632E-33,8.21587303869647E-33));
#18524=DIRECTION('ref_axis',(5.20917225812029E-33,-0.919145030018058,0.393919298579167));
#18525=DIRECTION('center_axis',(-1.,1.34704820113771E-16,1.20445972511707E-16));
#18526=DIRECTION('ref_axis',(-1.63770145274277E-16,-0.393919298579167,-0.919145030018058));
#18527=DIRECTION('',(1.80700362080917E-16,0.745459602640149,0.666550808889759));
#18528=DIRECTION('',(1.80700362080917E-16,0.745459602640149,0.666550808889759));
#18529=DIRECTION('',(1.80700362080917E-16,0.745459602640149,0.666550808889759));
#18530=DIRECTION('center_axis',(1.,-2.15204789668062E-15,-1.92424815673669E-15));
#18531=DIRECTION('ref_axis',(-2.61639632775514E-15,-0.393919298579167,-0.919145030018058));
#18532=DIRECTION('',(2.88687393529957E-15,0.745459602640149,0.666550808889758));
#18533=DIRECTION('',(2.88687393529957E-15,0.745459602640149,0.666550808889758));
#18534=DIRECTION('center_axis',(-8.38164711797325E-31,0.666550808889758,
-0.745459602640149));
#18535=DIRECTION('ref_axis',(1.,-7.81247014752972E-31,-1.82290970109027E-30));
#18536=DIRECTION('center_axis',(2.48029812061751E-15,0.745459602640149,
0.666550808889758));
#18537=DIRECTION('ref_axis',(1.,-5.39435679172679E-15,2.31186719645433E-15));
#18538=DIRECTION('',(5.91645678915759E-31,-0.666550808889758,0.745459602640149));
#18539=DIRECTION('',(1.,-1.84896205142464E-15,-1.65324471858535E-15));
#18540=DIRECTION('',(5.91645678915759E-31,-0.666550808889758,0.745459602640149));
#18541=DIRECTION('',(-1.,1.84896205142464E-15,1.65324471858535E-15));
#18542=DIRECTION('center_axis',(4.95069485153125E-17,-0.745459602640149,
-0.666550808889758));
#18543=DIRECTION('ref_axis',(7.80070196304878E-34,-0.666550808889758,0.745459602640149));
#18544=DIRECTION('',(5.91645678915759E-31,-0.666550808889758,0.745459602640149));
#18545=DIRECTION('',(-1.,-3.69054301681519E-17,-3.29988965785444E-17));
#18546=DIRECTION('',(5.91645678915759E-31,-0.666550808889758,0.745459602640149));
#18547=DIRECTION('',(1.,3.69054301681518E-17,3.29988965785444E-17));
#18548=DIRECTION('center_axis',(-1.,3.2296864575908E-15,2.88781593683036E-15));
#18549=DIRECTION('ref_axis',(-3.92655748994937E-15,-0.393919298579167,-0.919145030018058));
#18550=DIRECTION('',(-4.33247683194691E-15,-0.745459602640149,-0.666550808889758));
#18551=DIRECTION('',(1.83098382774925E-15,-0.289055347086674,0.95731238700886));
#18552=DIRECTION('',(-4.33247683194691E-15,-0.745459602640149,-0.666550808889758));
#18553=DIRECTION('',(1.83098382774926E-15,0.919145030018058,-0.393919298579166));
#18554=DIRECTION('center_axis',(-4.48685329518507E-17,0.957312387008861,
0.289055347086674));
#18555=DIRECTION('ref_axis',(1.,2.74967668360758E-17,6.41591226175102E-17));
#18556=DIRECTION('',(-1.22004564440084E-15,0.289055347086674,-0.95731238700886));
#18557=DIRECTION('',(1.,3.69054301681519E-17,3.29988965785444E-17));
#18558=DIRECTION('center_axis',(-9.86076131526264E-31,0.666550808889758,
-0.745459602640149));
#18559=DIRECTION('ref_axis',(1.,-9.19114135003496E-31,-2.14459964834149E-30));
#18560=DIRECTION('',(2.88687393529957E-15,0.745459602640149,0.666550808889758));
#18561=DIRECTION('',(-1.,1.84896205142464E-15,1.65324471858535E-15));
#18562=DIRECTION('center_axis',(1.,-2.15204789668062E-15,-1.92424815673669E-15));
#18563=DIRECTION('ref_axis',(-2.61639632775514E-15,-0.393919298579167,-0.919145030018058));
#18564=DIRECTION('',(-1.22004564440084E-15,-0.919145030018058,0.393919298579166));
#18565=DIRECTION('',(2.88687393529957E-15,0.745459602640149,0.666550808889758));
#18566=DIRECTION('center_axis',(-6.73294499808336E-16,-0.745459602640149,
-0.666550808889758));
#18567=DIRECTION('ref_axis',(-4.59044537750992E-32,-0.666550808889758,0.745459602640149));
#18568=DIRECTION('',(5.91645678915759E-31,-0.666550808889758,0.745459602640149));
#18569=DIRECTION('',(1.,-5.01913850286919E-16,-4.48784993468272E-16));
#18570=DIRECTION('center_axis',(-1.,2.15204789668062E-15,1.92424815673669E-15));
#18571=DIRECTION('ref_axis',(-2.61639632775514E-15,-0.393919298579167,-0.919145030018058));
#18572=DIRECTION('',(-2.88687393529957E-15,-0.745459602640149,-0.666550808889758));
#18573=DIRECTION('center_axis',(-2.24791350088801E-15,-0.393919298579166,
-0.919145030018059));
#18574=DIRECTION('ref_axis',(-3.23063398772322E-32,-0.919145030018058,0.393919298579166));
#18575=DIRECTION('center_axis',(-6.16297582203916E-33,0.666550808889759,
-0.745459602640149));
#18576=DIRECTION('ref_axis',(1.,-5.74446334377187E-33,-1.34037478021344E-32));
#18577=DIRECTION('axis',(0.,0.,1.));
#18578=DIRECTION('refdir',(1.,0.,0.));
#18579=DIRECTION('center_axis',(1.,-6.12303176911189E-17,0.));
#18580=DIRECTION('ref_axis',(0.,1.,0.));
#18581=DIRECTION('center_axis',(-1.0241047919602E-18,-0.0167254528569715,
0.999860119830134));
#18582=DIRECTION('ref_axis',(1.,-1.71286164185289E-20,1.02396154000794E-18));
#18583=DIRECTION('center_axis',(-1.0241047919602E-18,-0.0167254528569715,
0.999860119830134));
#18584=DIRECTION('ref_axis',(1.,-1.71286164185289E-20,1.02396154000794E-18));
#18585=DIRECTION('center_axis',(-1.,6.12303176911189E-17,0.));
#18586=DIRECTION('ref_axis',(6.12303176911189E-17,1.,0.));
#18587=DIRECTION('center_axis',(0.,0.,-1.));
#18588=DIRECTION('ref_axis',(1.,0.,0.));
#18589=DIRECTION('center_axis',(0.,0.,-1.));
#18590=DIRECTION('ref_axis',(1.,0.,0.));
#18591=DIRECTION('center_axis',(0.,0.,-1.));
#18592=DIRECTION('ref_axis',(1.,0.,0.));
#18593=DIRECTION('center_axis',(0.,0.,-1.));
#18594=DIRECTION('ref_axis',(1.,0.,0.));
#18595=DIRECTION('center_axis',(1.,-6.12303176911189E-17,0.));
#18596=DIRECTION('ref_axis',(0.,1.,0.));
#18597=DIRECTION('center_axis',(-3.05385885637485E-31,2.44929359829471E-15,
-1.));
#18598=DIRECTION('ref_axis',(1.,7.47979694701453E-46,-3.05385885637485E-31));
#18599=DIRECTION('center_axis',(-3.05385885637485E-31,2.44929359829471E-15,
-1.));
#18600=DIRECTION('ref_axis',(1.,7.47979694701453E-46,-3.05385885637485E-31));
#18601=DIRECTION('center_axis',(-3.05385885637485E-31,2.44929359829471E-15,
-1.));
#18602=DIRECTION('ref_axis',(1.,7.47979694701453E-46,-3.05385885637485E-31));
#18603=DIRECTION('center_axis',(-3.05385885637485E-31,2.44929359829471E-15,
-1.));
#18604=DIRECTION('ref_axis',(1.,7.47979694701453E-46,-3.05385885637485E-31));
#18605=DIRECTION('center_axis',(-1.,6.12303176911189E-17,0.));
#18606=DIRECTION('ref_axis',(6.12303176911189E-17,1.,0.));
#18607=DIRECTION('center_axis',(2.02350164340122E-18,0.0330473810965473,
0.999453786126532));
#18608=DIRECTION('ref_axis',(1.,-6.68714299589699E-20,-2.02239637873061E-18));
#18609=DIRECTION('center_axis',(2.02350164340122E-18,0.0330473810965473,
0.999453786126532));
#18610=DIRECTION('ref_axis',(1.,-6.68714299589699E-20,-2.02239637873061E-18));
#18611=DIRECTION('center_axis',(-1.,6.12303176911189E-17,0.));
#18612=DIRECTION('ref_axis',(0.,-1.,0.));
#18613=DIRECTION('center_axis',(1.,-6.12303176911189E-17,0.));
#18614=DIRECTION('ref_axis',(-6.12303176911189E-17,-1.,0.));
#18615=DIRECTION('center_axis',(2.97215916777767E-17,0.485406458736823,
0.874288607850163));
#18616=DIRECTION('ref_axis',(1.,-1.44270525643314E-17,-2.59852490110544E-17));
#18617=DIRECTION('center_axis',(-1.,6.12303176911189E-17,0.));
#18618=DIRECTION('ref_axis',(0.,-1.,0.));
#18619=DIRECTION('center_axis',(-1.18600730662684E-17,-0.193696089020763,
0.981061580685973));
#18620=DIRECTION('ref_axis',(1.,-2.29724976843668E-18,1.16354620294444E-17));
#18621=DIRECTION('center_axis',(1.,-6.12303176911189E-17,0.));
#18622=DIRECTION('ref_axis',(-6.12303176911189E-17,-1.,0.));
#18623=DIRECTION('center_axis',(-1.,6.12303176911189E-17,0.));
#18624=DIRECTION('ref_axis',(0.,0.970124980364195,-0.242605693406751));
#18625=DIRECTION('center_axis',(2.97215916777766E-17,0.485406458736823,
0.874288607850164));
#18626=DIRECTION('ref_axis',(1.,-1.44270525643314E-17,-2.59852490110543E-17));
#18627=DIRECTION('center_axis',(1.,-6.12303176911189E-17,0.));
#18628=DIRECTION('ref_axis',(5.94010607477901E-17,0.970124980364195,-0.242605693406751));
#18629=DIRECTION('center_axis',(-1.,6.12303176911189E-17,0.));
#18630=DIRECTION('ref_axis',(0.,0.996726356556968,0.0808490577846839));
#18631=DIRECTION('center_axis',(1.,-6.12303176911189E-17,0.));
#18632=DIRECTION('ref_axis',(6.10298714630946E-17,0.996726356556968,0.0808490577846839));
#18633=DIRECTION('center_axis',(-1.18600730662684E-17,-0.193696089020763,
0.981061580685973));
#18634=DIRECTION('ref_axis',(1.,-2.29724976843668E-18,1.16354620294444E-17));
#18635=DIRECTION('center_axis',(1.,0.,0.));
#18636=DIRECTION('ref_axis',(0.,0.,-1.));
#18637=DIRECTION('center_axis',(1.,-6.12303176911189E-17,0.));
#18638=DIRECTION('ref_axis',(-6.12303176911189E-17,-1.,0.));
#18639=DIRECTION('',(-1.,0.,0.));
#18640=DIRECTION('center_axis',(1.,-6.12303176911189E-17,0.));
#18641=DIRECTION('ref_axis',(6.12303176911189E-17,1.,0.));
#18642=DIRECTION('center_axis',(1.,0.,0.));
#18643=DIRECTION('ref_axis',(0.,0.,1.));
#18644=DIRECTION('center_axis',(1.,0.,0.));
#18645=DIRECTION('ref_axis',(0.,0.,1.));
#18646=DIRECTION('center_axis',(1.,0.,0.));
#18647=DIRECTION('ref_axis',(0.,0.,1.));
#18648=DIRECTION('',(-0.707106781186548,-8.65956056235493E-17,0.707106781186547));
#18649=DIRECTION('center_axis',(-1.,6.12303176911189E-17,0.));
#18650=DIRECTION('ref_axis',(6.12303176911189E-17,1.,0.));
#18651=DIRECTION('center_axis',(1.,0.,0.));
#18652=DIRECTION('ref_axis',(0.,0.,-1.));
#18653=DIRECTION('center_axis',(-1.,6.12303176911189E-17,0.));
#18654=DIRECTION('ref_axis',(6.12303176911189E-17,1.,0.));
#18655=DIRECTION('center_axis',(-1.,6.12303176911189E-17,0.));
#18656=DIRECTION('ref_axis',(6.12303176911189E-17,1.,0.));
#18657=DIRECTION('',(-1.,0.,0.));
#18658=DIRECTION('center_axis',(-1.,6.12303176911189E-17,0.));
#18659=DIRECTION('ref_axis',(6.12303176911189E-17,1.,0.));
#18660=DIRECTION('center_axis',(1.,-6.12303176911189E-17,0.));
#18661=DIRECTION('ref_axis',(6.12303176911189E-17,1.,0.));
#18662=DIRECTION('',(-1.,6.12303176911189E-17,0.));
#18663=DIRECTION('center_axis',(-1.,6.12303176911189E-17,0.));
#18664=DIRECTION('ref_axis',(6.12303176911189E-17,1.,0.));
#18665=DIRECTION('',(-1.,3.93558242098606E-17,0.));
#18666=DIRECTION('center_axis',(1.,0.,0.));
#18667=DIRECTION('ref_axis',(0.,0.,-1.));
#18668=DIRECTION('',(1.,0.,0.));
#18669=DIRECTION('center_axis',(-1.,0.,0.));
#18670=DIRECTION('ref_axis',(0.,0.,1.));
#18671=DIRECTION('',(1.,-6.12303176911189E-17,0.));
#18672=DIRECTION('center_axis',(-1.,3.78429896776521E-17,0.));
#18673=DIRECTION('ref_axis',(-3.78429896776521E-17,-1.,0.));
#18674=DIRECTION('',(-1.,3.93558242098606E-17,0.));
#18675=DIRECTION('center_axis',(-1.,6.12303176911189E-17,0.));
#18676=DIRECTION('ref_axis',(6.12303176911189E-17,1.,0.));
#18677=DIRECTION('center_axis',(1.,-6.12303176911189E-17,0.));
#18678=DIRECTION('ref_axis',(6.12303176911189E-17,1.,0.));
#18679=DIRECTION('center_axis',(1.,-6.12303176911189E-17,0.));
#18680=DIRECTION('ref_axis',(-6.12303176911189E-17,-1.,0.));
#18681=DIRECTION('center_axis',(-1.,6.12303176911189E-17,0.));
#18682=DIRECTION('ref_axis',(-6.12303176911189E-17,-1.,0.));
#18683=DIRECTION('',(-1.,6.12303176911189E-17,0.));
#18684=DIRECTION('center_axis',(1.,-6.12303176911189E-17,0.));
#18685=DIRECTION('ref_axis',(6.12303176911189E-17,1.,0.));
#18686=DIRECTION('',(1.,-6.12303176911189E-17,0.));
#18687=DIRECTION('',(-1.,6.12303176911189E-17,0.));
#18688=DIRECTION('center_axis',(1.,-6.12303176911189E-17,0.));
#18689=DIRECTION('ref_axis',(6.12303176911189E-17,1.,0.));
#18690=DIRECTION('',(-1.,6.12303176911189E-17,0.));
#18691=DIRECTION('center_axis',(-1.,0.,0.));
#18692=DIRECTION('ref_axis',(0.,0.,-1.));
#18693=DIRECTION('',(-1.,6.12303176911189E-17,0.));
#18694=DIRECTION('center_axis',(1.,-6.12303176911189E-17,0.));
#18695=DIRECTION('ref_axis',(6.12303176911189E-17,1.,0.));
#18696=DIRECTION('center_axis',(1.,-6.12303176911189E-17,0.));
#18697=DIRECTION('ref_axis',(0.,1.,0.));
#18698=DIRECTION('center_axis',(1.,-6.12303176911189E-17,0.));
#18699=DIRECTION('ref_axis',(6.12303176911189E-17,1.,0.));
#18700=DIRECTION('center_axis',(7.49855125668918E-33,1.22464679907692E-16,
-1.));
#18701=DIRECTION('ref_axis',(0.,-1.,-1.22464679907692E-16));
#18702=DIRECTION('center_axis',(1.,-6.305873043676E-17,0.));
#18703=DIRECTION('ref_axis',(0.,1.,0.));
#18704=DIRECTION('center_axis',(1.,-6.305873043676E-17,0.));
#18705=DIRECTION('ref_axis',(6.305873043676E-17,1.,0.));
#18706=DIRECTION('center_axis',(-1.,6.305873043676E-17,0.));
#18707=DIRECTION('ref_axis',(6.305873043676E-17,1.,0.));
#18708=DIRECTION('center_axis',(1.,-6.305873043676E-17,0.));
#18709=DIRECTION('ref_axis',(0.,1.,0.));
#18710=DIRECTION('center_axis',(1.,-6.305873043676E-17,0.));
#18711=DIRECTION('ref_axis',(6.305873043676E-17,1.,0.));
#18712=DIRECTION('center_axis',(-1.,6.305873043676E-17,0.));
#18713=DIRECTION('ref_axis',(6.305873043676E-17,1.,0.));
#18714=DIRECTION('center_axis',(-1.,0.,0.));
#18715=DIRECTION('ref_axis',(0.,0.,1.));
#18716=DIRECTION('center_axis',(-1.,0.,0.));
#18717=DIRECTION('ref_axis',(0.,0.,-1.));
#18718=DIRECTION('',(-1.,0.,0.));
#18719=DIRECTION('center_axis',(1.,-6.12303176911189E-17,0.));
#18720=DIRECTION('ref_axis',(6.12303176911189E-17,1.,0.));
#18721=DIRECTION('',(1.,0.,0.));
#18722=DIRECTION('center_axis',(-1.,0.,0.));
#18723=DIRECTION('ref_axis',(0.,0.,1.));
#18724=DIRECTION('center_axis',(-1.,6.12303176911189E-17,0.));
#18725=DIRECTION('ref_axis',(6.12303176911189E-17,1.,0.));
#18726=DIRECTION('center_axis',(-1.,6.12303176911189E-17,0.));
#18727=DIRECTION('ref_axis',(6.12303176911189E-17,1.,0.));
#18728=DIRECTION('center_axis',(-0.707106781186543,-8.6003326957104E-14,
-0.707106781186552));
#18729=DIRECTION('ref_axis',(0.707106781186552,1.48735968909061E-10,-0.707106781186543));
#18730=DIRECTION('',(-1.,0.,0.));
#18731=DIRECTION('center_axis',(-1.,8.82754440022857E-17,0.));
#18732=DIRECTION('ref_axis',(-8.82754440022857E-17,-1.,0.));
#18733=DIRECTION('',(1.,0.,0.));
#18734=DIRECTION('center_axis',(1.,-6.12303176911189E-17,0.));
#18735=DIRECTION('ref_axis',(-6.12303176911189E-17,-1.,0.));
#18736=DIRECTION('',(-1.,6.12303176911189E-17,0.));
#18737=DIRECTION('center_axis',(-1.,0.,0.));
#18738=DIRECTION('ref_axis',(0.,0.,-1.));
#18739=DIRECTION('center_axis',(1.,-6.12303176911189E-17,0.));
#18740=DIRECTION('ref_axis',(0.,-0.933406972407284,0.358819486457282));
#18741=DIRECTION('center_axis',(1.,-6.12303176911189E-17,0.));
#18742=DIRECTION('ref_axis',(6.12303176911189E-17,1.,0.));
#18743=DIRECTION('center_axis',(1.,-6.12303176911189E-17,0.));
#18744=DIRECTION('ref_axis',(6.12303176911189E-17,1.,0.));
#18745=DIRECTION('center_axis',(1.,-6.12303176911189E-17,0.));
#18746=DIRECTION('ref_axis',(6.12303176911189E-17,1.,0.));
#18747=DIRECTION('center_axis',(0.,0.,-1.));
#18748=DIRECTION('ref_axis',(1.,0.,0.));
#18749=DIRECTION('center_axis',(0.,0.,1.));
#18750=DIRECTION('ref_axis',(1.,0.,0.));
#18751=DIRECTION('center_axis',(-1.,0.,0.));
#18752=DIRECTION('ref_axis',(0.,0.,-1.));
#18753=DIRECTION('center_axis',(0.,0.,-1.));
#18754=DIRECTION('ref_axis',(1.,0.,0.));
#18755=DIRECTION('center_axis',(1.,0.,0.));
#18756=DIRECTION('ref_axis',(0.,0.,1.));
#18757=DIRECTION('center_axis',(-1.,6.12303176911189E-17,0.));
#18758=DIRECTION('ref_axis',(0.,-1.,0.));
#18759=DIRECTION('center_axis',(-1.35958617011586E-32,-2.22044604925031E-16,
-1.));
#18760=DIRECTION('ref_axis',(0.,1.,-2.22044604925031E-16));
#18761=DIRECTION('center_axis',(1.,-6.12303176911189E-17,0.));
#18762=DIRECTION('ref_axis',(-6.12303176911189E-17,-1.,0.));
#18763=DIRECTION('center_axis',(0.,0.,-1.));
#18764=DIRECTION('ref_axis',(-1.,0.,0.));
#18765=DIRECTION('center_axis',(0.,0.,-1.));
#18766=DIRECTION('ref_axis',(1.,0.,0.));
#18767=DIRECTION('',(0.,0.,-1.));
#18768=DIRECTION('center_axis',(0.,0.,-1.));
#18769=DIRECTION('ref_axis',(-1.,0.,0.));
#18770=DIRECTION('center_axis',(1.,-6.12303176911189E-17,0.));
#18771=DIRECTION('ref_axis',(1.24734901031854E-17,0.20371428033591,-0.979030383587364));
#18772=DIRECTION('center_axis',(1.,0.,0.));
#18773=DIRECTION('ref_axis',(0.,0.,1.));
#18774=DIRECTION('center_axis',(1.,-6.37765983815004E-17,0.));
#18775=DIRECTION('ref_axis',(-6.37765983815004E-17,-1.,0.));
#18776=DIRECTION('',(-1.,6.12303176911189E-17,0.));
#18777=DIRECTION('center_axis',(-1.,6.305873043676E-17,0.));
#18778=DIRECTION('ref_axis',(6.305873043676E-17,1.,0.));
#18779=DIRECTION('',(-1.,3.93558242098606E-17,0.));
#18780=DIRECTION('',(-1.,3.93558242098606E-17,0.));
#18781=DIRECTION('center_axis',(-1.,0.,0.));
#18782=DIRECTION('ref_axis',(0.,0.,-1.));
#18783=DIRECTION('',(-1.,6.12303176911189E-17,0.));
#18784=DIRECTION('center_axis',(-0.707106781186548,-3.48206089692902E-16,
0.707106781186548));
#18785=DIRECTION('ref_axis',(0.707106781186547,7.42019951680791E-31,0.707106781186547));
#18786=DIRECTION('',(0.707106781186547,3.48206089692903E-16,-0.707106781186547));
#18787=DIRECTION('center_axis',(-0.707106781186547,-6.13317366673352E-16,
0.707106781186548));
#18788=DIRECTION('ref_axis',(-0.707106781186548,-1.21863909340796E-30,-0.707106781186547));
#18789=DIRECTION('center_axis',(-0.707106781186548,-6.13317366673348E-16,
0.707106781186548));
#18790=DIRECTION('ref_axis',(-0.707106781186548,-1.52186717178597E-30,-0.707106781186548));
#18791=DIRECTION('',(-0.707106781186547,-3.48206089692903E-16,0.707106781186547));
#18792=DIRECTION('center_axis',(-1.,6.12303176911189E-17,0.));
#18793=DIRECTION('ref_axis',(6.12303176911189E-17,1.,0.));
#18794=DIRECTION('center_axis',(1.,0.,0.));
#18795=DIRECTION('ref_axis',(0.,0.,1.));
#18796=DIRECTION('center_axis',(-1.,6.12303176911189E-17,0.));
#18797=DIRECTION('ref_axis',(6.12303176911189E-17,1.,0.));
#18798=DIRECTION('',(-1.,6.12303176911189E-17,0.));
#18799=DIRECTION('center_axis',(1.,-6.12303176911189E-17,0.));
#18800=DIRECTION('ref_axis',(0.,0.0945993501281125,0.995515425774678));
#18801=DIRECTION('center_axis',(-1.,6.12303176911189E-17,0.));
#18802=DIRECTION('ref_axis',(6.12303176911189E-17,1.,0.));
#18803=DIRECTION('center_axis',(0.,-0.206307963004919,-0.978487109981915));
#18804=DIRECTION('ref_axis',(0.,-0.978487109981915,0.206307963004919));
#18805=DIRECTION('center_axis',(1.,-6.12303176911189E-17,0.));
#18806=DIRECTION('ref_axis',(0.,1.,0.));
#18807=DIRECTION('center_axis',(-1.,6.12303176911189E-17,0.));
#18808=DIRECTION('ref_axis',(6.12303176911189E-17,1.,0.));
#18809=DIRECTION('center_axis',(1.,-8.55850097257312E-17,0.));
#18810=DIRECTION('ref_axis',(8.29584272353424E-17,0.969310250722573,-0.245840675731543));
#18811=DIRECTION('center_axis',(1.,-6.12303176911189E-17,0.));
#18812=DIRECTION('ref_axis',(6.12303176911189E-17,1.,0.));
#18813=DIRECTION('center_axis',(1.,-6.12303176911189E-17,0.));
#18814=DIRECTION('ref_axis',(6.12303176911189E-17,1.,0.));
#18815=DIRECTION('',(-1.,8.55850097257312E-17,0.));
#18816=DIRECTION('center_axis',(1.,0.,0.));
#18817=DIRECTION('ref_axis',(0.,0.,-1.));
#18818=DIRECTION('',(-1.,0.,0.));
#18819=DIRECTION('center_axis',(-1.,8.82766640598215E-17,0.));
#18820=DIRECTION('ref_axis',(-8.82766640598215E-17,-1.,0.));
#18821=DIRECTION('',(1.,-8.55850097257312E-17,0.));
#18822=DIRECTION('center_axis',(1.,0.,0.));
#18823=DIRECTION('ref_axis',(0.,0.,-1.));
#18824=DIRECTION('',(-1.,8.55850097257312E-17,0.));
#18825=DIRECTION('center_axis',(1.,-6.12303176911189E-17,0.));
#18826=DIRECTION('ref_axis',(6.12303176911189E-17,1.,0.));
#18827=DIRECTION('',(1.,-8.55850097257312E-17,0.));
#18828=DIRECTION('',(1.,-8.55850097257312E-17,0.));
#18829=DIRECTION('center_axis',(-0.894427190999916,0.420243315606445,-0.152956058030083));
#18830=DIRECTION('ref_axis',(0.425247203315731,0.90507724315229,5.35984724282349E-16));
#18831=DIRECTION('',(0.894427190999916,-0.420243315606445,0.152956058030083));
#18832=DIRECTION('center_axis',(0.948683298050566,0.297156898213485,-0.108156265856593));
#18833=DIRECTION('ref_axis',(0.316227766016682,-0.89147069465054,0.324468797543589));
#18834=DIRECTION('center_axis',(0.948683298050506,0.297156898213675,-0.108156265856598));
#18835=DIRECTION('ref_axis',(0.316227766016862,-0.89147069464147,0.324468797568334));
#18836=DIRECTION('',(-0.894427190999916,0.420243315606445,-0.152956058030083));
#18837=DIRECTION('center_axis',(1.,-6.12303176911189E-17,0.));
#18838=DIRECTION('ref_axis',(0.,1.,0.));
#18839=DIRECTION('center_axis',(-1.,6.12303176911189E-17,0.));
#18840=DIRECTION('ref_axis',(6.12303176911189E-17,1.,0.));
#18841=DIRECTION('center_axis',(0.,-0.301227558036465,0.953552283977857));
#18842=DIRECTION('ref_axis',(0.,0.953552283977857,0.301227558036465));
#18843=DIRECTION('center_axis',(1.,-6.12303176911189E-17,0.));
#18844=DIRECTION('ref_axis',(0.,1.,0.));
#18845=DIRECTION('center_axis',(-1.,6.12303176911189E-17,0.));
#18846=DIRECTION('ref_axis',(6.12303176911189E-17,1.,0.));
#18847=DIRECTION('center_axis',(1.,-6.12303176911189E-17,0.));
#18848=DIRECTION('ref_axis',(6.12303176911189E-17,1.,0.));
#18849=DIRECTION('center_axis',(1.,-6.12303176911189E-17,0.));
#18850=DIRECTION('ref_axis',(0.,1.,0.));
#18851=DIRECTION('center_axis',(-1.,6.12303176911189E-17,0.));
#18852=DIRECTION('ref_axis',(6.12303176911189E-17,1.,0.));
#18853=DIRECTION('center_axis',(1.,-6.12303176911189E-17,0.));
#18854=DIRECTION('ref_axis',(6.12303176911189E-17,1.,0.));
#18855=DIRECTION('center_axis',(0.191261891041587,-0.962950243082436,-0.190120273465704));
#18856=DIRECTION('ref_axis',(-6.86713994557681E-6,0.193694776232803,-0.98106183985158));
#18857=DIRECTION('center_axis',(-0.191881081657469,0.962831674217306,0.190096863798062));
#18858=DIRECTION('ref_axis',(3.99680288865059E-14,0.193696089020735,-0.981061580685979));
#18859=DIRECTION('center_axis',(0.00786589508707537,0.999969063368702,-1.88252157794132E-14));
#18860=DIRECTION('ref_axis',(-3.94970882666714E-7,3.10691472549253E-9,0.999999999999922));
#18861=DIRECTION('center_axis',(-0.00663612315024062,-0.999977980692342,
1.83917848476882E-13));
#18862=DIRECTION('ref_axis',(4.13457446057927E-8,-2.74198441729828E-10,
0.999999999999999));
#18863=DIRECTION('center_axis',(2.97215916777767E-17,0.485406458736824,
0.874288607850163));
#18864=DIRECTION('ref_axis',(1.08239046981355E-32,0.874288607850163,-0.485406458736824));
#18865=DIRECTION('',(-2.97215916777767E-17,-0.485406458736824,-0.874288607850163));
#18866=DIRECTION('center_axis',(-1.18600730662684E-17,-0.19369608902076,
0.981061580685974));
#18867=DIRECTION('ref_axis',(-2.11938170784821E-33,0.981061580685974,0.19369608902076));
#18868=DIRECTION('',(1.18600730662684E-17,0.19369608902076,-0.981061580685974));
#18869=DIRECTION('center_axis',(-1.18600730662687E-17,-0.193696089020763,
0.981061580685973));
#18870=DIRECTION('ref_axis',(-1.,6.12303176911196E-17,3.04400344543169E-34));
#18871=DIRECTION('center_axis',(-1.50855276528563E-32,-2.46373499627365E-16,
1.));
#18872=DIRECTION('ref_axis',(0.,-1.,-2.46373499627365E-16));
#18873=DIRECTION('center_axis',(1.,-6.12303176911189E-17,0.));
#18874=DIRECTION('ref_axis',(5.75556361012452E-17,0.939985913376917,0.341213250992636));
#18875=DIRECTION('',(-1.,6.12303176911189E-17,0.));
#18876=DIRECTION('',(1.,-6.12303176911189E-17,0.));
#18877=DIRECTION('center_axis',(2.64577897101399E-17,0.419573777126289,
0.907721237797144));
#18878=DIRECTION('ref_axis',(1.,-6.30587304367601E-17,-1.7798463758201E-33));
#18879=DIRECTION('',(-5.72397488459722E-17,-0.907721237797144,0.419573777126289));
#18880=DIRECTION('',(-1.,6.12303176911189E-17,0.));
#18881=DIRECTION('',(5.55800597652948E-17,0.907721237797144,-0.419573777126289));
#18882=DIRECTION('center_axis',(-2.64577897101398E-17,-0.419573777126288,
-0.907721237797145));
#18883=DIRECTION('ref_axis',(1.,-1.6659881145224E-34,-2.91474833995815E-17));
#18884=DIRECTION('',(5.72397488459722E-17,0.907721237797144,-0.419573777126288));
#18885=DIRECTION('',(1.,-6.305873043676E-17,0.));
#18886=DIRECTION('',(-5.55800597652948E-17,-0.907721237797144,0.419573777126288));
#18887=DIRECTION('center_axis',(-5.72397488459722E-17,-0.907721237797144,
0.419573777126289));
#18888=DIRECTION('ref_axis',(-1.,6.06873725410465E-33,-1.36423561162507E-16));
#18889=DIRECTION('',(1.,-6.305873043676E-17,0.));
#18890=DIRECTION('',(-2.64577897101398E-17,-0.419573777126289,-0.907721237797144));
#18891=DIRECTION('',(2.56906356683054E-17,0.419573777126289,0.907721237797144));
#18892=DIRECTION('center_axis',(5.72397488459722E-17,0.907721237797144,
-0.419573777126289));
#18893=DIRECTION('ref_axis',(-5.56772127245432E-34,-0.419573777126289,-0.907721237797144));
#18894=DIRECTION('',(1.,-6.12303176911189E-17,0.));
#18895=DIRECTION('',(2.64577897101398E-17,0.419573777126289,0.907721237797144));
#18896=DIRECTION('',(1.,-6.305873043676E-17,0.));
#18897=DIRECTION('',(-2.56906356683054E-17,-0.419573777126289,-0.907721237797144));
#18898=DIRECTION('center_axis',(2.64577897101398E-17,0.419573777126289,
0.907721237797144));
#18899=DIRECTION('ref_axis',(1.,-6.30587304367598E-17,4.62196821834101E-33));
#18900=DIRECTION('',(1.,-6.12303176911189E-17,0.));
#18901=DIRECTION('',(-5.72397488459722E-17,-0.907721237797144,0.419573777126289));
#18902=DIRECTION('',(1.,-6.305873043676E-17,0.));
#18903=DIRECTION('',(5.55800597652948E-17,0.907721237797144,-0.419573777126289));
#18904=DIRECTION('center_axis',(-2.64577897101398E-17,-0.419573777126289,
-0.907721237797144));
#18905=DIRECTION('ref_axis',(1.,7.16552847671617E-35,-2.91474833995815E-17));
#18906=DIRECTION('',(1.,-6.305873043676E-17,0.));
#18907=DIRECTION('',(5.72397488459722E-17,0.907721237797144,-0.419573777126289));
#18908=DIRECTION('',(-1.,6.12303176911189E-17,0.));
#18909=DIRECTION('',(-5.55800597652948E-17,-0.907721237797144,0.419573777126289));
#18910=DIRECTION('center_axis',(-7.16258653671378E-18,-1.,-4.9960036108132E-16));
#18911=DIRECTION('ref_axis',(-1.73759657126474E-49,4.9960036108132E-16,
-1.));
#18912=DIRECTION('',(3.05906888276069E-32,4.9960036108132E-16,-1.));
#18913=DIRECTION('center_axis',(-5.55800597652948E-17,-0.907721237797145,
0.419573777126288));
#18914=DIRECTION('ref_axis',(-8.12311769207607E-32,-0.419573777126288,-0.907721237797145));
#18915=DIRECTION('',(5.55800597652948E-17,0.907721237797144,-0.419573777126288));
#18916=DIRECTION('center_axis',(2.56906356683053E-17,0.419573777126289,
0.907721237797144));
#18917=DIRECTION('ref_axis',(-7.58956401293417E-33,-0.907721237797144,0.419573777126289));
#18918=DIRECTION('',(-2.56906356683053E-17,-0.419573777126289,-0.907721237797144));
#18919=DIRECTION('center_axis',(1.,-6.12303176911189E-17,0.));
#18920=DIRECTION('ref_axis',(0.,1.,0.));
#18921=DIRECTION('center_axis',(1.,-6.12303176911189E-17,0.));
#18922=DIRECTION('ref_axis',(6.12303176911189E-17,1.,0.));
#18923=DIRECTION('center_axis',(-1.,6.12303176911189E-17,0.));
#18924=DIRECTION('ref_axis',(6.12303176911189E-17,1.,0.));
#18925=DIRECTION('center_axis',(-2.56906356683053E-17,-0.419573777126289,
-0.907721237797144));
#18926=DIRECTION('ref_axis',(7.58956401293417E-33,0.907721237797144,-0.419573777126289));
#18927=DIRECTION('',(2.56906356683053E-17,0.419573777126289,0.907721237797144));
#18928=DIRECTION('center_axis',(-5.55800597652948E-17,-0.907721237797144,
0.419573777126289));
#18929=DIRECTION('ref_axis',(-1.29808072260833E-31,-0.419573777126289,-0.907721237797144));
#18930=DIRECTION('',(5.55800597652948E-17,0.907721237797144,-0.419573777126289));
#18931=DIRECTION('center_axis',(5.72397488459722E-17,0.907721237797145,
-0.419573777126288));
#18932=DIRECTION('ref_axis',(8.70154526560722E-32,0.419573777126288,0.907721237797145));
#18933=DIRECTION('',(-5.72397488459722E-17,-0.907721237797144,0.419573777126288));
#18934=DIRECTION('center_axis',(-2.64577897101398E-17,-0.419573777126289,
-0.907721237797144));
#18935=DIRECTION('ref_axis',(9.2001233786812E-33,0.907721237797144,-0.419573777126289));
#18936=DIRECTION('',(2.64577897101398E-17,0.419573777126289,0.907721237797144));
#18937=DIRECTION('center_axis',(1.,-6.305873043676E-17,0.));
#18938=DIRECTION('ref_axis',(0.,1.,0.));
#18939=DIRECTION('center_axis',(-1.,6.305873043676E-17,0.));
#18940=DIRECTION('ref_axis',(6.305873043676E-17,1.,0.));
#18941=DIRECTION('center_axis',(1.,-6.305873043676E-17,0.));
#18942=DIRECTION('ref_axis',(6.305873043676E-17,1.,0.));
#18943=DIRECTION('center_axis',(1.,-6.305873043676E-17,0.));
#18944=DIRECTION('ref_axis',(0.,1.,0.));
#18945=DIRECTION('center_axis',(0.,1.,0.));
#18946=DIRECTION('ref_axis',(0.,0.,-1.));
#18947=DIRECTION('center_axis',(1.,-6.305873043676E-17,0.));
#18948=DIRECTION('ref_axis',(6.305873043676E-17,1.,0.));
#18949=DIRECTION('center_axis',(0.,0.525870255519711,-0.85056479727275));
#18950=DIRECTION('ref_axis',(0.,-0.85056479727275,-0.525870255519711));
#18951=DIRECTION('center_axis',(-1.,6.305873043676E-17,0.));
#18952=DIRECTION('ref_axis',(6.305873043676E-17,1.,0.));
#18953=DIRECTION('center_axis',(6.305873043676E-17,1.,-1.71170019451462E-16));
#18954=DIRECTION('ref_axis',(1.07937641154447E-32,1.71170019451462E-16,
1.));
#18955=DIRECTION('',(-6.305873043676E-17,-1.,1.71170019451462E-16));
#18956=DIRECTION('',(6.305873043676E-17,1.,-1.71170019451462E-16));
#18957=DIRECTION('center_axis',(-1.,8.82754440022857E-17,0.));
#18958=DIRECTION('ref_axis',(8.82754440022857E-17,1.,0.));
#18959=DIRECTION('center_axis',(1.,-8.82754440022857E-17,0.));
#18960=DIRECTION('ref_axis',(-8.82754440022857E-17,-1.,0.));
#18961=DIRECTION('',(8.82754440022857E-17,1.,0.));
#18962=DIRECTION('',(-1.3611865338937E-31,-1.5419764230905E-15,-1.));
#18963=DIRECTION('',(-8.82754440022857E-17,-1.,0.));
#18964=DIRECTION('center_axis',(-0.948683298050517,3.48666447216684E-15,
-0.316227766016828));
#18965=DIRECTION('ref_axis',(0.316227766016828,3.38856734140111E-13,-0.948683298050517));
#18966=DIRECTION('center_axis',(0.,-1.,0.));
#18967=DIRECTION('ref_axis',(0.,0.,1.));
#18968=DIRECTION('center_axis',(-1.,0.,0.));
#18969=DIRECTION('ref_axis',(0.,1.96105308347356E-6,-0.999999999998077));
#18970=DIRECTION('center_axis',(-6.12303176911189E-17,-1.,-6.16297582203916E-33));
#18971=DIRECTION('ref_axis',(-1.,6.12303176911189E-17,3.77360967506142E-49));
#18972=DIRECTION('',(-6.12303176911189E-17,-1.,-5.89862595156241E-33));
#18973=DIRECTION('center_axis',(0.,-1.,0.));
#18974=DIRECTION('ref_axis',(0.,0.,1.));
#18975=DIRECTION('',(6.12303176911189E-17,1.,6.16297582203916E-33));
#18976=DIRECTION('center_axis',(-0.707106781204563,-5.65566764166261E-12,
-0.707106781168532));
#18977=DIRECTION('ref_axis',(0.673256666820156,0.305697433935813,-0.673256666856907));
#18978=DIRECTION('center_axis',(-0.707106781186548,4.32963728535968E-17,
-0.707106781186548));
#18979=DIRECTION('ref_axis',(2.30001377051388E-33,1.,6.12303176911189E-17));
#18980=DIRECTION('',(0.707106781186547,-6.05177407449811E-17,-0.707106781186547));
#18981=DIRECTION('',(-6.12303176911189E-17,-1.,0.));
#18982=DIRECTION('center_axis',(8.55850097257312E-17,1.,0.));
#18983=DIRECTION('ref_axis',(1.,-8.55850097257312E-17,0.));
#18984=DIRECTION('',(-0.707106781186547,6.05177407449811E-17,0.707106781186547));
#18985=DIRECTION('',(0.,0.,-1.));
#18986=DIRECTION('',(-1.,8.55850097257312E-17,0.));
#18987=DIRECTION('',(0.,0.,1.));
#18988=DIRECTION('',(-1.,8.55850097257312E-17,0.));
#18989=DIRECTION('center_axis',(7.16258653671378E-18,1.,4.9960036108132E-16));
#18990=DIRECTION('ref_axis',(1.,-7.16258653671378E-18,0.));
#18991=DIRECTION('',(-3.05906888276069E-32,-4.9960036108132E-16,1.));
#18992=DIRECTION('center_axis',(1.,-6.12303176911189E-17,0.));
#18993=DIRECTION('ref_axis',(0.,-0.357902634963279,-0.93375891100773));
#18994=DIRECTION('center_axis',(-1.,6.12303176911189E-17,0.));
#18995=DIRECTION('ref_axis',(6.12303176911189E-17,1.,0.));
#18996=DIRECTION('center_axis',(0.,0.939692620785909,-0.342020143325668));
#18997=DIRECTION('ref_axis',(0.,-0.342020143325668,-0.939692620785909));
#18998=DIRECTION('center_axis',(0.,-0.939692620785909,0.342020143325668));
#18999=DIRECTION('ref_axis',(0.,-0.342020143325668,-0.939692620785909));
#19000=DIRECTION('',(0.,0.342020143325668,0.939692620785909));
#19001=DIRECTION('center_axis',(0.,-0.939692620785909,0.342020143325668));
#19002=DIRECTION('ref_axis',(0.,-0.342020143325668,-0.939692620785909));
#19003=DIRECTION('',(0.,0.342020143325668,0.939692620785909));
#19004=DIRECTION('center_axis',(0.,0.342020143325668,0.939692620785909));
#19005=DIRECTION('ref_axis',(1.,0.,0.));
#19006=DIRECTION('',(-5.75376777027213E-17,-0.939692620785909,0.342020143325668));
#19007=DIRECTION('center_axis',(0.,0.342020143325668,0.939692620785909));
#19008=DIRECTION('ref_axis',(1.,0.,0.));
#19009=DIRECTION('',(5.75376777027213E-17,0.939692620785909,-0.342020143325668));
#19010=DIRECTION('center_axis',(0.,0.342020143325668,0.939692620785909));
#19011=DIRECTION('ref_axis',(1.,0.,0.));
#19012=DIRECTION('',(-5.75376777027213E-17,-0.939692620785909,0.342020143325668));
#19013=DIRECTION('',(0.894427190999916,0.420243315606445,-0.152956058030083));
#19014=DIRECTION('center_axis',(1.,-6.12303176911189E-17,0.));
#19015=DIRECTION('ref_axis',(0.,1.,0.));
#19016=DIRECTION('center_axis',(-6.6521838836082E-15,0.843685290277401,
0.536838086362674));
#19017=DIRECTION('ref_axis',(1.87310260347094E-29,0.536838086362674,-0.843685290277401));
#19018=DIRECTION('center_axis',(-1.,6.12303176911189E-17,0.));
#19019=DIRECTION('ref_axis',(6.12303176911189E-17,1.,0.));
#19020=DIRECTION('center_axis',(-5.75376777027213E-17,-0.939692620785909,
0.342020143325668));
#19021=DIRECTION('ref_axis',(8.8935491616808E-32,-0.342020143325668,-0.939692620785909));
#19022=DIRECTION('',(5.75376777027213E-17,0.939692620785909,-0.342020143325668));
#19023=DIRECTION('center_axis',(7.4313463805646E-16,0.939692620785909,-0.342020143325667));
#19024=DIRECTION('ref_axis',(1.85564127880603E-30,-0.342020143325667,-0.939692620785909));
#19025=DIRECTION('center_axis',(0.948683298050523,-0.297156898213624,0.108156265856586));
#19026=DIRECTION('ref_axis',(0.316227766016811,0.891470694640734,-0.324468797570405));
#19027=DIRECTION('center_axis',(-1.,-2.35521515975489E-13,-5.36913090858677E-14));
#19028=DIRECTION('ref_axis',(-2.02953649309067E-13,0.939690866223616,-0.342024963907476));
#19029=DIRECTION('center_axis',(0.894427190999916,0.420243315606445,-0.152956058030083));
#19030=DIRECTION('ref_axis',(0.425247203315731,-0.90507724315229,-5.35984724282349E-16));
#19031=DIRECTION('',(-0.894427190999916,-0.420243315606445,0.152956058030083));
#19032=DIRECTION('center_axis',(5.75376777027213E-17,0.939692620785909,
-0.342020143325668));
#19033=DIRECTION('ref_axis',(-8.8935491616808E-32,0.342020143325668,0.939692620785909));
#19034=DIRECTION('center_axis',(0.,-0.939692620785909,0.342020143325668));
#19035=DIRECTION('ref_axis',(0.,0.342020143325668,0.939692620785909));
#19036=DIRECTION('',(5.75376777027213E-17,0.939692620785909,-0.342020143325668));
#19037=DIRECTION('center_axis',(-1.,-1.10682065829975E-15,2.76579965799101E-15));
#19038=DIRECTION('ref_axis',(-1.98603300901544E-15,0.9396922190012,-0.342021247218065));
#19039=DIRECTION('center_axis',(-5.75376777027213E-17,-0.939692620785909,
0.342020143325668));
#19040=DIRECTION('ref_axis',(8.8935491616808E-32,-0.342020143325668,-0.939692620785909));
#19041=DIRECTION('',(-5.75376777027213E-17,-0.939692620785909,0.342020143325668));
#19042=DIRECTION('center_axis',(-1.,6.12303176911189E-17,0.));
#19043=DIRECTION('ref_axis',(6.12303176911189E-17,1.,0.));
#19044=DIRECTION('center_axis',(-1.,8.82766640598215E-17,0.));
#19045=DIRECTION('ref_axis',(8.82766640598215E-17,1.,0.));
#19046=DIRECTION('center_axis',(1.,-8.82766640598215E-17,0.));
#19047=DIRECTION('ref_axis',(-8.82766640598215E-17,-1.,0.));
#19048=DIRECTION('center_axis',(1.,-6.12303176911189E-17,0.));
#19049=DIRECTION('ref_axis',(0.,1.,0.));
#19050=DIRECTION('center_axis',(1.,-6.12303176911189E-17,0.));
#19051=DIRECTION('ref_axis',(6.12303176911189E-17,1.,0.));
#19052=DIRECTION('center_axis',(-3.98057119674385E-15,0.902145193524675,
-0.431432555332032));
#19053=DIRECTION('ref_axis',(2.30883845873134E-29,-0.431432555332032,-0.902145193524675));
#19054=DIRECTION('center_axis',(1.,-6.12303176911189E-17,0.));
#19055=DIRECTION('ref_axis',(0.,-0.679936320676586,0.733271163911951));
#19056=DIRECTION('center_axis',(1.,-6.12303176911189E-17,0.));
#19057=DIRECTION('ref_axis',(6.12303176911189E-17,1.,0.));
#19058=DIRECTION('center_axis',(0.,0.968402813368906,-0.249391240943199));
#19059=DIRECTION('ref_axis',(0.,-0.249391240943199,-0.968402813368906));
#19060=DIRECTION('center_axis',(1.,-6.12303176911189E-17,0.));
#19061=DIRECTION('ref_axis',(0.,1.,0.));
#19062=DIRECTION('center_axis',(-1.,6.12303176911189E-17,0.));
#19063=DIRECTION('ref_axis',(6.12303176911189E-17,1.,0.));
#19064=DIRECTION('center_axis',(-5.63595351442503E-15,0.673655460688034,
0.739045546827253));
#19065=DIRECTION('ref_axis',(-8.67000511622114E-30,0.739045546827253,-0.673655460688034));
#19066=DIRECTION('center_axis',(3.05906888276069E-32,4.9960036108132E-16,
-1.));
#19067=DIRECTION('ref_axis',(-3.06415924378128E-57,1.,4.9960036108132E-16));
#19068=DIRECTION('',(3.05906888276069E-32,4.9960036108132E-16,-1.));
#19069=DIRECTION('center_axis',(0.894427190999906,-4.00966414299127E-14,
0.447213595499978));
#19070=DIRECTION('ref_axis',(0.447213595499978,4.85406311470918E-13,-0.894427190999906));
#19071=DIRECTION('center_axis',(-1.,0.,0.));
#19072=DIRECTION('ref_axis',(0.,0.112528245522859,0.993648526371145));
#19073=DIRECTION('center_axis',(-1.,0.,0.));
#19074=DIRECTION('ref_axis',(0.,0.,-1.));
#19075=DIRECTION('center_axis',(-1.,0.,0.));
#19076=DIRECTION('ref_axis',(0.,0.,-1.));
#19077=DIRECTION('center_axis',(1.,-6.12303176911189E-17,0.));
#19078=DIRECTION('ref_axis',(-6.12303176911189E-17,-1.,0.));
#19079=DIRECTION('',(-1.,6.12303176911189E-17,0.));
#19080=DIRECTION('center_axis',(1.,-6.305873043676E-17,0.));
#19081=DIRECTION('ref_axis',(6.305873043676E-17,1.,0.));
#19082=DIRECTION('',(1.,-6.12303176911189E-17,0.));
#19083=DIRECTION('center_axis',(-1.,6.12303176911189E-17,0.));
#19084=DIRECTION('ref_axis',(6.12303176911189E-17,1.,0.));
#19085=DIRECTION('center_axis',(1.89956701267235E-32,3.10233081307019E-16,
1.));
#19086=DIRECTION('ref_axis',(0.,1.,-3.10233081307019E-16));
#19087=DIRECTION('',(-1.,6.12303176911189E-17,0.));
#19088=DIRECTION('',(6.305873043676E-17,1.,-3.10233081307019E-16));
#19089=DIRECTION('',(-6.12303176911189E-17,-1.,3.10233081307019E-16));
#19090=DIRECTION('center_axis',(1.,-6.305873043676E-17,0.));
#19091=DIRECTION('ref_axis',(0.,1.,0.));
#19092=DIRECTION('center_axis',(-1.,6.305873043676E-17,0.));
#19093=DIRECTION('ref_axis',(6.305873043676E-17,1.,0.));
#19094=DIRECTION('center_axis',(0.,0.873412217959863,0.486981619281912));
#19095=DIRECTION('ref_axis',(0.,0.486981619281912,-0.873412217959863));
#19096=DIRECTION('center_axis',(1.,-6.12303176911189E-17,0.));
#19097=DIRECTION('ref_axis',(-6.12303176911189E-17,-1.,0.));
#19098=DIRECTION('center_axis',(-1.,6.305873043676E-17,0.));
#19099=DIRECTION('ref_axis',(6.305873043676E-17,1.,0.));
#19100=DIRECTION('center_axis',(-1.,6.12303176911189E-17,0.));
#19101=DIRECTION('ref_axis',(6.12303176911189E-17,1.,0.));
#19102=DIRECTION('center_axis',(-1.,0.,0.));
#19103=DIRECTION('ref_axis',(0.,0.,1.));
#19104=DIRECTION('',(1.,-6.12303176911189E-17,0.));
#19105=DIRECTION('center_axis',(-1.,6.12303176911189E-17,0.));
#19106=DIRECTION('ref_axis',(6.12303176911189E-17,1.,0.));
#19107=DIRECTION('center_axis',(-1.,0.,0.));
#19108=DIRECTION('ref_axis',(0.,0.,1.));
#19109=DIRECTION('center_axis',(1.,-6.12303176911189E-17,0.));
#19110=DIRECTION('ref_axis',(-6.12303176911189E-17,-1.,0.));
#19111=DIRECTION('',(1.,-6.12303176911189E-17,0.));
#19112=DIRECTION('center_axis',(-1.,6.12303176911189E-17,0.));
#19113=DIRECTION('ref_axis',(6.12303176911189E-17,1.,0.));
#19114=DIRECTION('center_axis',(1.65126718156494E-17,0.419573777126287,
0.907721237797145));
#19115=DIRECTION('ref_axis',(1.,-3.93558242098606E-17,1.53156320849217E-33));
#19116=DIRECTION('',(3.4350885432143E-17,0.907721237797145,-0.419573777126287));
#19117=DIRECTION('',(3.4350885432143E-17,0.907721237797145,-0.419573777126287));
#19118=DIRECTION('center_axis',(-1.,3.78429896776521E-17,0.));
#19119=DIRECTION('ref_axis',(3.78429896776521E-17,1.,0.));
#19120=DIRECTION('',(0.,-0.882947592858927,0.469471562785891));
#19121=DIRECTION('center_axis',(-8.55850097257312E-17,-1.,1.54197642309049E-15));
#19122=DIRECTION('ref_axis',(9.35280776177934E-48,-1.54197642309049E-15,
-1.));
#19123=DIRECTION('',(1.3611865338937E-31,1.5419764230905E-15,1.));
#19124=DIRECTION('',(1.,-8.55850097257312E-17,0.));
#19125=DIRECTION('',(-1.3611865338937E-31,-1.5419764230905E-15,-1.));
#19126=DIRECTION('',(-1.,8.55850097257312E-17,0.));
#19127=DIRECTION('center_axis',(8.68731872386614E-33,1.37765518964554E-16,
1.));
#19128=DIRECTION('ref_axis',(0.,1.,-1.37765518964554E-16));
#19129=DIRECTION('',(1.,-6.12303176911189E-17,0.));
#19130=DIRECTION('',(-6.305873043676E-17,-1.,1.37765518964554E-16));
#19131=DIRECTION('',(1.,0.,0.));
#19132=DIRECTION('',(0.,1.,-1.33305621742574E-16));
#19133=DIRECTION('',(-1.,1.1968129724039E-48,8.68731872386614E-33));
#19134=DIRECTION('',(6.12303176911189E-17,1.,-1.37765518964554E-16));
#19135=DIRECTION('center_axis',(-3.05906888276069E-32,-4.9960036108132E-16,
1.));
#19136=DIRECTION('ref_axis',(3.06415924378128E-57,-1.,-4.9960036108132E-16));
#19137=DIRECTION('center_axis',(0.894431478679542,-2.13240231356641E-5,
0.447205019529537));
#19138=DIRECTION('ref_axis',(0.447205018870395,-2.96107870526001E-5,-0.894431478773154));
#19139=DIRECTION('',(-3.05906888276069E-32,-4.9960036108132E-16,1.));
#19140=DIRECTION('center_axis',(-0.707106780946326,8.56130761774713E-10,
-0.707106781426769));
#19141=DIRECTION('ref_axis',(0.707106553895062,-0.000802219031349341,-0.707106553415591));
#19142=DIRECTION('center_axis',(-0.707106780941704,-8.72599632391827E-10,
-0.707106781431391));
#19143=DIRECTION('ref_axis',(0.707106548468998,0.000811736179642942,-0.707106547980313));
#19144=DIRECTION('center_axis',(-5.72397488459722E-17,-0.907721237797144,
0.419573777126289));
#19145=DIRECTION('ref_axis',(-1.1368799380976E-31,-0.419573777126289,-0.907721237797144));
#19146=DIRECTION('',(5.72397488459722E-17,0.907721237797144,-0.419573777126289));
#19147=DIRECTION('center_axis',(1.,-6.305873043676E-17,0.));
#19148=DIRECTION('ref_axis',(0.,1.,0.));
#19149=DIRECTION('center_axis',(1.,-6.305873043676E-17,0.));
#19150=DIRECTION('ref_axis',(6.305873043676E-17,1.,0.));
#19151=DIRECTION('center_axis',(-6.305873043676E-17,-1.,3.10233081307019E-16));
#19152=DIRECTION('ref_axis',(1.95629042467048E-32,3.10233081307019E-16,
1.));
#19153=DIRECTION('center_axis',(1.,-6.305873043676E-17,0.));
#19154=DIRECTION('ref_axis',(0.,-0.991300262557005,-0.131619867248123));
#19155=DIRECTION('center_axis',(0.,-0.512782925680917,0.858518299822502));
#19156=DIRECTION('ref_axis',(0.,0.858518299822502,0.512782925680917));
#19157=DIRECTION('center_axis',(1.,-6.305873043676E-17,0.));
#19158=DIRECTION('ref_axis',(6.305873043676E-17,1.,0.));
#19159=DIRECTION('center_axis',(6.305873043676E-17,1.,-3.10233081307019E-16));
#19160=DIRECTION('ref_axis',(1.95629042467048E-32,3.10233081307019E-16,
1.));
#19161=DIRECTION('',(-6.305873043676E-17,-1.,3.10233081307019E-16));
#19162=DIRECTION('center_axis',(1.,-6.12303176911189E-17,0.));
#19163=DIRECTION('ref_axis',(-6.12303176911189E-17,-1.,0.));
#19164=DIRECTION('center_axis',(1.,-6.37765983815004E-17,0.));
#19165=DIRECTION('ref_axis',(-6.37765983815004E-17,-1.,0.));
#19166=DIRECTION('center_axis',(-1.,0.,0.));
#19167=DIRECTION('ref_axis',(0.,0.,-1.));
#19168=DIRECTION('center_axis',(1.,-6.12303176911189E-17,0.));
#19169=DIRECTION('ref_axis',(0.,-0.855521656752581,-0.517767027559035));
#19170=DIRECTION('center_axis',(1.,-6.12303176911189E-17,0.));
#19171=DIRECTION('ref_axis',(6.12303176911189E-17,1.,0.));
#19172=DIRECTION('center_axis',(1.,-6.12303176911189E-17,0.));
#19173=DIRECTION('ref_axis',(6.12303176911189E-17,1.,0.));
#19174=DIRECTION('center_axis',(1.,0.,0.));
#19175=DIRECTION('ref_axis',(0.,0.,1.));
#19176=DIRECTION('center_axis',(1.,0.,0.));
#19177=DIRECTION('ref_axis',(0.,0.,1.));
#19178=DIRECTION('center_axis',(1.,0.,0.));
#19179=DIRECTION('ref_axis',(0.,0.,1.));
#19180=DIRECTION('',(0.,-0.882947592858927,0.469471562785891));
#19181=DIRECTION('center_axis',(1.,-6.12303176911189E-17,0.));
#19182=DIRECTION('ref_axis',(0.,0.,1.));
#19183=DIRECTION('',(-5.55800597652948E-17,-0.907721237797144,0.419573777126289));
#19184=DIRECTION('center_axis',(-1.,6.12303176911189E-17,0.));
#19185=DIRECTION('ref_axis',(6.12303176911189E-17,1.,0.));
#19186=DIRECTION('',(-6.12303176911189E-17,-1.,1.37765518964554E-16));
#19187=DIRECTION('',(6.12303176911189E-17,1.,1.13606963518701E-16));
#19188=DIRECTION('center_axis',(1.,-6.305873043676E-17,0.));
#19189=DIRECTION('ref_axis',(-6.305873043676E-17,-1.,0.));
#19190=DIRECTION('',(-5.55800597652948E-17,-0.907721237797144,0.419573777126289));
#19191=DIRECTION('center_axis',(1.,-6.12303176911189E-17,0.));
#19192=DIRECTION('ref_axis',(6.12303176911189E-17,1.,0.));
#19193=DIRECTION('center_axis',(-1.,6.12303176911189E-17,0.));
#19194=DIRECTION('ref_axis',(6.12303176911189E-17,1.,0.));
#19195=DIRECTION('center_axis',(0.,0.,1.));
#19196=DIRECTION('ref_axis',(-1.,0.,0.));
#19197=DIRECTION('center_axis',(0.,0.,-1.));
#19198=DIRECTION('ref_axis',(-1.,0.,0.));
#19199=DIRECTION('center_axis',(0.,0.,-1.));
#19200=DIRECTION('ref_axis',(-1.,0.,0.));
#19201=DIRECTION('',(8.82754440022857E-17,1.,0.));
#19202=DIRECTION('center_axis',(1.,-6.305873043676E-17,0.));
#19203=DIRECTION('ref_axis',(0.,0.,1.));
#19204=DIRECTION('center_axis',(1.,-6.12303176911189E-17,0.));
#19205=DIRECTION('ref_axis',(-6.12303176911189E-17,-1.,0.));
#19206=DIRECTION('center_axis',(1.,-6.305873043676E-17,0.));
#19207=DIRECTION('ref_axis',(6.305873043676E-17,1.,0.));
#19208=DIRECTION('center_axis',(1.,-6.12303176911189E-17,0.));
#19209=DIRECTION('ref_axis',(-6.12303176911189E-17,-1.,0.));
#19210=DIRECTION('center_axis',(1.,-6.305873043676E-17,0.));
#19211=DIRECTION('ref_axis',(6.305873043676E-17,1.,0.));
#19212=DIRECTION('',(1.,-6.305873043676E-17,0.));
#19213=DIRECTION('center_axis',(-1.,6.12303176911189E-17,0.));
#19214=DIRECTION('ref_axis',(6.12303176911189E-17,1.,0.));
#19215=DIRECTION('center_axis',(1.,-6.305873043676E-17,0.));
#19216=DIRECTION('ref_axis',(0.,0.,1.));
#19217=DIRECTION('',(6.50521303491303E-17,0.882947592858927,-0.469471562785891));
#19218=DIRECTION('center_axis',(-1.,0.,0.));
#19219=DIRECTION('ref_axis',(0.,0.,-1.));
#19220=DIRECTION('',(6.305873043676E-17,1.,-1.37765518964554E-16));
#19221=DIRECTION('center_axis',(1.,-6.305873043676E-17,0.));
#19222=DIRECTION('ref_axis',(6.305873043676E-17,1.,0.));
#19223=DIRECTION('center_axis',(1.,-6.305873043676E-17,0.));
#19224=DIRECTION('ref_axis',(0.,0.,1.));
#19225=DIRECTION('',(-2.64577897101398E-17,-0.419573777126289,-0.907721237797144));
#19226=DIRECTION('center_axis',(1.,-6.305873043676E-17,0.));
#19227=DIRECTION('ref_axis',(6.305873043676E-17,1.,0.));
#19228=DIRECTION('',(-5.72397488459722E-17,-0.907721237797144,0.419573777126289));
#19229=DIRECTION('center_axis',(-1.,6.305873043676E-17,0.));
#19230=DIRECTION('ref_axis',(6.305873043676E-17,1.,0.));
#19231=DIRECTION('center_axis',(1.,-6.305873043676E-17,0.));
#19232=DIRECTION('ref_axis',(0.,0.,1.));
#19233=DIRECTION('',(-6.305873043676E-17,-1.,-1.13606963518701E-16));
#19234=DIRECTION('center_axis',(-1.,6.305873043676E-17,0.));
#19235=DIRECTION('ref_axis',(6.305873043676E-17,1.,0.));
#19236=DIRECTION('',(5.72397488459722E-17,0.907721237797144,-0.419573777126289));
#19237=DIRECTION('center_axis',(7.16391088826457E-33,1.13606963518701E-16,
-1.));
#19238=DIRECTION('ref_axis',(0.,1.,1.13606963518701E-16));
#19239=DIRECTION('',(6.305873043676E-17,1.,1.13606963518701E-16));
#19240=DIRECTION('',(-1.,6.12303176911189E-17,0.));
#19241=DIRECTION('',(-6.12303176911189E-17,-1.,-1.13606963518701E-16));
#19242=DIRECTION('center_axis',(1.,-6.12303176911189E-17,0.));
#19243=DIRECTION('ref_axis',(-6.12303176911189E-17,-1.,0.));
#19244=DIRECTION('center_axis',(-1.,6.305873043676E-17,0.));
#19245=DIRECTION('ref_axis',(6.305873043676E-17,1.,0.));
#19246=DIRECTION('center_axis',(1.,-6.12303176911189E-17,0.));
#19247=DIRECTION('ref_axis',(6.12303176911189E-17,1.,0.));
#19248=DIRECTION('center_axis',(1.,-6.12303176911189E-17,0.));
#19249=DIRECTION('ref_axis',(5.75176428514148E-17,0.939365416027515,0.342917796521927));
#19250=DIRECTION('center_axis',(1.,-6.12303176911189E-17,0.));
#19251=DIRECTION('ref_axis',(-6.12303176911189E-17,-1.,0.));
#19252=DIRECTION('center_axis',(-1.,6.305873043676E-17,0.));
#19253=DIRECTION('ref_axis',(6.305873043676E-17,1.,0.));
#19254=DIRECTION('center_axis',(1.,-6.12303176911189E-17,0.));
#19255=DIRECTION('ref_axis',(6.12303176911189E-17,1.,0.));
#19256=DIRECTION('center_axis',(1.,-6.12303176911189E-17,0.));
#19257=DIRECTION('ref_axis',(-6.12303176911189E-17,-1.,0.));
#19258=DIRECTION('center_axis',(1.,-6.12303176911189E-17,0.));
#19259=DIRECTION('ref_axis',(0.,1.,0.));
#19260=DIRECTION('center_axis',(1.,-6.12303176911189E-17,0.));
#19261=DIRECTION('ref_axis',(0.,1.,0.));
#19262=DIRECTION('center_axis',(5.55800597652948E-17,0.907721237797144,
-0.419573777126289));
#19263=DIRECTION('ref_axis',(1.29808072260833E-31,0.419573777126289,0.907721237797144));
#19264=DIRECTION('center_axis',(5.55800597652948E-17,0.907721237797144,
-0.419573777126289));
#19265=DIRECTION('ref_axis',(1.29808072260833E-31,0.419573777126289,0.907721237797144));
#19266=DIRECTION('center_axis',(-6.12303176911189E-17,-1.,-1.13606963518701E-16));
#19267=DIRECTION('ref_axis',(6.95619046817341E-33,1.13606963518701E-16,
-1.));
#19268=DIRECTION('center_axis',(1.,-6.12303176911189E-17,0.));
#19269=DIRECTION('ref_axis',(0.,1.,0.));
#19270=DIRECTION('center_axis',(6.12303176911189E-17,1.,-1.37765518964554E-16));
#19271=DIRECTION('ref_axis',(8.43542649308151E-33,1.37765518964554E-16,
1.));
#19272=DIRECTION('center_axis',(0.707106781186548,-1.06487712312249E-15,
0.707106781186548));
#19273=DIRECTION('ref_axis',(-1.50596366978067E-15,-1.,3.33894885375682E-33));
#19274=DIRECTION('',(7.1625865367138E-18,1.,1.49880108324396E-15));
#19275=DIRECTION('center_axis',(-1.,0.,0.));
#19276=DIRECTION('ref_axis',(0.,0.,1.));
#19277=DIRECTION('center_axis',(-1.,8.82766640598215E-17,0.));
#19278=DIRECTION('ref_axis',(0.,0.93969262078591,-0.342020143325664));
#19279=DIRECTION('center_axis',(-1.3611865338937E-31,-1.5419764230905E-15,
-1.));
#19280=DIRECTION('ref_axis',(-3.05518935066593E-57,1.,-1.5419764230905E-15));
#19281=DIRECTION('center_axis',(1.,-8.55850097257312E-17,0.));
#19282=DIRECTION('ref_axis',(-8.55850097257312E-17,-1.,0.));
#19283=DIRECTION('',(1.,-8.55850097257312E-17,0.));
#19284=DIRECTION('center_axis',(0.923879532511291,2.62280693261509E-15,
-0.382683432365079));
#19285=DIRECTION('ref_axis',(0.382683432365079,-1.7921752496165E-12,0.923879532511291));
#19286=DIRECTION('center_axis',(-1.,8.82754440022857E-17,0.));
#19287=DIRECTION('ref_axis',(0.,0.995871426936473,-0.090775002128966));
#19288=DIRECTION('center_axis',(0.,0.,-1.));
#19289=DIRECTION('ref_axis',(0.,1.,0.));
#19290=DIRECTION('',(-1.,8.55850097257312E-17,0.));
#19291=DIRECTION('',(-8.82754440022857E-17,-1.,0.));
#19292=DIRECTION('center_axis',(5.49761868397523E-12,-9.20733867538014E-13,
-1.));
#19293=DIRECTION('ref_axis',(0.732793660910527,-0.680450917061141,4.65516458078155E-12));
#19294=DIRECTION('center_axis',(8.82754440022857E-17,1.,0.));
#19295=DIRECTION('ref_axis',(1.,-8.82754440022857E-17,0.));
#19296=DIRECTION('center_axis',(-0.707106781186578,-0.707106781186517,1.40152838177972E-12));
#19297=DIRECTION('ref_axis',(0.707106781186517,-0.707106781186578,-1.08700436557221E-11));
#19298=DIRECTION('center_axis',(0.,-1.,0.));
#19299=DIRECTION('ref_axis',(0.,0.,1.));
#19300=DIRECTION('center_axis',(1.,-8.55850097257312E-17,0.));
#19301=DIRECTION('ref_axis',(-8.55850097257312E-17,-1.,0.));
#19302=DIRECTION('center_axis',(1.3611865338937E-31,1.54197642309049E-15,
1.));
#19303=DIRECTION('ref_axis',(-8.16770755219275E-61,-1.,1.54197642309049E-15));
#19304=DIRECTION('center_axis',(1.,-6.12303176911189E-17,0.));
#19305=DIRECTION('ref_axis',(0.,0.,1.));
#19306=DIRECTION('',(-6.12303176911189E-17,-1.,1.71170019451462E-16));
#19307=DIRECTION('',(1.44560289664734E-16,-0.939692620785909,0.342020143325668));
#19308=DIRECTION('center_axis',(1.0480794670208E-32,1.71170019451462E-16,
1.));
#19309=DIRECTION('ref_axis',(0.,1.,-1.71170019451462E-16));
#19310=DIRECTION('center_axis',(5.72397488459722E-17,0.907721237797144,
-0.419573777126289));
#19311=DIRECTION('ref_axis',(1.37844232230888E-31,0.419573777126289,0.907721237797144));
#19312=DIRECTION('center_axis',(2.64577897101398E-17,0.419573777126289,
0.907721237797144));
#19313=DIRECTION('ref_axis',(-5.00442534740975E-33,-0.907721237797144,0.419573777126289));
#19314=DIRECTION('center_axis',(1.,-6.305873043676E-17,0.));
#19315=DIRECTION('ref_axis',(0.,1.,0.));
#19316=DIRECTION('center_axis',(1.,-6.305873043676E-17,0.));
#19317=DIRECTION('ref_axis',(0.,1.,0.));
#19318=DIRECTION('center_axis',(1.,-6.305873043676E-17,0.));
#19319=DIRECTION('ref_axis',(0.,1.,0.));
#19320=DIRECTION('center_axis',(-5.72397488459722E-17,-0.907721237797144,
0.419573777126289));
#19321=DIRECTION('ref_axis',(-1.34762744319869E-31,-0.419573777126289,-0.907721237797144));
#19322=DIRECTION('center_axis',(6.305873043676E-17,1.,1.13606963518701E-16));
#19323=DIRECTION('ref_axis',(-7.16391088826459E-33,-1.13606963518701E-16,
1.));
#19324=DIRECTION('center_axis',(1.,-6.305873043676E-17,0.));
#19325=DIRECTION('ref_axis',(0.,1.,0.));
#19326=DIRECTION('center_axis',(-6.305873043676E-17,-1.,1.37765518964554E-16));
#19327=DIRECTION('ref_axis',(-8.68731872386616E-33,-1.37765518964554E-16,
-1.));
#19328=DIRECTION('center_axis',(1.,0.,0.));
#19329=DIRECTION('ref_axis',(0.,0.112528245522859,0.993648526371145));
#19330=DIRECTION('center_axis',(-1.,0.,0.));
#19331=DIRECTION('ref_axis',(0.,0.,-1.));
#19332=DIRECTION('center_axis',(-1.,0.,0.));
#19333=DIRECTION('ref_axis',(0.,0.0968769480691947,0.995296366381792));
#19334=DIRECTION('center_axis',(0.,0.469471562785891,0.882947592858927));
#19335=DIRECTION('ref_axis',(1.,0.,0.));
#19336=DIRECTION('center_axis',(0.,0.342020143325668,0.939692620785909));
#19337=DIRECTION('ref_axis',(1.,0.,0.));
#19338=DIRECTION('',(0.,0.939692620785909,-0.342020143325668));
#19339=DIRECTION('',(0.894427190999916,0.420243315606445,-0.152956058030083));
#19340=DIRECTION('center_axis',(-1.,0.,0.));
#19341=DIRECTION('ref_axis',(0.,-1.,0.));
#19342=DIRECTION('',(0.,-0.342020143325668,-0.939692620785909));
#19343=DIRECTION('center_axis',(-0.447213595499957,0.84048663121289,-0.305912116060166));
#19344=DIRECTION('ref_axis',(-1.70074100669568E-17,-0.342020143325668,-0.939692620785909));
#19345=DIRECTION('center_axis',(0.707106781186548,-6.05177407449811E-17,
-0.707106781186548));
#19346=DIRECTION('ref_axis',(-0.707106781186548,1.46675000719695E-31,-0.707106781186548));
#19347=DIRECTION('center_axis',(1.,-6.12303176911189E-17,0.));
#19348=DIRECTION('ref_axis',(0.,0.,1.));
#19349=DIRECTION('center_axis',(1.,-6.12303176911189E-17,0.));
#19350=DIRECTION('ref_axis',(0.,0.,1.));
#19351=DIRECTION('center_axis',(1.,-6.12303176911189E-17,0.));
#19352=DIRECTION('ref_axis',(0.,0.,1.));
#19353=DIRECTION('axis',(0.,0.,1.));
#19354=DIRECTION('refdir',(1.,0.,0.));
#19355=DIRECTION('center_axis',(1.1842378929335E-15,1.1842378929335E-15,
-1.));
#19356=DIRECTION('ref_axis',(1.1842378929335E-15,1.,1.03620815631681E-15));
#19357=DIRECTION('center_axis',(-1.,1.E-15,-1.E-15));
#19358=DIRECTION('ref_axis',(-1.E-15,-1.15648231731787E-15,1.));
#19359=DIRECTION('center_axis',(1.E-15,1.,1.E-15));
#19360=DIRECTION('ref_axis',(-1.247520350843E-15,-9.99999999999999E-16,
1.));
#19361=DIRECTION('center_axis',(1.E-15,1.E-15,-1.));
#19362=DIRECTION('ref_axis',(1.15845497931055E-15,1.,1.E-15));
#19363=DIRECTION('center_axis',(1.E-15,1.,1.E-15));
#19364=DIRECTION('ref_axis',(-1.15845497931055E-15,-9.99999999999999E-16,
1.));
#19365=DIRECTION('center_axis',(1.E-15,1.E-15,-1.));
#19366=DIRECTION('ref_axis',(1.247520350843E-15,1.,1.E-15));
#19367=DIRECTION('center_axis',(-1.E-15,-1.,-1.E-15));
#19368=DIRECTION('ref_axis',(1.15845497931055E-15,9.99999999999999E-16,
-1.));
#19369=DIRECTION('center_axis',(1.E-15,1.E-15,-1.));
#19370=DIRECTION('ref_axis',(1.15845497931055E-15,1.,1.E-15));
#19371=DIRECTION('center_axis',(-1.E-15,-1.,-1.E-15));
#19372=DIRECTION('ref_axis',(1.24752035084299E-15,9.99999999999999E-16,
-1.));
#19373=DIRECTION('center_axis',(-1.E-15,-1.E-15,1.));
#19374=DIRECTION('ref_axis',(-1.15845497931055E-15,-1.,-1.E-15));
#19375=DIRECTION('center_axis',(-1.E-15,-1.,-1.E-15));
#19376=DIRECTION('ref_axis',(1.15845497931055E-15,9.99999999999999E-16,
-1.));
#19377=DIRECTION('center_axis',(-1.E-15,-1.E-15,1.));
#19378=DIRECTION('ref_axis',(-1.247520350843E-15,-1.,-1.E-15));
#19379=DIRECTION('center_axis',(1.E-15,1.,1.E-15));
#19380=DIRECTION('ref_axis',(-1.15845497931055E-15,-9.99999999999999E-16,
1.));
#19381=DIRECTION('center_axis',(-1.E-15,-1.E-15,1.));
#19382=DIRECTION('ref_axis',(-1.15845497931055E-15,-1.,-1.E-15));
#19383=DIRECTION('center_axis',(1.,-1.E-15,1.E-15));
#19384=DIRECTION('ref_axis',(1.E-15,-1.E-30,-1.));
#19385=DIRECTION('center_axis',(-1.,1.E-15,-1.E-15));
#19386=DIRECTION('ref_axis',(-1.E-15,1.E-30,1.));
#19387=DIRECTION('',(-0.707106781186548,7.93702386810097E-16,-0.707106781186547));
#19388=DIRECTION('center_axis',(-1.,1.E-15,-1.E-15));
#19389=DIRECTION('ref_axis',(-1.E-15,1.E-30,1.));
#19390=DIRECTION('center_axis',(-1.,1.E-15,-1.E-15));
#19391=DIRECTION('ref_axis',(-1.E-15,1.E-30,1.));
#19392=DIRECTION('center_axis',(1.,-1.E-15,1.E-15));
#19393=DIRECTION('ref_axis',(-1.E-15,-1.15648231731787E-15,1.));
#19394=DIRECTION('',(-1.,1.E-15,-1.E-15));
#19395=DIRECTION('center_axis',(-1.,1.E-15,-1.E-15));
#19396=DIRECTION('ref_axis',(-1.E-15,-1.15648231731787E-15,1.));
#19397=DIRECTION('center_axis',(1.,-1.E-15,1.E-15));
#19398=DIRECTION('ref_axis',(-1.E-15,1.E-30,1.));
#19399=DIRECTION('center_axis',(-1.,1.E-15,-1.E-15));
#19400=DIRECTION('ref_axis',(-1.E-15,1.E-30,1.));
#19401=DIRECTION('',(-1.,1.E-15,-1.E-15));
#19402=DIRECTION('center_axis',(-1.,1.E-15,-1.E-15));
#19403=DIRECTION('ref_axis',(1.E-15,1.,1.E-15));
#19404=DIRECTION('center_axis',(-1.E-15,-1.,-1.E-15));
#19405=DIRECTION('ref_axis',(-1.E-15,-1.E-15,1.));
#19406=DIRECTION('',(1.,-1.E-15,1.E-15));
#19407=DIRECTION('',(1.E-15,1.E-15,-1.));
#19408=DIRECTION('',(1.,-1.E-15,1.E-15));
#19409=DIRECTION('center_axis',(1.E-15,1.E-15,-1.));
#19410=DIRECTION('ref_axis',(1.,-1.E-15,1.E-15));
#19411=DIRECTION('',(1.E-15,1.,1.E-15));
#19412=DIRECTION('',(1.,-1.E-15,1.E-15));
#19413=DIRECTION('center_axis',(-1.E-15,-1.,-1.E-15));
#19414=DIRECTION('ref_axis',(-1.E-15,-1.E-15,1.));
#19415=DIRECTION('',(1.E-15,1.E-15,-1.));
#19416=DIRECTION('',(1.,-1.E-15,1.E-15));
#19417=DIRECTION('center_axis',(-1.E-15,-9.99999999999999E-16,1.));
#19418=DIRECTION('ref_axis',(1.E-15,1.,1.E-15));
#19419=DIRECTION('',(-1.E-15,-1.,-1.E-15));
#19420=DIRECTION('',(1.,-1.E-15,1.E-15));
#19421=DIRECTION('center_axis',(-1.E-15,-1.,-1.E-15));
#19422=DIRECTION('ref_axis',(-1.E-15,-1.E-15,1.));
#19423=DIRECTION('',(1.E-15,1.E-15,-1.));
#19424=DIRECTION('',(1.,-1.E-15,1.E-15));
#19425=DIRECTION('center_axis',(-1.E-15,-9.99999999999999E-16,1.));
#19426=DIRECTION('ref_axis',(1.E-15,1.,1.E-15));
#19427=DIRECTION('',(-1.E-15,-1.,-1.E-15));
#19428=DIRECTION('',(1.,-1.E-15,1.E-15));
#19429=DIRECTION('center_axis',(1.E-15,1.E-15,-1.));
#19430=DIRECTION('ref_axis',(1.,-1.E-15,1.E-15));
#19431=DIRECTION('',(1.,-1.E-15,1.E-15));
#19432=DIRECTION('',(1.E-15,1.,1.E-15));
#19433=DIRECTION('center_axis',(9.99999999999999E-16,1.,1.E-15));
#19434=DIRECTION('ref_axis',(-1.,1.E-15,-1.E-15));
#19435=DIRECTION('',(1.,-1.E-15,1.E-15));
#19436=DIRECTION('',(-1.E-15,-1.E-15,1.));
#19437=DIRECTION('center_axis',(9.99999999999999E-16,1.,1.E-15));
#19438=DIRECTION('ref_axis',(-1.,1.E-15,-1.E-15));
#19439=DIRECTION('',(-1.E-15,-1.E-15,1.));
#19440=DIRECTION('',(1.,-1.E-15,1.E-15));
#19441=DIRECTION('center_axis',(-1.E-15,-9.99999999999999E-16,1.));
#19442=DIRECTION('ref_axis',(1.E-15,1.,1.E-15));
#19443=DIRECTION('',(-1.E-15,-1.,-1.E-15));
#19444=DIRECTION('',(1.,-1.E-15,1.E-15));
#19445=DIRECTION('center_axis',(1.E-15,1.E-15,-1.));
#19446=DIRECTION('ref_axis',(1.,-1.E-15,1.E-15));
#19447=DIRECTION('',(1.,-1.E-15,1.E-15));
#19448=DIRECTION('',(1.E-15,1.,1.E-15));
#19449=DIRECTION('center_axis',(9.99999999999999E-16,1.,1.E-15));
#19450=DIRECTION('ref_axis',(-1.,1.E-15,-1.E-15));
#19451=DIRECTION('',(-1.E-15,-1.E-15,1.));
#19452=DIRECTION('center_axis',(-1.,1.E-15,-1.E-15));
#19453=DIRECTION('ref_axis',(1.E-15,1.,1.E-15));
#19454=DIRECTION('center_axis',(-1.,1.E-15,-1.E-15));
#19455=DIRECTION('ref_axis',(1.E-15,1.,1.E-15));
#19456=DIRECTION('axis',(0.,0.,1.));
#19457=DIRECTION('refdir',(1.,0.,0.));
#19458=DIRECTION('center_axis',(-0.109509747813017,0.,0.993985721795806));
#19459=DIRECTION('ref_axis',(-0.993985721795806,0.,-0.109509747813017));
#19460=DIRECTION('',(0.109509747813017,0.,-0.993985721795806));
#19461=DIRECTION('center_axis',(0.109509747813016,0.,-0.993985721795806));
#19462=DIRECTION('ref_axis',(-0.993985721795806,0.,-0.109509747813016));
#19463=DIRECTION('',(-0.109509747813016,0.,0.993985721795806));
#19464=DIRECTION('center_axis',(-0.109509747813016,0.,0.993985721795806));
#19465=DIRECTION('ref_axis',(-0.993985721795806,0.,-0.109509747813016));
#19466=DIRECTION('',(0.109509747813017,0.,-0.993985721795806));
#19467=DIRECTION('center_axis',(0.109509747813017,0.,-0.993985721795806));
#19468=DIRECTION('ref_axis',(0.993985721795806,0.,0.109509747813017));
#19469=DIRECTION('center_axis',(-0.109509747813016,0.,0.993985721795806));
#19470=DIRECTION('ref_axis',(-0.993985721795806,0.,-0.109509747813016));
#19471=DIRECTION('',(-0.109509747813016,-5.79756587691265E-17,0.993985721795806));
#19472=DIRECTION('center_axis',(0.109509747813016,0.,-0.993985721795806));
#19473=DIRECTION('ref_axis',(-6.66524446162044E-16,1.,-7.34325679030328E-17));
#19474=DIRECTION('center_axis',(-0.109509747813017,0.,0.993985721795806));
#19475=DIRECTION('ref_axis',(-0.993985721795806,0.,-0.109509747813017));
#19476=DIRECTION('',(0.109509747813017,0.,-0.993985721795806));
#19477=DIRECTION('center_axis',(0.109509747813016,0.,-0.993985721795806));
#19478=DIRECTION('ref_axis',(-0.993985721795806,0.,-0.109509747813016));
#19479=DIRECTION('',(-0.109509747813016,5.79756587691264E-17,0.993985721795806));
#19480=DIRECTION('center_axis',(0.109509747813016,0.,-0.993985721795806));
#19481=DIRECTION('ref_axis',(-0.993985721795806,0.,-0.109509747813016));
#19482=DIRECTION('center_axis',(0.109509747813016,0.,-0.993985721795806));
#19483=DIRECTION('ref_axis',(-6.66524446162044E-16,1.,-7.34325679030328E-17));
#19484=DIRECTION('',(0.109509747813016,3.61400724161835E-16,-0.993985721795806));
#19485=DIRECTION('center_axis',(0.109509747813016,0.,-0.993985721795806));
#19486=DIRECTION('ref_axis',(-6.66524446162044E-16,1.,-7.34325679030328E-17));
#19487=DIRECTION('center_axis',(-0.109509747813017,0.,0.993985721795806));
#19488=DIRECTION('ref_axis',(-0.993985721795806,0.,-0.109509747813017));
#19489=DIRECTION('',(0.109509747813017,0.,-0.993985721795806));
#19490=DIRECTION('center_axis',(0.109509747813016,0.,-0.993985721795806));
#19491=DIRECTION('ref_axis',(-0.993985721795806,0.,-0.109509747813016));
#19492=DIRECTION('',(-0.109509747813016,0.,0.993985721795806));
#19493=DIRECTION('center_axis',(-0.109509747813016,0.,0.993985721795806));
#19494=DIRECTION('ref_axis',(0.936831271488445,-0.334206918693375,0.103212907423556));
#19495=DIRECTION('',(0.109509747813017,0.,-0.993985721795806));
#19496=DIRECTION('center_axis',(-0.109509747813016,0.,0.993985721795806));
#19497=DIRECTION('ref_axis',(-0.993985721795806,0.,-0.109509747813016));
#19498=DIRECTION('',(0.109509747813016,0.,-0.993985721795806));
#19499=DIRECTION('center_axis',(0.109509747813016,0.,-0.993985721795806));
#19500=DIRECTION('ref_axis',(-0.993985721795806,0.,-0.109509747813016));
#19501=DIRECTION('center_axis',(0.109509747813016,0.,-0.993985721795806));
#19502=DIRECTION('ref_axis',(-6.66524446162044E-16,1.,-7.34325679030328E-17));
#19503=DIRECTION('',(-0.109509747813016,-5.79756587691265E-17,0.993985721795806));
#19504=DIRECTION('center_axis',(-0.109509747813016,0.,0.993985721795806));
#19505=DIRECTION('ref_axis',(-0.993985721795806,0.,-0.109509747813016));
#19506=DIRECTION('center_axis',(-0.109509747813016,0.,0.993985721795806));
#19507=DIRECTION('ref_axis',(0.936831271488445,-0.334206918693375,0.103212907423556));
#19508=DIRECTION('',(-0.109509747813016,-5.79756587691265E-17,0.993985721795806));
#19509=DIRECTION('center_axis',(0.109509747813016,0.,-0.993985721795806));
#19510=DIRECTION('ref_axis',(-7.61742224185193E-16,1.,-8.39229347463232E-17));
#19511=DIRECTION('center_axis',(-0.109509747813017,0.,0.993985721795806));
#19512=DIRECTION('ref_axis',(-0.993985721795806,0.,-0.109509747813017));
#19513=DIRECTION('center_axis',(-0.109509747813016,0.,0.993985721795806));
#19514=DIRECTION('ref_axis',(-0.993985721795806,0.,-0.109509747813016));
#19515=DIRECTION('',(0.109509747813017,0.,-0.993985721795806));
#19516=DIRECTION('center_axis',(-0.109509747813016,0.,0.993985721795806));
#19517=DIRECTION('ref_axis',(0.936831271488445,-0.334206918693375,0.103212907423556));
#19518=DIRECTION('',(0.109509747813016,0.,-0.993985721795806));
#19519=DIRECTION('center_axis',(0.109509747813016,0.,-0.993985721795806));
#19520=DIRECTION('ref_axis',(-0.993985721795806,0.,-0.109509747813016));
#19521=DIRECTION('',(0.109509747813017,0.,-0.993985721795806));
#19522=DIRECTION('center_axis',(0.109509747813016,0.,-0.993985721795806));
#19523=DIRECTION('ref_axis',(-7.61742224185193E-16,1.,-8.39229347463232E-17));
#19524=DIRECTION('',(-0.109509747813016,-5.79756587691265E-17,0.993985721795806));
#19525=DIRECTION('center_axis',(-0.109509747813016,0.,0.993985721795806));
#19526=DIRECTION('ref_axis',(0.936831271488445,-0.334206918693375,0.103212907423556));
#19527=DIRECTION('center_axis',(0.109509747813016,0.,-0.993985721795806));
#19528=DIRECTION('ref_axis',(0.993985721795806,0.,0.109509747813016));
#19529=DIRECTION('',(-0.109509747813016,0.,0.993985721795806));
#19530=DIRECTION('center_axis',(-0.109509747813016,0.,0.993985721795806));
#19531=DIRECTION('ref_axis',(-0.993985721795806,0.,-0.109509747813016));
#19532=DIRECTION('',(0.109509747813015,7.50701870275913E-16,-0.993985721795806));
#19533=DIRECTION('center_axis',(0.109509747813016,0.,-0.993985721795806));
#19534=DIRECTION('ref_axis',(0.936831271488447,0.33420691869337,0.103212907423556));
#19535=DIRECTION('',(0.109509747813016,3.00462919747432E-16,-0.993985721795806));
#19536=DIRECTION('center_axis',(0.109509747813016,0.,-0.993985721795806));
#19537=DIRECTION('ref_axis',(0.936831271488447,0.33420691869337,0.103212907423556));
#19538=DIRECTION('',(-0.109509747813016,0.,0.993985721795806));
#19539=DIRECTION('center_axis',(-0.109509747813016,0.,0.993985721795806));
#19540=DIRECTION('ref_axis',(-0.993985721795806,0.,-0.109509747813016));
#19541=DIRECTION('center_axis',(0.109509747813016,0.,-0.993985721795806));
#19542=DIRECTION('ref_axis',(0.993985721795806,0.,0.109509747813016));
#19543=DIRECTION('',(-0.109509747813016,0.,0.993985721795806));
#19544=DIRECTION('center_axis',(-0.109509747813016,0.,0.993985721795806));
#19545=DIRECTION('ref_axis',(0.936831271488445,-0.334206918693375,0.103212907423556));
#19546=DIRECTION('',(0.109509747813015,7.50701870275913E-16,-0.993985721795806));
#19547=DIRECTION('center_axis',(0.109509747813016,0.,-0.993985721795806));
#19548=DIRECTION('ref_axis',(0.936831271488447,0.33420691869337,0.103212907423556));
#19549=DIRECTION('',(0.109509747813016,3.00462919747432E-16,-0.993985721795806));
#19550=DIRECTION('center_axis',(0.109509747813016,0.,-0.993985721795806));
#19551=DIRECTION('ref_axis',(0.936831271488447,0.33420691869337,0.103212907423556));
#19552=DIRECTION('',(-0.109509747813016,0.,0.993985721795806));
#19553=DIRECTION('center_axis',(-0.109509747813016,0.,0.993985721795806));
#19554=DIRECTION('ref_axis',(0.936831271488445,-0.334206918693375,0.103212907423556));
#19555=DIRECTION('center_axis',(0.109509747813016,0.,-0.993985721795806));
#19556=DIRECTION('ref_axis',(0.993985721795806,0.,0.109509747813016));
#19557=DIRECTION('center_axis',(0.109509747813016,0.,-0.993985721795806));
#19558=DIRECTION('ref_axis',(0.993985721795806,0.,0.109509747813016));
#19559=DIRECTION('',(0.109509747813016,0.,-0.993985721795806));
#19560=DIRECTION('center_axis',(0.109509747813016,0.,-0.993985721795806));
#19561=DIRECTION('ref_axis',(0.993985721795806,0.,0.109509747813016));
#19562=DIRECTION('center_axis',(0.109509747813016,0.,-0.993985721795806));
#19563=DIRECTION('ref_axis',(0.993985721795806,0.,0.109509747813016));
#19564=DIRECTION('center_axis',(-0.109509747813016,0.,0.993985721795806));
#19565=DIRECTION('ref_axis',(0.993985721795806,0.,0.109509747813016));
#19566=DIRECTION('',(-0.109509747813016,0.,0.993985721795806));
#19567=DIRECTION('center_axis',(0.109509747813016,0.,-0.993985721795806));
#19568=DIRECTION('ref_axis',(-0.993985721795806,0.,-0.109509747813016));
#19569=DIRECTION('center_axis',(-0.109509747813016,0.,0.993985721795806));
#19570=DIRECTION('ref_axis',(-0.993985721795806,0.,-0.109509747813016));
#19571=DIRECTION('center_axis',(-0.109509747813016,0.,0.993985721795806));
#19572=DIRECTION('ref_axis',(0.993985721795806,0.,0.109509747813016));
#19573=DIRECTION('',(-0.109509747813016,0.,0.993985721795806));
#19574=DIRECTION('center_axis',(-0.109509747813016,0.,0.993985721795806));
#19575=DIRECTION('ref_axis',(0.993985721795806,0.,0.109509747813016));
#19576=DIRECTION('center_axis',(-0.109509747813016,0.,0.993985721795806));
#19577=DIRECTION('ref_axis',(-0.993985721795806,0.,-0.109509747813016));
#19578=DIRECTION('center_axis',(-0.109509747813016,0.,0.993985721795806));
#19579=DIRECTION('ref_axis',(-0.993985721795806,0.,-0.109509747813016));
#19580=DIRECTION('',(-0.109509747813016,5.79756587691264E-17,0.993985721795806));
#19581=DIRECTION('center_axis',(-0.109509747813016,0.,0.993985721795806));
#19582=DIRECTION('ref_axis',(-0.993985721795806,0.,-0.109509747813016));
#19583=DIRECTION('',(-0.109509747813016,-1.50231459873716E-16,0.993985721795806));
#19584=DIRECTION('center_axis',(-0.109509747813016,0.,0.993985721795806));
#19585=DIRECTION('ref_axis',(-0.993985721795806,0.,-0.109509747813016));
#19586=DIRECTION('center_axis',(-0.109509747813016,0.,0.993985721795806));
#19587=DIRECTION('ref_axis',(-0.936831271488455,0.334206918693347,-0.103212907423557));
#19588=DIRECTION('',(-0.109509747813016,1.50231459873716E-16,0.993985721795806));
#19589=DIRECTION('center_axis',(0.109509747813016,0.,-0.993985721795806));
#19590=DIRECTION('ref_axis',(-0.496992860897901,-0.86602540378444,-0.0547548739065078));
#19591=DIRECTION('center_axis',(-0.109509747813016,0.,0.993985721795806));
#19592=DIRECTION('ref_axis',(-0.993985721795806,0.,-0.109509747813016));
#19593=DIRECTION('center_axis',(0.109509747813016,0.,-0.993985721795806));
#19594=DIRECTION('ref_axis',(-0.496992860897901,-0.86602540378444,-0.0547548739065078));
#19595=DIRECTION('',(-0.109509747813016,1.50231459873716E-16,0.993985721795806));
#19596=DIRECTION('center_axis',(-0.109509747813016,0.,0.993985721795806));
#19597=DIRECTION('ref_axis',(-0.936831271488455,0.334206918693348,-0.103212907423557));
#19598=DIRECTION('center_axis',(0.109509747813016,0.,-0.993985721795806));
#19599=DIRECTION('ref_axis',(0.993985721795806,0.,0.109509747813016));
#19600=DIRECTION('center_axis',(-0.109509747813016,0.,0.993985721795806));
#19601=DIRECTION('ref_axis',(0.936831271488445,-0.334206918693375,0.103212907423556));
#19602=DIRECTION('',(0.109509747813016,1.15951317538253E-16,-0.993985721795806));
#19603=DIRECTION('center_axis',(0.109509747813016,0.,-0.993985721795806));
#19604=DIRECTION('ref_axis',(-6.23243637969703E-16,1.,-6.86642193379008E-17));
#19605=DIRECTION('',(-0.109509747813016,0.,0.993985721795806));
#19606=DIRECTION('center_axis',(0.109509747813016,0.,-0.993985721795806));
#19607=DIRECTION('ref_axis',(-6.23243637969703E-16,1.,-6.86642193379008E-17));
#19608=DIRECTION('',(0.109509747813016,1.15951317538253E-16,-0.993985721795806));
#19609=DIRECTION('center_axis',(-0.109509747813016,0.,0.993985721795806));
#19610=DIRECTION('ref_axis',(0.936831271488445,-0.334206918693375,0.103212907423556));
#19611=DIRECTION('center_axis',(-0.109509747813016,0.,0.993985721795806));
#19612=DIRECTION('ref_axis',(-0.993985721795806,0.,-0.109509747813016));
#19613=DIRECTION('center_axis',(-0.109509747813016,0.,0.993985721795806));
#19614=DIRECTION('ref_axis',(-0.936831271488455,0.334206918693348,-0.103212907423557));
#19615=DIRECTION('',(-0.109509747813016,1.50231459873716E-16,0.993985721795806));
#19616=DIRECTION('center_axis',(0.109509747813016,0.,-0.993985721795806));
#19617=DIRECTION('ref_axis',(-0.496992860897901,-0.86602540378444,-0.0547548739065078));
#19618=DIRECTION('center_axis',(-0.109509747813016,0.,0.993985721795806));
#19619=DIRECTION('ref_axis',(-0.993985721795806,0.,-0.109509747813016));
#19620=DIRECTION('center_axis',(0.109509747813016,0.,-0.993985721795806));
#19621=DIRECTION('ref_axis',(-0.496992860897901,-0.86602540378444,-0.0547548739065078));
#19622=DIRECTION('',(-0.109509747813016,1.50231459873716E-16,0.993985721795806));
#19623=DIRECTION('center_axis',(-0.109509747813016,0.,0.993985721795806));
#19624=DIRECTION('ref_axis',(-0.936831271488455,0.334206918693348,-0.103212907423557));
#19625=DIRECTION('center_axis',(0.109509747813016,0.,-0.993985721795806));
#19626=DIRECTION('ref_axis',(0.993985721795806,0.,0.109509747813016));
#19627=DIRECTION('center_axis',(-0.109509747813016,0.,0.993985721795806));
#19628=DIRECTION('ref_axis',(-0.993985721795806,0.,-0.109509747813016));
#19629=DIRECTION('',(0.109509747813016,1.15951317538253E-16,-0.993985721795806));
#19630=DIRECTION('center_axis',(0.109509747813016,0.,-0.993985721795806));
#19631=DIRECTION('ref_axis',(-5.4533818322349E-16,1.,-6.00811919206632E-17));
#19632=DIRECTION('',(-0.109509747813016,0.,0.993985721795806));
#19633=DIRECTION('center_axis',(0.109509747813016,0.,-0.993985721795806));
#19634=DIRECTION('ref_axis',(-5.4533818322349E-16,1.,-6.00811919206632E-17));
#19635=DIRECTION('',(0.109509747813016,1.15951317538253E-16,-0.993985721795806));
#19636=DIRECTION('center_axis',(-0.109509747813016,0.,0.993985721795806));
#19637=DIRECTION('ref_axis',(-0.993985721795806,0.,-0.109509747813016));
#19638=DIRECTION('center_axis',(-0.109509747813016,0.,0.993985721795806));
#19639=DIRECTION('ref_axis',(-0.993985721795806,0.,-0.109509747813016));
#19640=DIRECTION('center_axis',(-0.109509747813016,0.,0.993985721795806));
#19641=DIRECTION('ref_axis',(-0.993985721795806,0.,-0.109509747813016));
#19642=DIRECTION('center_axis',(-0.109509747813016,0.,0.993985721795806));
#19643=DIRECTION('ref_axis',(-0.993985721795806,0.,-0.109509747813016));
#19644=DIRECTION('',(-0.109509747813016,-1.50231459873716E-16,0.993985721795806));
#19645=DIRECTION('center_axis',(-0.109509747813017,0.,0.993985721795806));
#19646=DIRECTION('ref_axis',(-0.993985721795806,0.,-0.109509747813017));
#19647=DIRECTION('center_axis',(0.109509747813017,0.,-0.993985721795806));
#19648=DIRECTION('ref_axis',(-0.993985721795806,0.,-0.109509747813017));
#19649=DIRECTION('',(-0.109509747813017,0.,0.993985721795806));
#19650=DIRECTION('center_axis',(0.109509747813017,0.,-0.993985721795806));
#19651=DIRECTION('ref_axis',(-0.993985721795806,0.,-0.109509747813017));
#19652=DIRECTION('center_axis',(-0.109509747813017,0.,0.993985721795806));
#19653=DIRECTION('ref_axis',(-0.993985721795806,0.,-0.109509747813017));
#19654=DIRECTION('center_axis',(0.109509747813016,0.,-0.993985721795806));
#19655=DIRECTION('ref_axis',(-0.993985721795806,0.,-0.109509747813016));
#19656=DIRECTION('center_axis',(0.109509747813016,0.,-0.993985721795806));
#19657=DIRECTION('ref_axis',(-0.993985721795806,0.,-0.109509747813016));
#19658=DIRECTION('center_axis',(0.109509747813016,0.,-0.993985721795806));
#19659=DIRECTION('ref_axis',(-7.61742224185193E-16,1.,-8.39229347463232E-17));
#19660=DIRECTION('',(0.109509747813016,3.61400724161835E-16,-0.993985721795806));
#19661=DIRECTION('center_axis',(0.109509747813016,0.,-0.993985721795806));
#19662=DIRECTION('ref_axis',(-7.61742224185193E-16,1.,-8.39229347463232E-17));
#19663=DIRECTION('center_axis',(0.109509747813017,0.,-0.993985721795806));
#19664=DIRECTION('ref_axis',(0.,-1.,0.));
#19665=DIRECTION('center_axis',(0.645221227515378,0.760681545236145,0.0710855421355126));
#19666=DIRECTION('ref_axis',(0.109509747813016,-3.16883939248426E-18,-0.993985721795806));
#19667=DIRECTION('',(-0.756106594798299,0.64912524734226,-0.0833020441848256));
#19668=DIRECTION('',(0.756106594798299,-0.64912524734226,0.0833020441848256));
#19669=DIRECTION('center_axis',(-0.645221227515378,-0.760681545236145,-0.0710855421355126));
#19670=DIRECTION('ref_axis',(-0.756106594798299,0.64912524734226,-0.0833020441848256));
#19671=DIRECTION('',(-0.756106594798299,0.64912524734226,-0.0833020441848256));
#19672=DIRECTION('',(0.756106594798299,-0.64912524734226,0.0833020441848256));
#19673=DIRECTION('center_axis',(-0.496992860897903,0.866025403784439,-0.054754873906508));
#19674=DIRECTION('ref_axis',(0.86081688607418,0.5,0.0948382235681014));
#19675=DIRECTION('center_axis',(-0.496992860897903,0.866025403784439,-0.0547548739065078));
#19676=DIRECTION('ref_axis',(-0.86081688607418,-0.5,-0.0948382235681014));
#19677=DIRECTION('',(-0.496992860897903,0.866025403784439,-0.054754873906508));
#19678=DIRECTION('center_axis',(0.496992860897903,-0.866025403784439,0.0547548739065076));
#19679=DIRECTION('ref_axis',(0.86081688607418,0.5,0.0948382235681014));
#19680=DIRECTION('',(0.496992860897903,-0.866025403784439,0.054754873906508));
#19681=DIRECTION('center_axis',(0.109509747813016,0.,-0.993985721795806));
#19682=DIRECTION('ref_axis',(0.,-1.,0.));
#19683=DIRECTION('',(0.756106594798299,-0.64912524734226,0.0833020441848256));
#19684=DIRECTION('',(-0.86081688607418,-0.5,-0.0948382235680992));
#19685=DIRECTION('',(-0.86081688607418,-0.5,-0.0948382235680992));
#19686=DIRECTION('center_axis',(-0.496992860897903,0.866025403784439,-0.0547548739065078));
#19687=DIRECTION('ref_axis',(-0.109509747813016,-8.62567737696967E-18,0.993985721795806));
#19688=DIRECTION('',(-0.109509747813016,-1.50231459873716E-16,0.993985721795806));
#19689=DIRECTION('center_axis',(-0.496992860897903,0.866025403784439,-0.0547548739065078));
#19690=DIRECTION('ref_axis',(-0.86081688607418,-0.5,-0.0948382235681014));
#19691=DIRECTION('',(-0.86081688607418,-0.5,-0.0948382235680992));
#19692=DIRECTION('center_axis',(-0.756106594798299,0.64912524734226,-0.0833020441848257));
#19693=DIRECTION('ref_axis',(0.645221227515377,0.760681545236146,0.0710855421355155));
#19694=DIRECTION('center_axis',(0.109509747813016,0.,-0.993985721795806));
#19695=DIRECTION('ref_axis',(0.,-1.,0.));
#19696=DIRECTION('',(0.756106594798299,-0.64912524734226,0.0833020441848257));
#19697=DIRECTION('',(-0.86081688607418,0.5,-0.0948382235680992));
#19698=DIRECTION('',(-0.496992860897903,-0.866025403784439,-0.054754873906508));
#19699=DIRECTION('',(-0.86081688607418,0.5,-0.0948382235680992));
#19700=DIRECTION('center_axis',(0.496992860897903,-0.866025403784439,0.054754873906508));
#19701=DIRECTION('ref_axis',(-0.86081688607418,-0.5,-0.0948382235681014));
#19702=DIRECTION('',(-0.496992860897903,0.866025403784439,-0.054754873906508));
#19703=DIRECTION('center_axis',(0.496992860897903,-0.866025403784439,0.0547548739065076));
#19704=DIRECTION('ref_axis',(0.86081688607418,0.5,0.0948382235681014));
#19705=DIRECTION('',(0.496992860897903,-0.866025403784439,0.054754873906508));
#19706=DIRECTION('center_axis',(-0.756106594798299,0.64912524734226,-0.0833020441848257));
#19707=DIRECTION('ref_axis',(0.645221227515377,0.760681545236146,0.0710855421355154));
#19708=DIRECTION('',(-0.756106594798299,0.64912524734226,-0.0833020441848257));
#19709=DIRECTION('center_axis',(0.756106594798299,-0.64912524734226,0.0833020441848257));
#19710=DIRECTION('ref_axis',(-0.645221227515377,-0.760681545236146,-0.0710855421355154));
#19711=DIRECTION('',(-0.756106594798299,0.64912524734226,-0.0833020441848256));
#19712=DIRECTION('center_axis',(-0.109509747813016,0.,0.993985721795806));
#19713=DIRECTION('ref_axis',(0.993985721795806,0.,0.109509747813016));
#19714=DIRECTION('',(-0.86081688607418,0.5,-0.0948382235680992));
#19715=DIRECTION('',(0.496992860897903,0.866025403784439,0.054754873906508));
#19716=DIRECTION('',(-0.86081688607418,0.5,-0.0948382235680992));
#19717=DIRECTION('center_axis',(0.496992860897903,-0.866025403784439,0.0547548739065076));
#19718=DIRECTION('ref_axis',(0.109509747813016,4.04398041928102E-16,-0.993985721795806));
#19719=DIRECTION('',(-0.86081688607418,-0.5,-0.0948382235680992));
#19720=DIRECTION('',(0.109509747813016,3.00462919747432E-16,-0.993985721795806));
#19721=DIRECTION('center_axis',(0.109509747813016,0.,-0.993985721795806));
#19722=DIRECTION('ref_axis',(0.,-1.,0.));
#19723=DIRECTION('center_axis',(-0.756106594798299,0.64912524734226,-0.0833020441848257));
#19724=DIRECTION('ref_axis',(0.645221227515377,0.760681545236146,0.0710855421355155));
#19725=DIRECTION('center_axis',(-0.86081688607418,-0.5,-0.0948382235680992));
#19726=DIRECTION('ref_axis',(-0.496992860897903,0.866025403784439,-0.054754873906508));
#19727=DIRECTION('center_axis',(-0.993985721795806,6.12303176911189E-17,
-0.109509747813016));
#19728=DIRECTION('ref_axis',(-0.109509747813016,-4.27307853354592E-34,0.993985721795806));
#19729=DIRECTION('',(-3.7115920228551E-17,-1.,-2.22241612446982E-16));
#19730=DIRECTION('',(1.08354344120878E-16,1.,-4.24367274947369E-16));
#19731=DIRECTION('center_axis',(-0.496992860897903,-0.866025403784439,-0.054754873906508));
#19732=DIRECTION('ref_axis',(-0.86081688607418,0.5,-0.0948382235681014));
#19733=DIRECTION('center_axis',(-0.496992860897903,-0.866025403784439,-0.0547548739065078));
#19734=DIRECTION('ref_axis',(0.86081688607418,-0.5,0.0948382235681014));
#19735=DIRECTION('',(-0.496992860897903,-0.866025403784439,-0.054754873906508));
#19736=DIRECTION('center_axis',(0.496992860897903,0.866025403784439,0.0547548739065076));
#19737=DIRECTION('ref_axis',(-0.86081688607418,0.5,-0.0948382235681014));
#19738=DIRECTION('center_axis',(0.86081688607418,-0.5,0.0948382235680992));
#19739=DIRECTION('ref_axis',(0.109509747813016,-1.37062880361661E-18,-0.993985721795806));
#19740=DIRECTION('',(-0.109509747813016,1.50231459873716E-16,0.993985721795806));
#19741=DIRECTION('',(0.496992860897903,0.866025403784439,0.054754873906508));
#19742=DIRECTION('',(0.109509747813016,-3.00462919747432E-16,-0.993985721795806));
#19743=DIRECTION('center_axis',(0.496992860897903,0.866025403784439,0.0547548739065076));
#19744=DIRECTION('ref_axis',(0.109509747813015,-2.68836199388207E-18,-0.993985721795806));
#19745=DIRECTION('center_axis',(0.496992860897903,0.866025403784439,0.0547548739065076));
#19746=DIRECTION('ref_axis',(-0.86081688607418,0.5,-0.0948382235681014));
#19747=DIRECTION('',(0.86081688607418,-0.5,0.0948382235680992));
#19748=DIRECTION('',(-0.109509747813016,0.,0.993985721795806));
#19749=DIRECTION('',(0.86081688607418,-0.5,0.0948382235680992));
#19750=DIRECTION('center_axis',(-0.86081688607418,0.5,-0.0948382235680992));
#19751=DIRECTION('ref_axis',(-0.109509747813016,1.37062880361661E-18,0.993985721795806));
#19752=DIRECTION('',(0.496992860897903,0.866025403784439,0.0547548739065076));
#19753=DIRECTION('',(0.109509747813016,3.12982208070242E-16,-0.993985721795806));
#19754=DIRECTION('',(-0.496992860897903,-0.866025403784439,-0.0547548739065082));
#19755=DIRECTION('center_axis',(0.109509747813016,0.,-0.993985721795806));
#19756=DIRECTION('ref_axis',(0.,-1.,0.));
#19757=DIRECTION('',(0.86081688607418,-0.5,0.0948382235680992));
#19758=DIRECTION('center_axis',(-0.496992860897903,-0.866025403784439,-0.0547548739065078));
#19759=DIRECTION('ref_axis',(-0.86081688607418,0.5,-0.0948382235680992));
#19760=DIRECTION('center_axis',(-0.496992860897903,-0.866025403784439,-0.0547548739065078));
#19761=DIRECTION('ref_axis',(0.86081688607418,-0.5,0.0948382235681014));
#19762=DIRECTION('',(0.86081688607418,-0.5,0.0948382235680992));
#19763=DIRECTION('center_axis',(-0.109509747813016,0.,0.993985721795806));
#19764=DIRECTION('ref_axis',(0.993985721795806,0.,0.109509747813016));
#19765=DIRECTION('center_axis',(0.496992860897903,0.866025403784439,0.054754873906508));
#19766=DIRECTION('ref_axis',(0.86081688607418,-0.5,0.0948382235681014));
#19767=DIRECTION('center_axis',(-0.993985721795806,6.12303176911189E-17,
-0.109509747813016));
#19768=DIRECTION('ref_axis',(-0.109509747813016,-4.27307853354592E-34,0.993985721795806));
#19769=DIRECTION('',(-3.7115920228551E-17,-1.,-2.22241612446982E-16));
#19770=DIRECTION('',(1.08354344120878E-16,1.,-4.24367274947369E-16));
#19771=DIRECTION('center_axis',(-0.496992860897903,-0.866025403784439,-0.054754873906508));
#19772=DIRECTION('ref_axis',(-0.86081688607418,0.5,-0.0948382235680945));
#19773=DIRECTION('center_axis',(-0.496992860897903,-0.866025403784439,-0.0547548739065078));
#19774=DIRECTION('ref_axis',(0.86081688607418,-0.5,0.0948382235680946));
#19775=DIRECTION('',(-0.496992860897903,-0.866025403784439,-0.054754873906508));
#19776=DIRECTION('center_axis',(0.496992860897903,0.866025403784439,0.0547548739065076));
#19777=DIRECTION('ref_axis',(-0.86081688607418,0.5,-0.0948382235680945));
#19778=DIRECTION('',(0.496992860897903,0.866025403784439,0.054754873906508));
#19779=DIRECTION('center_axis',(0.86081688607418,-0.5,0.0948382235680992));
#19780=DIRECTION('ref_axis',(0.109509747813016,-1.37062880361661E-18,-0.993985721795806));
#19781=DIRECTION('',(-0.109509747813016,1.50231459873716E-16,0.993985721795806));
#19782=DIRECTION('',(0.496992860897903,0.866025403784439,0.054754873906508));
#19783=DIRECTION('',(0.109509747813016,-3.00462919747432E-16,-0.993985721795806));
#19784=DIRECTION('center_axis',(0.496992860897903,0.866025403784439,0.0547548739065076));
#19785=DIRECTION('ref_axis',(0.109509747813015,-2.68836199388207E-18,-0.993985721795806));
#19786=DIRECTION('center_axis',(0.496992860897903,0.866025403784439,0.0547548739065076));
#19787=DIRECTION('ref_axis',(-0.86081688607418,0.5,-0.0948382235680945));
#19788=DIRECTION('',(-0.86081688607418,0.5,-0.0948382235680992));
#19789=DIRECTION('',(0.86081688607418,-0.5,0.0948382235680992));
#19790=DIRECTION('',(-0.109509747813016,0.,0.993985721795806));
#19791=DIRECTION('',(0.86081688607418,-0.5,0.0948382235680992));
#19792=DIRECTION('',(-0.86081688607418,0.5,-0.0948382235680992));
#19793=DIRECTION('center_axis',(-0.86081688607418,0.5,-0.0948382235680992));
#19794=DIRECTION('ref_axis',(-0.109509747813016,1.37062880361661E-18,0.993985721795806));
#19795=DIRECTION('',(0.496992860897903,0.866025403784439,0.0547548739065076));
#19796=DIRECTION('',(0.109509747813016,3.12982208070242E-16,-0.993985721795806));
#19797=DIRECTION('',(-0.496992860897903,-0.866025403784439,-0.0547548739065082));
#19798=DIRECTION('center_axis',(0.109509747813016,0.,-0.993985721795806));
#19799=DIRECTION('ref_axis',(0.,-1.,0.));
#19800=DIRECTION('',(0.86081688607418,-0.5,0.0948382235680992));
#19801=DIRECTION('center_axis',(-0.496992860897903,-0.866025403784439,-0.0547548739065078));
#19802=DIRECTION('ref_axis',(-0.86081688607418,0.5,-0.0948382235680992));
#19803=DIRECTION('',(-0.86081688607418,0.5,-0.0948382235680992));
#19804=DIRECTION('center_axis',(-0.496992860897903,-0.866025403784439,-0.0547548739065078));
#19805=DIRECTION('ref_axis',(0.86081688607418,-0.5,0.0948382235680946));
#19806=DIRECTION('',(-0.86081688607418,0.5,-0.0948382235680992));
#19807=DIRECTION('',(0.86081688607418,-0.5,0.0948382235680992));
#19808=DIRECTION('center_axis',(0.109509747813016,0.,-0.993985721795806));
#19809=DIRECTION('ref_axis',(0.,-1.,0.));
#19810=DIRECTION('',(-0.496992860897903,-0.866025403784439,-0.054754873906508));
#19811=DIRECTION('',(0.756106594798299,-0.64912524734226,0.0833020441848256));
#19812=DIRECTION('center_axis',(-0.109509747813016,0.,0.993985721795806));
#19813=DIRECTION('ref_axis',(0.993985721795806,0.,0.109509747813016));
#19814=DIRECTION('',(-0.756106594798299,0.64912524734226,-0.0833020441848256));
#19815=DIRECTION('center_axis',(-0.109509747813016,0.,0.993985721795806));
#19816=DIRECTION('ref_axis',(0.993985721795806,0.,0.109509747813016));
#19817=DIRECTION('center_axis',(0.496992860897903,0.866025403784439,0.054754873906508));
#19818=DIRECTION('ref_axis',(0.86081688607418,-0.5,0.0948382235680945));
#19819=DIRECTION('center_axis',(0.645221227515378,0.760681545236145,0.0710855421355126));
#19820=DIRECTION('ref_axis',(0.109509747813016,-3.16883939248426E-18,-0.993985721795806));
#19821=DIRECTION('',(-0.756106594798299,0.64912524734226,-0.0833020441848257));
#19822=DIRECTION('',(0.756106594798299,-0.64912524734226,0.0833020441848256));
#19823=DIRECTION('center_axis',(-0.645221227515378,-0.760681545236145,-0.0710855421355126));
#19824=DIRECTION('ref_axis',(-0.756106594798299,0.64912524734226,-0.0833020441848256));
#19825=DIRECTION('',(-0.756106594798299,0.64912524734226,-0.0833020441848256));
#19826=DIRECTION('',(0.756106594798299,-0.64912524734226,0.0833020441848256));
#19827=DIRECTION('center_axis',(-0.496992860897903,0.866025403784439,-0.054754873906508));
#19828=DIRECTION('ref_axis',(0.86081688607418,0.5,0.0948382235680945));
#19829=DIRECTION('center_axis',(-0.496992860897903,0.866025403784439,-0.0547548739065078));
#19830=DIRECTION('ref_axis',(-0.86081688607418,-0.5,-0.0948382235680946));
#19831=DIRECTION('',(-0.496992860897903,0.866025403784439,-0.054754873906508));
#19832=DIRECTION('center_axis',(0.496992860897903,-0.866025403784439,0.0547548739065076));
#19833=DIRECTION('ref_axis',(0.86081688607418,0.5,0.0948382235680945));
#19834=DIRECTION('',(0.496992860897903,-0.866025403784439,0.054754873906508));
#19835=DIRECTION('center_axis',(0.109509747813016,0.,-0.993985721795806));
#19836=DIRECTION('ref_axis',(0.,-1.,0.));
#19837=DIRECTION('',(0.756106594798299,-0.64912524734226,0.0833020441848256));
#19838=DIRECTION('',(-0.86081688607418,-0.5,-0.0948382235680992));
#19839=DIRECTION('',(-0.86081688607418,-0.5,-0.0948382235680992));
#19840=DIRECTION('center_axis',(-0.496992860897903,0.866025403784439,-0.0547548739065078));
#19841=DIRECTION('ref_axis',(-0.109509747813016,-8.62567737696967E-18,0.993985721795806));
#19842=DIRECTION('',(-0.109509747813016,-1.50231459873716E-16,0.993985721795806));
#19843=DIRECTION('center_axis',(-0.496992860897903,0.866025403784439,-0.0547548739065078));
#19844=DIRECTION('ref_axis',(-0.86081688607418,-0.5,-0.0948382235680946));
#19845=DIRECTION('',(-0.86081688607418,-0.5,-0.0948382235680992));
#19846=DIRECTION('center_axis',(-0.756106594798299,0.64912524734226,-0.0833020441848257));
#19847=DIRECTION('ref_axis',(0.645221227515378,0.760681545236146,0.0710855421355019));
#19848=DIRECTION('center_axis',(0.496992860897903,-0.866025403784439,0.054754873906508));
#19849=DIRECTION('ref_axis',(-0.86081688607418,-0.5,-0.0948382235680945));
#19850=DIRECTION('',(-0.496992860897903,0.866025403784439,-0.054754873906508));
#19851=DIRECTION('center_axis',(0.496992860897903,-0.866025403784439,0.0547548739065076));
#19852=DIRECTION('ref_axis',(0.86081688607418,0.5,0.0948382235680945));
#19853=DIRECTION('',(0.496992860897903,-0.866025403784439,0.054754873906508));
#19854=DIRECTION('center_axis',(-0.756106594798299,0.64912524734226,-0.0833020441848257));
#19855=DIRECTION('ref_axis',(0.645221227515378,0.760681545236146,0.0710855421355018));
#19856=DIRECTION('',(-0.756106594798299,0.64912524734226,-0.0833020441848256));
#19857=DIRECTION('center_axis',(0.756106594798299,-0.64912524734226,0.0833020441848257));
#19858=DIRECTION('ref_axis',(-0.645221227515378,-0.760681545236146,-0.0710855421355019));
#19859=DIRECTION('center_axis',(0.496992860897903,-0.866025403784439,0.0547548739065076));
#19860=DIRECTION('ref_axis',(0.109509747813016,4.04398041928102E-16,-0.993985721795806));
#19861=DIRECTION('',(-0.86081688607418,-0.5,-0.0948382235680992));
#19862=DIRECTION('',(0.109509747813016,3.00462919747432E-16,-0.993985721795806));
#19863=DIRECTION('center_axis',(0.109509747813016,0.,-0.993985721795806));
#19864=DIRECTION('ref_axis',(0.,-1.,0.));
#19865=DIRECTION('center_axis',(-0.756106594798299,0.64912524734226,-0.0833020441848257));
#19866=DIRECTION('ref_axis',(0.645221227515378,0.760681545236146,0.0710855421355019));
#19867=DIRECTION('center_axis',(-0.86081688607418,-0.5,-0.0948382235680992));
#19868=DIRECTION('ref_axis',(-0.496992860897903,0.866025403784439,-0.054754873906508));
#19869=DIRECTION('center_axis',(-0.109509747813016,0.,0.993985721795806));
#19870=DIRECTION('ref_axis',(0.993985721795806,0.,0.109509747813016));
#19871=DIRECTION('center_axis',(-0.109509747813016,0.,0.993985721795806));
#19872=DIRECTION('ref_axis',(0.993985721795806,0.,0.109509747813016));
#19873=DIRECTION('center_axis',(0.109509747813016,0.,-0.993985721795806));
#19874=DIRECTION('ref_axis',(0.,-1.,0.));
#19875=DIRECTION('center_axis',(0.109509747813016,0.,-0.993985721795806));
#19876=DIRECTION('ref_axis',(0.,-1.,0.));
#19877=DIRECTION('center_axis',(0.,1.,0.));
#19878=DIRECTION('ref_axis',(0.993985721795806,0.,0.109509747813016));
#19879=DIRECTION('',(-0.993985721795806,0.,-0.109509747813016));
#19880=DIRECTION('',(-0.109509747813016,0.,0.993985721795806));
#19881=DIRECTION('',(-0.993985721795806,0.,-0.109509747813016));
#19882=DIRECTION('',(-0.109509747813016,0.,0.993985721795806));
#19883=DIRECTION('center_axis',(0.993985721795806,0.,0.109509747813016));
#19884=DIRECTION('ref_axis',(0.,1.,0.));
#19885=DIRECTION('',(0.,1.,0.));
#19886=DIRECTION('',(-0.109509747813016,0.,0.993985721795806));
#19887=DIRECTION('',(0.,1.,0.));
#19888=DIRECTION('center_axis',(-0.993985721795806,0.,-0.109509747813016));
#19889=DIRECTION('ref_axis',(-0.109509747813016,0.,0.993985721795806));
#19890=DIRECTION('',(0.,1.,0.));
#19891=DIRECTION('',(-0.109509747813016,0.,0.993985721795806));
#19892=DIRECTION('',(0.,1.,0.));
#19893=DIRECTION('',(0.109509747813016,0.,-0.993985721795806));
#19894=DIRECTION('center_axis',(-0.109509747813016,0.,0.993985721795806));
#19895=DIRECTION('ref_axis',(-0.993985721795806,0.,-0.109509747813016));
#19896=DIRECTION('center_axis',(-0.109509747813016,0.,0.993985721795806));
#19897=DIRECTION('ref_axis',(0.993985721795806,0.,0.109509747813016));
#19898=DIRECTION('',(-0.109509747813016,0.,0.993985721795806));
#19899=DIRECTION('center_axis',(0.109509747813016,0.,-0.993985721795806));
#19900=DIRECTION('ref_axis',(0.993985721795806,0.,0.109509747813016));
#19901=DIRECTION('center_axis',(0.,1.,0.));
#19902=DIRECTION('ref_axis',(0.993985721795806,0.,0.109509747813016));
#19903=DIRECTION('',(0.993985721795806,0.,0.109509747813016));
#19904=DIRECTION('',(0.109509747813016,0.,-0.993985721795806));
#19905=DIRECTION('',(0.993985721795806,0.,0.109509747813016));
#19906=DIRECTION('center_axis',(-0.109509747813016,0.,0.993985721795806));
#19907=DIRECTION('ref_axis',(-0.993985721795806,0.,-0.109509747813016));
#19908=DIRECTION('center_axis',(-0.109509747813016,0.,0.993985721795806));
#19909=DIRECTION('ref_axis',(0.993985721795806,0.,0.109509747813016));
#19910=DIRECTION('',(-0.109509747813016,0.,0.993985721795806));
#19911=DIRECTION('center_axis',(0.109509747813016,0.,-0.993985721795806));
#19912=DIRECTION('ref_axis',(0.993985721795806,0.,0.109509747813016));
#19913=DIRECTION('center_axis',(0.993985721795806,0.,0.109509747813016));
#19914=DIRECTION('ref_axis',(0.,1.,0.));
#19915=DIRECTION('',(0.,-1.,0.));
#19916=DIRECTION('',(0.,-1.,0.));
#19917=DIRECTION('',(0.109509747813016,0.,-0.993985721795806));
#19918=DIRECTION('center_axis',(-0.109509747813016,0.,0.993985721795806));
#19919=DIRECTION('ref_axis',(0.993985721795806,0.,0.109509747813016));
#19920=DIRECTION('center_axis',(-0.109509747813016,0.,0.993985721795806));
#19921=DIRECTION('ref_axis',(0.993985721795806,0.,0.109509747813016));
#19922=DIRECTION('',(-0.993985721795806,0.,-0.109509747813016));
#19923=DIRECTION('center_axis',(-0.109509747813016,0.,0.993985721795806));
#19924=DIRECTION('ref_axis',(0.993985721795806,0.,0.109509747813016));
#19925=DIRECTION('center_axis',(-0.109509747813016,0.,0.993985721795806));
#19926=DIRECTION('ref_axis',(-0.993985721795806,0.,-0.109509747813016));
#19927=DIRECTION('',(-0.109509747813016,0.,0.993985721795806));
#19928=DIRECTION('center_axis',(0.109509747813016,0.,-0.993985721795806));
#19929=DIRECTION('ref_axis',(0.993985721795806,0.,0.109509747813016));
#19930=DIRECTION('center_axis',(-0.109509747813016,0.,0.993985721795806));
#19931=DIRECTION('ref_axis',(0.993985721795806,0.,0.109509747813016));
#19932=DIRECTION('',(-0.993985721795806,0.,-0.109509747813016));
#19933=DIRECTION('center_axis',(0.109509747813016,0.,-0.993985721795806));
#19934=DIRECTION('ref_axis',(0.993985721795806,0.,0.109509747813016));
#19935=DIRECTION('',(0.993985721795806,0.,0.109509747813016));
#19936=DIRECTION('',(0.,-1.,0.));
#19937=DIRECTION('center_axis',(0.,-1.,0.));
#19938=DIRECTION('ref_axis',(0.109509747813016,0.,-0.993985721795806));
#19939=DIRECTION('',(0.109509747813016,0.,-0.993985721795806));
#19940=DIRECTION('center_axis',(0.,-1.,0.));
#19941=DIRECTION('ref_axis',(0.109509747813016,0.,-0.993985721795806));
#19942=DIRECTION('',(-0.109509747813016,0.,0.993985721795806));
#19943=DIRECTION('',(0.993985721795806,0.,0.109509747813016));
#19944=DIRECTION('center_axis',(0.109509747813016,0.,-0.993985721795806));
#19945=DIRECTION('ref_axis',(0.,-1.,0.));
#19946=DIRECTION('',(0.,-1.,0.));
#19947=DIRECTION('center_axis',(-0.993985721795806,0.,-0.109509747813016));
#19948=DIRECTION('ref_axis',(-0.109509747813016,0.,0.993985721795806));
#19949=DIRECTION('center_axis',(-0.109509747813016,0.,0.993985721795806));
#19950=DIRECTION('ref_axis',(-0.993985721795806,0.,-0.109509747813016));
#19951=DIRECTION('axis',(0.,0.,1.));
#19952=DIRECTION('refdir',(1.,0.,0.));
#19953=DIRECTION('center_axis',(0.,-1.,0.));
#19954=DIRECTION('ref_axis',(0.,0.,-1.));
#19955=DIRECTION('',(-1.27406007682284E-17,-0.994573647104338,0.104034900324722));
#19956=DIRECTION('center_axis',(0.,1.,0.));
#19957=DIRECTION('ref_axis',(0.645833333333334,0.,-0.763478425075362));
#19958=DIRECTION('',(-1.27406007682284E-17,-0.994573647104339,0.104034900324722));
#19959=DIRECTION('center_axis',(0.,1.,0.));
#19960=DIRECTION('ref_axis',(-0.985799694950984,0.,-0.167925463925357));
#19961=DIRECTION('center_axis',(-0.4309815049242,-0.76811996556279,0.473546894105632));
#19962=DIRECTION('ref_axis',(-5.07348349240606E-16,0.524786664869244,0.85123378479441));
#19963=DIRECTION('center_axis',(0.4309815049242,0.76811996556279,-0.473546894105632));
#19964=DIRECTION('ref_axis',(5.07348349240606E-16,-0.524786664869244,-0.85123378479441));
#19965=DIRECTION('',(0.430981504924199,0.76811996556279,-0.473546894105633));
#19966=DIRECTION('center_axis',(-0.4309815049242,-0.76811996556279,0.473546894105632));
#19967=DIRECTION('ref_axis',(-5.07348349240606E-16,0.524786664869244,0.85123378479441));
#19968=DIRECTION('',(-0.430981504924199,-0.76811996556279,0.473546894105632));
#19969=DIRECTION('center_axis',(0.,-1.,0.));
#19970=DIRECTION('ref_axis',(0.,0.,1.));
#19971=DIRECTION('center_axis',(0.,1.,0.));
#19972=DIRECTION('ref_axis',(1.,0.,0.));
#19973=DIRECTION('',(0.,1.,0.));
#19974=DIRECTION('center_axis',(0.,1.,0.));
#19975=DIRECTION('ref_axis',(1.,0.,0.));
#19976=DIRECTION('',(0.,1.,0.));
#19977=DIRECTION('center_axis',(0.109509747813017,0.,-0.993985721795806));
#19978=DIRECTION('ref_axis',(0.993985721795806,0.,0.109509747813017));
#19979=DIRECTION('',(0.109509747813017,0.,-0.993985721795806));
#19980=DIRECTION('center_axis',(0.109509747813017,0.,-0.993985721795806));
#19981=DIRECTION('ref_axis',(-0.993985721795806,0.,-0.109509747813017));
#19982=DIRECTION('center_axis',(0.,1.,0.));
#19983=DIRECTION('ref_axis',(0.,0.,-1.));
#19984=DIRECTION('center_axis',(0.,-1.,0.));
#19985=DIRECTION('ref_axis',(0.739563468005766,0.,0.673086827081978));
#19986=DIRECTION('',(0.,1.,0.));
#19987=DIRECTION('center_axis',(0.,1.,0.));
#19988=DIRECTION('ref_axis',(0.,0.,1.));
#19989=DIRECTION('center_axis',(0.4309815049242,0.76811996556279,-0.473546894105632));
#19990=DIRECTION('ref_axis',(3.700389135243E-16,-0.524786664869244,-0.85123378479441));
#19991=DIRECTION('center_axis',(0.4309815049242,0.76811996556279,-0.473546894105632));
#19992=DIRECTION('ref_axis',(0.739563468005766,-1.35479487508513E-16,0.673086827081978));
#19993=DIRECTION('',(0.4309815049242,0.76811996556279,-0.473546894105632));
#19994=DIRECTION('center_axis',(0.4309815049242,0.76811996556279,-0.473546894105632));
#19995=DIRECTION('ref_axis',(-2.09125183283633E-15,-0.524786664869243,-0.851233784794411));
#19996=DIRECTION('center_axis',(-0.4309815049242,-0.76811996556279,0.473546894105632));
#19997=DIRECTION('ref_axis',(0.739563468005766,-3.21197772818101E-17,0.673086827081978));
#19998=DIRECTION('',(0.4309815049242,0.76811996556279,-0.473546894105632));
#19999=DIRECTION('center_axis',(-0.4309815049242,-0.76811996556279,0.473546894105632));
#20000=DIRECTION('ref_axis',(7.7903033594954E-16,-0.524786664869244,-0.85123378479441));
#20001=DIRECTION('center_axis',(0.,1.,0.));
#20002=DIRECTION('ref_axis',(0.,0.,-1.));
#20003=DIRECTION('center_axis',(0.,-1.,0.));
#20004=DIRECTION('ref_axis',(0.739563468005766,0.,0.673086827081978));
#20005=DIRECTION('',(0.,1.,0.));
#20006=DIRECTION('center_axis',(0.,1.,0.));
#20007=DIRECTION('ref_axis',(0.,0.,1.));
#20008=DIRECTION('center_axis',(0.,-1.,0.));
#20009=DIRECTION('ref_axis',(0.,0.,1.));
#20010=DIRECTION('center_axis',(0.,1.,0.));
#20011=DIRECTION('ref_axis',(1.,0.,0.));
#20012=DIRECTION('',(0.,-1.,0.));
#20013=DIRECTION('center_axis',(0.,1.,0.));
#20014=DIRECTION('ref_axis',(0.,0.,1.));
#20015=DIRECTION('center_axis',(0.,-1.,0.));
#20016=DIRECTION('ref_axis',(0.,0.,1.));
#20017=DIRECTION('center_axis',(0.,1.,0.));
#20018=DIRECTION('ref_axis',(1.,0.,0.));
#20019=DIRECTION('',(0.,-1.,0.));
#20020=DIRECTION('center_axis',(0.,1.,0.));
#20021=DIRECTION('ref_axis',(0.,0.,1.));
#20022=DIRECTION('center_axis',(0.,1.,0.));
#20023=DIRECTION('ref_axis',(0.,0.,-1.));
#20024=DIRECTION('center_axis',(0.,1.,0.));
#20025=DIRECTION('ref_axis',(1.,0.,0.));
#20026=DIRECTION('',(0.,-1.,0.));
#20027=DIRECTION('center_axis',(0.,1.,0.));
#20028=DIRECTION('ref_axis',(1.,0.,0.));
#20029=DIRECTION('',(0.,-1.,0.));
#20030=DIRECTION('center_axis',(0.109509747813017,0.,-0.993985721795806));
#20031=DIRECTION('ref_axis',(-0.993985721795806,0.,-0.109509747813017));
#20032=DIRECTION('center_axis',(0.109509747813017,0.,-0.993985721795806));
#20033=DIRECTION('ref_axis',(-0.993985721795806,0.,-0.109509747813017));
#20034=DIRECTION('',(-0.780289129569036,8.65956056235497E-17,0.625418958999803));
#20035=DIRECTION('center_axis',(-0.109509747813017,0.,0.993985721795806));
#20036=DIRECTION('ref_axis',(-0.993985721795806,0.,-0.109509747813017));
#20037=DIRECTION('center_axis',(-0.109509747813017,0.,0.993985721795806));
#20038=DIRECTION('ref_axis',(-0.993985721795806,0.,-0.109509747813017));
#20039=DIRECTION('center_axis',(-0.109509747813017,0.,0.993985721795806));
#20040=DIRECTION('ref_axis',(0.993985721795806,0.,0.109509747813017));
#20041=DIRECTION('',(-0.109509747813017,0.,0.993985721795806));
#20042=DIRECTION('center_axis',(-0.109509747813017,0.,0.993985721795806));
#20043=DIRECTION('ref_axis',(0.993985721795806,0.,0.109509747813017));
#20044=DIRECTION('center_axis',(-0.109509747813017,0.,0.993985721795806));
#20045=DIRECTION('ref_axis',(-0.993985721795806,0.,-0.109509747813017));
#20046=DIRECTION('',(0.109509747813017,0.,-0.993985721795806));
#20047=DIRECTION('center_axis',(0.109509747813016,0.,-0.993985721795806));
#20048=DIRECTION('ref_axis',(0.993985721795806,0.,0.109509747813016));
#20049=DIRECTION('center_axis',(0.109509747813017,0.,-0.993985721795806));
#20050=DIRECTION('ref_axis',(0.993985721795806,0.,0.109509747813017));
#20051=DIRECTION('center_axis',(0.109509747813017,0.,-0.993985721795806));
#20052=DIRECTION('ref_axis',(0.993985721795806,0.,0.109509747813017));
#20053=DIRECTION('',(0.109509747813017,0.,-0.993985721795806));
#20054=DIRECTION('center_axis',(0.109509747813017,0.,-0.993985721795806));
#20055=DIRECTION('ref_axis',(0.993985721795806,0.,0.109509747813017));
#20056=DIRECTION('center_axis',(0.109509747813017,0.,-0.993985721795806));
#20057=DIRECTION('ref_axis',(0.,-1.,0.));
#20058=DIRECTION('center_axis',(0.109509747813017,0.,-0.993985721795806));
#20059=DIRECTION('ref_axis',(0.,-1.,0.));
#20060=DIRECTION('center_axis',(0.109509747813017,0.,-0.993985721795806));
#20061=DIRECTION('ref_axis',(0.,-1.,0.));
#20062=DIRECTION('center_axis',(-0.167925463925357,0.,0.985799694950984));
#20063=DIRECTION('ref_axis',(0.,1.,0.));
#20064=DIRECTION('',(-0.985799694950984,0.,-0.167925463925357));
#20065=DIRECTION('',(-0.985799694950984,0.,-0.167925463925357));
#20066=DIRECTION('',(0.,-1.,0.));
#20067=DIRECTION('center_axis',(-0.718304971572534,0.,-0.695728372149779));
#20068=DIRECTION('ref_axis',(-0.695728372149779,0.,0.718304971572534));
#20069=DIRECTION('',(0.695728372149779,0.,-0.718304971572534));
#20070=DIRECTION('',(0.,-1.,0.));
#20071=DIRECTION('',(0.695728372149779,0.,-0.718304971572534));
#20072=DIRECTION('',(0.,-1.,0.));
#20073=DIRECTION('center_axis',(-0.17364817766693,0.,-0.984807753012208));
#20074=DIRECTION('ref_axis',(-0.984807753012208,0.,0.17364817766693));
#20075=DIRECTION('',(0.984807753012208,0.,-0.17364817766693));
#20076=DIRECTION('',(0.984807753012208,0.,-0.17364817766693));
#20077=DIRECTION('',(0.,-1.,0.));
#20078=DIRECTION('center_axis',(0.64278760968654,0.,-0.766044443118978));
#20079=DIRECTION('ref_axis',(0.,-1.,0.));
#20080=DIRECTION('',(0.766044443118978,0.,0.64278760968654));
#20081=DIRECTION('',(0.766044443118978,0.,0.64278760968654));
#20082=DIRECTION('',(0.766044443118978,0.,0.64278760968654));
#20083=DIRECTION('',(0.,-1.,0.));
#20084=DIRECTION('center_axis',(0.982829341293941,0.,-0.184516898661661));
#20085=DIRECTION('ref_axis',(0.,-1.,0.));
#20086=DIRECTION('',(0.184516898661661,0.,0.982829341293941));
#20087=DIRECTION('',(0.,-1.,0.));
#20088=DIRECTION('',(0.184516898661661,0.,0.982829341293941));
#20089=DIRECTION('center_axis',(0.763478425075362,0.,0.645833333333334));
#20090=DIRECTION('ref_axis',(0.,-1.,0.));
#20091=DIRECTION('',(0.645833333333334,0.,-0.763478425075362));
#20092=DIRECTION('',(0.645833333333334,0.,-0.763478425075362));
#20093=DIRECTION('',(0.,1.,0.));
#20094=DIRECTION('center_axis',(0.,-1.,0.));
#20095=DIRECTION('ref_axis',(0.,0.,1.));
#20096=DIRECTION('center_axis',(0.,1.,0.));
#20097=DIRECTION('ref_axis',(-1.,0.,0.));
#20098=DIRECTION('center_axis',(0.,1.,0.));
#20099=DIRECTION('ref_axis',(-1.,0.,0.));
#20100=DIRECTION('',(0.,1.,0.));
#20101=DIRECTION('center_axis',(0.763478425075362,0.,-0.645833333333334));
#20102=DIRECTION('ref_axis',(0.,-1.,0.));
#20103=DIRECTION('',(-0.645833333333334,0.,-0.763478425075362));
#20104=DIRECTION('',(-0.645833333333334,0.,-0.763478425075362));
#20105=DIRECTION('',(0.,1.,0.));
#20106=DIRECTION('center_axis',(0.,-1.,0.));
#20107=DIRECTION('ref_axis',(-1.22464679914735E-16,0.,-1.));
#20108=DIRECTION('center_axis',(0.,1.,0.));
#20109=DIRECTION('ref_axis',(1.,0.,0.));
#20110=DIRECTION('center_axis',(0.,1.,0.));
#20111=DIRECTION('ref_axis',(1.,0.,0.));
#20112=DIRECTION('',(0.,1.,0.));
#20113=DIRECTION('center_axis',(-0.763478425075362,0.,-0.645833333333334));
#20114=DIRECTION('ref_axis',(-0.645833333333334,0.,0.763478425075362));
#20115=DIRECTION('',(-0.645833333333334,0.,0.763478425075362));
#20116=DIRECTION('',(-0.645833333333334,0.,0.763478425075362));
#20117=DIRECTION('',(0.,1.,0.));
#20118=DIRECTION('center_axis',(0.,-1.,0.));
#20119=DIRECTION('ref_axis',(0.,0.,1.));
#20120=DIRECTION('',(0.,-1.,0.));
#20121=DIRECTION('center_axis',(0.,1.,0.));
#20122=DIRECTION('ref_axis',(1.,0.,0.));
#20123=DIRECTION('center_axis',(0.,1.,0.));
#20124=DIRECTION('ref_axis',(1.,0.,0.));
#20125=DIRECTION('center_axis',(0.4309815049242,0.76811996556279,-0.473546894105632));
#20126=DIRECTION('ref_axis',(5.07348349240606E-16,-0.524786664869244,-0.85123378479441));
#20127=DIRECTION('center_axis',(-0.4309815049242,-0.76811996556279,0.473546894105632));
#20128=DIRECTION('ref_axis',(-3.9632604677809E-16,0.524786664869244,0.85123378479441));
#20129=DIRECTION('',(-0.430981504924199,-0.76811996556279,0.473546894105632));
#20130=DIRECTION('center_axis',(0.4309815049242,0.76811996556279,-0.473546894105632));
#20131=DIRECTION('ref_axis',(5.07348349240606E-16,-0.524786664869244,-0.85123378479441));
#20132=DIRECTION('',(0.430981504924199,0.76811996556279,-0.473546894105632));
#20133=DIRECTION('center_axis',(-0.109509747813016,0.,0.993985721795806));
#20134=DIRECTION('ref_axis',(0.,1.,0.));
#20135=DIRECTION('',(-0.993985721795806,0.,-0.109509747813017));
#20136=DIRECTION('',(0.,-1.,0.));
#20137=DIRECTION('',(-0.993985721795806,0.,-0.109509747813017));
#20138=DIRECTION('',(0.,-1.,0.));
#20139=DIRECTION('center_axis',(0.,1.,0.));
#20140=DIRECTION('ref_axis',(1.,0.,0.));
#20141=DIRECTION('',(-0.673086827081978,2.93742993772391E-16,0.739563468005766));
#20142=DIRECTION('',(0.645833333333333,0.,0.763478425075362));
#20143=DIRECTION('',(-0.673086827081978,2.93742993772391E-16,0.739563468005766));
#20144=DIRECTION('',(0.739563468005766,0.,0.673086827081978));
#20145=DIRECTION('center_axis',(-0.763478425075362,0.,0.645833333333334));
#20146=DIRECTION('ref_axis',(0.,1.,0.));
#20147=DIRECTION('',(0.645833333333333,0.,0.763478425075362));
#20148=DIRECTION('',(0.,-1.,0.));
#20149=DIRECTION('center_axis',(0.4309815049242,0.76811996556279,-0.473546894105632));
#20150=DIRECTION('ref_axis',(-0.739563468005766,3.32136590985229E-17,-0.673086827081978));
#20151=DIRECTION('',(-0.517011430438976,0.640305956948566,0.568073465576086));
#20152=DIRECTION('',(0.739563468005766,0.,0.673086827081978));
#20153=DIRECTION('',(-0.517011430438976,0.640305956948566,0.568073465576086));
#20154=DIRECTION('center_axis',(-0.739563468005766,0.,-0.673086827081978));
#20155=DIRECTION('ref_axis',(-0.673086827081978,0.,0.739563468005766));
#20156=DIRECTION('',(0.517011430438976,-0.640305956948566,-0.568073465576087));
#20157=DIRECTION('',(-0.673086827081978,0.,0.739563468005766));
#20158=DIRECTION('',(0.673086827081978,0.,-0.739563468005766));
#20159=DIRECTION('',(0.673086827081978,0.,-0.739563468005766));
#20160=DIRECTION('',(0.424474651014543,0.776076502349984,-0.46639739830567));
#20161=DIRECTION('center_axis',(0.522366870539629,-0.630638773387917,-0.573957829515739));
#20162=DIRECTION('ref_axis',(-1.65075943026669E-17,0.673089942300288,-0.73956063279098));
#20163=DIRECTION('',(0.739563468005766,0.,0.673086827081978));
#20164=DIRECTION('',(0.739563468005766,0.,0.673086827081978));
#20165=DIRECTION('',(0.424474651014543,0.776076502349984,-0.46639739830567));
#20166=DIRECTION('',(0.739563468005766,0.,0.673086827081978));
#20167=DIRECTION('center_axis',(0.,-1.,0.));
#20168=DIRECTION('ref_axis',(0.,0.,-1.));
#20169=DIRECTION('center_axis',(0.,1.,0.));
#20170=DIRECTION('ref_axis',(1.,0.,0.));
#20171=DIRECTION('center_axis',(0.176227439339188,0.,-0.984349475351083));
#20172=DIRECTION('ref_axis',(0.,-1.,0.));
#20173=DIRECTION('',(0.984349475351083,0.,0.176227439339188));
#20174=DIRECTION('',(0.,-1.,0.));
#20175=DIRECTION('',(0.984349475351083,0.,0.176227439339188));
#20176=DIRECTION('',(0.,-1.,0.));
#20177=DIRECTION('center_axis',(0.,1.,0.));
#20178=DIRECTION('ref_axis',(1.,0.,0.));
#20179=DIRECTION('center_axis',(0.,1.,0.));
#20180=DIRECTION('ref_axis',(1.,0.,0.));
#20181=DIRECTION('center_axis',(0.,1.,0.));
#20182=DIRECTION('ref_axis',(-1.,0.,0.));
#20183=DIRECTION('',(-0.176227439496628,0.,-0.984349475322897));
#20184=DIRECTION('center_axis',(0.,1.,0.));
#20185=DIRECTION('ref_axis',(1.,0.,0.));
#20186=DIRECTION('center_axis',(0.,1.,0.));
#20187=DIRECTION('ref_axis',(0.,0.,-1.));
#20188=DIRECTION('center_axis',(0.,1.,0.));
#20189=DIRECTION('ref_axis',(1.,0.,0.));
#20190=DIRECTION('center_axis',(0.,1.,0.));
#20191=DIRECTION('ref_axis',(1.,0.,0.));
#20192=DIRECTION('',(0.,-1.,0.));
#20193=DIRECTION('center_axis',(0.,-1.,0.));
#20194=DIRECTION('ref_axis',(0.,0.,-1.));
#20195=DIRECTION('',(-0.176227439496628,0.,-0.984349475322897));
#20196=DIRECTION('',(0.,0.,1.));
#20197=DIRECTION('center_axis',(0.,1.,0.));
#20198=DIRECTION('ref_axis',(1.,0.,0.));
#20199=DIRECTION('',(-0.673086827081978,0.,0.739563468005766));
#20200=DIRECTION('',(-0.131887341059678,0.,-0.991264712005934));
#20201=DIRECTION('',(0.,0.,1.));
#20202=DIRECTION('',(-0.758169482971429,0.,0.652057539708603));
#20203=DIRECTION('center_axis',(0.652057539708603,0.,0.758169482971429));
#20204=DIRECTION('ref_axis',(0.,-1.,0.));
#20205=DIRECTION('',(0.,-1.,0.));
#20206=DIRECTION('',(-0.758169482971429,0.,0.652057539708603));
#20207=DIRECTION('center_axis',(1.,0.,0.));
#20208=DIRECTION('ref_axis',(0.,1.,0.));
#20209=DIRECTION('',(0.,0.,1.));
#20210=DIRECTION('center_axis',(0.,1.,0.));
#20211=DIRECTION('ref_axis',(1.,0.,0.));
#20212=DIRECTION('',(-0.176227439496628,0.,-0.984349475322897));
#20213=DIRECTION('center_axis',(0.,1.,0.));
#20214=DIRECTION('ref_axis',(-1.,0.,0.));
#20215=DIRECTION('center_axis',(0.,1.,0.));
#20216=DIRECTION('ref_axis',(1.,0.,0.));
#20217=DIRECTION('center_axis',(-0.984349475322897,0.,0.176227439496628));
#20218=DIRECTION('ref_axis',(0.,1.,0.));
#20219=DIRECTION('',(0.,-1.,0.));
#20220=DIRECTION('center_axis',(0.,1.,0.));
#20221=DIRECTION('ref_axis',(0.707106781243096,0.,0.707106781129999));
#20222=DIRECTION('center_axis',(-0.4309815049242,-0.76811996556279,0.473546894105632));
#20223=DIRECTION('ref_axis',(-0.872101888572109,0.489324325932158,-1.43093366045896E-19));
#20224=DIRECTION('',(0.739563468005766,0.,0.673086827081978));
#20225=DIRECTION('',(0.517011430438976,-0.640305956948566,-0.568073465576087));
#20226=DIRECTION('center_axis',(0.517011430438976,-0.640305956948566,-0.568073465576086));
#20227=DIRECTION('ref_axis',(-2.77812299687849E-17,0.663653900301021,-0.748039772081166));
#20228=DIRECTION('center_axis',(0.,1.,0.));
#20229=DIRECTION('ref_axis',(1.,0.,0.));
#20230=DIRECTION('',(-0.131887341059678,0.,-0.991264712005934));
#20231=DIRECTION('center_axis',(0.,1.,0.));
#20232=DIRECTION('ref_axis',(1.,0.,0.));
#20233=DIRECTION('center_axis',(-0.991264712005934,0.,0.131887341059678));
#20234=DIRECTION('ref_axis',(0.,1.,0.));
#20235=DIRECTION('',(0.,-1.,0.));
#20236=DIRECTION('center_axis',(-0.739563468005766,0.,-0.673086827081978));
#20237=DIRECTION('ref_axis',(-0.673086827081978,0.,0.739563468005766));
#20238=DIRECTION('',(0.673086827081978,0.,-0.739563468005766));
#20239=DIRECTION('center_axis',(0.,-1.,0.));
#20240=DIRECTION('ref_axis',(0.,0.,-1.));
#20241=DIRECTION('center_axis',(0.,1.,0.));
#20242=DIRECTION('ref_axis',(1.,0.,0.));
#20243=DIRECTION('center_axis',(0.,1.,0.));
#20244=DIRECTION('ref_axis',(0.,0.,-1.));
#20245=DIRECTION('axis',(0.,0.,1.));
#20246=DIRECTION('refdir',(1.,0.,0.));
#20247=DIRECTION('center_axis',(0.,-1.,0.));
#20248=DIRECTION('ref_axis',(0.,0.,-1.));
#20249=DIRECTION('center_axis',(0.616244820322966,0.0279867525047081,-0.787057217176334));
#20250=DIRECTION('ref_axis',(0.787551815229396,-0.0245787495049397,0.615758088376967));
#20251=DIRECTION('center_axis',(0.,1.,0.));
#20252=DIRECTION('ref_axis',(0.,0.,1.));
#20253=DIRECTION('center_axis',(0.0586169709474566,1.30991163966162E-16,
0.998280547099334));
#20254=DIRECTION('ref_axis',(0.998280547099334,-9.82981897176464E-33,-0.0586169709474566));
#20255=DIRECTION('center_axis',(0.0586169709474566,1.30991163966162E-16,
0.998280547099334));
#20256=DIRECTION('ref_axis',(0.998280547099334,-9.82981897176464E-33,-0.0586169709474566));
#20257=DIRECTION('center_axis',(0.,-1.,0.));
#20258=DIRECTION('ref_axis',(0.,0.,1.));
#20259=DIRECTION('center_axis',(0.,1.,0.));
#20260=DIRECTION('ref_axis',(0.,0.,-1.));
#20261=DIRECTION('center_axis',(-6.12303176911189E-17,-1.,3.41304790901886E-16));
#20262=DIRECTION('ref_axis',(-8.90039129279581E-34,3.41304790901886E-16,
1.));
#20263=DIRECTION('',(0.,-1.,0.));
#20264=DIRECTION('center_axis',(6.12303176911189E-17,1.,-3.41304790901886E-16));
#20265=DIRECTION('ref_axis',(2.09156632226363E-34,-3.41304790901886E-16,
-1.));
#20266=DIRECTION('center_axis',(1.,-6.12303176911189E-17,0.));
#20267=DIRECTION('ref_axis',(6.12303176911189E-17,1.,0.));
#20268=DIRECTION('',(-0.999877952034695,0.0156230930005404,1.91327708358932E-18));
#20269=DIRECTION('center_axis',(1.,-6.12303176911189E-17,0.));
#20270=DIRECTION('ref_axis',(6.12303176911189E-17,1.,0.));
#20271=DIRECTION('center_axis',(1.,-6.12303176911189E-17,0.));
#20272=DIRECTION('ref_axis',(6.12303176911189E-17,1.,0.));
#20273=DIRECTION('center_axis',(1.,-6.12303176911189E-17,0.));
#20274=DIRECTION('ref_axis',(6.12303176911189E-17,1.,0.));
#20275=DIRECTION('center_axis',(1.,0.,0.));
#20276=DIRECTION('ref_axis',(0.,0.,-1.));
#20277=DIRECTION('center_axis',(-1.,0.,0.));
#20278=DIRECTION('ref_axis',(0.,0.,-1.));
#20279=DIRECTION('center_axis',(0.,-1.,0.));
#20280=DIRECTION('ref_axis',(0.,0.,-1.));
#20281=DIRECTION('center_axis',(0.,1.,0.));
#20282=DIRECTION('ref_axis',(0.,0.,-1.));
#20283=DIRECTION('',(4.30002198846826E-17,0.936329177569045,-0.351123441588391));
#20284=DIRECTION('center_axis',(0.,-1.,0.));
#20285=DIRECTION('ref_axis',(0.,0.,-1.));
#20286=DIRECTION('center_axis',(0.,-1.,0.));
#20287=DIRECTION('ref_axis',(0.,0.,-1.));
#20288=DIRECTION('center_axis',(0.,-1.,0.));
#20289=DIRECTION('ref_axis',(0.,0.,-1.));
#20290=DIRECTION('center_axis',(0.,-1.,0.));
#20291=DIRECTION('ref_axis',(0.,0.,-1.));
#20292=DIRECTION('center_axis',(0.,-1.,0.));
#20293=DIRECTION('ref_axis',(0.,0.,-1.));
#20294=DIRECTION('center_axis',(0.,-1.,0.));
#20295=DIRECTION('ref_axis',(0.,0.,-1.));
#20296=DIRECTION('center_axis',(-1.,0.,-1.22464679914735E-16));
#20297=DIRECTION('ref_axis',(-1.22464679914735E-16,0.,1.));
#20298=DIRECTION('center_axis',(0.,1.,0.));
#20299=DIRECTION('ref_axis',(0.,0.,-1.));
#20300=DIRECTION('center_axis',(0.,-1.,0.));
#20301=DIRECTION('ref_axis',(0.,0.,-1.));
#20302=DIRECTION('',(0.,-1.,0.));
#20303=DIRECTION('center_axis',(0.,1.,0.));
#20304=DIRECTION('ref_axis',(0.,0.,1.));
#20305=DIRECTION('center_axis',(0.,1.,0.));
#20306=DIRECTION('ref_axis',(0.,0.,1.));
#20307=DIRECTION('center_axis',(0.,1.,0.));
#20308=DIRECTION('ref_axis',(0.,0.,-1.));
#20309=DIRECTION('',(0.,1.,0.));
#20310=DIRECTION('center_axis',(0.,1.,0.));
#20311=DIRECTION('ref_axis',(0.,0.,-1.));
#20312=DIRECTION('center_axis',(-0.0992537560260724,-0.0678968120752535,
0.992743025573454));
#20313=DIRECTION('ref_axis',(-0.78073602976301,-0.613230529687184,-0.119998205359365));
#20314=DIRECTION('center_axis',(0.,1.,0.));
#20315=DIRECTION('ref_axis',(0.,0.,1.));
#20316=DIRECTION('center_axis',(0.,1.,0.));
#20317=DIRECTION('ref_axis',(0.,0.,-1.));
#20318=DIRECTION('center_axis',(0.,1.,0.));
#20319=DIRECTION('ref_axis',(0.,0.,1.));
#20320=DIRECTION('center_axis',(0.,-1.,0.));
#20321=DIRECTION('ref_axis',(0.,0.,-1.));
#20322=DIRECTION('',(0.,-1.,0.));
#20323=DIRECTION('center_axis',(0.,-1.,-3.65204942310907E-16));
#20324=DIRECTION('ref_axis',(0.,-3.65204942310907E-16,1.));
#20325=DIRECTION('',(0.,1.,0.));
#20326=DIRECTION('center_axis',(-0.0235708115402593,-0.177622508721337,
0.983816375772874));
#20327=DIRECTION('ref_axis',(-0.0102596870461854,-0.983994984048997,-0.177900562641405));
#20328=DIRECTION('center_axis',(-0.0365025544384845,0.274626243368348,0.960857944741497));
#20329=DIRECTION('ref_axis',(-0.126726318578374,0.952464399007476,-0.277041529022093));
#20330=DIRECTION('center_axis',(-6.12303176911189E-17,-1.,3.41304790901886E-16));
#20331=DIRECTION('ref_axis',(0.,-3.41393580072236E-16,-1.));
#20332=DIRECTION('center_axis',(0.,1.,0.));
#20333=DIRECTION('ref_axis',(1.,0.,0.));
#20334=DIRECTION('center_axis',(-1.,6.12303176911189E-17,-1.22464679914735E-16));
#20335=DIRECTION('ref_axis',(-1.22464679914735E-16,3.40005801291454E-16,
1.));
#20336=DIRECTION('center_axis',(1.,0.,0.));
#20337=DIRECTION('ref_axis',(0.,-0.919145030018057,0.393919298579168));
#20338=DIRECTION('',(1.,0.,0.));
#20339=DIRECTION('center_axis',(-1.,6.12303176911189E-17,0.));
#20340=DIRECTION('ref_axis',(6.12303176911189E-17,1.,0.));
#20341=DIRECTION('',(-1.,0.,0.));
#20342=DIRECTION('center_axis',(0.,-1.,0.));
#20343=DIRECTION('ref_axis',(0.,0.,-1.));
#20344=DIRECTION('center_axis',(0.,1.,0.));
#20345=DIRECTION('ref_axis',(0.,0.,-1.));
#20346=DIRECTION('center_axis',(0.645833333333334,0.,0.763478425075362));
#20347=DIRECTION('ref_axis',(0.763478425075362,0.,-0.645833333333334));
#20348=DIRECTION('center_axis',(0.,-1.,0.));
#20349=DIRECTION('ref_axis',(0.,0.,-1.));
#20350=DIRECTION('center_axis',(-0.645833333333332,3.20901901721091E-15,
0.763478425075363));
#20351=DIRECTION('ref_axis',(0.763478425075363,1.69290416562703E-30,0.645833333333332));
#20352=DIRECTION('center_axis',(-6.12303176911189E-17,-1.,3.41304790901886E-16));
#20353=DIRECTION('ref_axis',(0.,-3.5527136788005E-16,-1.));
#20354=DIRECTION('center_axis',(-1.,6.12303176911189E-17,-1.22464679914735E-16));
#20355=DIRECTION('ref_axis',(-1.22464679914735E-16,3.33066907387547E-16,
1.));
#20356=DIRECTION('center_axis',(6.12303176911189E-17,1.,-3.41304790901886E-16));
#20357=DIRECTION('ref_axis',(8.90039129279581E-34,-3.41304790901886E-16,
-1.));
#20358=DIRECTION('center_axis',(-0.0528173258599627,0.994670318915973,-0.0885510404038205));
#20359=DIRECTION('ref_axis',(5.77315972805033E-14,-0.0886748135151963,-0.996060629403675));
#20360=DIRECTION('center_axis',(-0.830210692183039,-5.0361934159377E-5,
0.557449732306542));
#20361=DIRECTION('ref_axis',(0.554262125429395,0.106713543884745,0.825473025522971));
#20362=DIRECTION('center_axis',(-0.0514510747169759,-0.994945252858774,
0.0862364814000291));
#20363=DIRECTION('ref_axis',(-6.66133814775061E-14,0.0863508516932711,0.996264789306461));
#20364=DIRECTION('center_axis',(0.,-1.,0.));
#20365=DIRECTION('ref_axis',(0.491127762261646,0.,0.87108755078687));
#20366=DIRECTION('center_axis',(0.,1.,0.));
#20367=DIRECTION('ref_axis',(0.,0.,-1.));
#20368=DIRECTION('center_axis',(0.777751862218069,-1.11075125232563E-14,
-0.628571428571428));
#20369=DIRECTION('ref_axis',(0.628571428571428,-5.32211583197118E-30,0.777751862218069));
#20370=DIRECTION('center_axis',(-1.,0.,0.));
#20371=DIRECTION('ref_axis',(0.,0.,-1.));
#20372=DIRECTION('center_axis',(-1.,6.12303176911189E-17,0.));
#20373=DIRECTION('ref_axis',(6.12303176911189E-17,1.,0.));
#20374=DIRECTION('',(1.,0.,0.));
#20375=DIRECTION('center_axis',(-0.830143860196626,4.61445617944268E-5,
-0.557549252755776));
#20376=DIRECTION('ref_axis',(0.554525958306133,-0.103929478609263,-0.825651031029861));
#20377=DIRECTION('center_axis',(1.,0.,0.));
#20378=DIRECTION('ref_axis',(0.,0.919145030018077,-0.393919298579124));
#20379=DIRECTION('',(1.,0.,0.));
#20380=DIRECTION('center_axis',(-1.,6.12303176911189E-17,0.));
#20381=DIRECTION('ref_axis',(6.12303176911189E-17,1.,0.));
#20382=DIRECTION('',(-1.,0.,0.));
#20383=DIRECTION('center_axis',(-1.,6.12303176911189E-17,0.));
#20384=DIRECTION('ref_axis',(0.,-1.,0.));
#20385=DIRECTION('center_axis',(1.,-6.12303176911189E-17,0.));
#20386=DIRECTION('ref_axis',(-6.12303176911189E-17,-1.,0.));
#20387=DIRECTION('center_axis',(0.,0.844082777626921,-0.536212891036408));
#20388=DIRECTION('ref_axis',(0.,0.536212891036408,0.844082777626921));
#20389=DIRECTION('center_axis',(-1.,6.12303176911189E-17,0.));
#20390=DIRECTION('ref_axis',(-6.12303176911189E-17,-1.,0.));
#20391=DIRECTION('center_axis',(6.12303176911189E-17,1.,-5.4780741346636E-16));
#20392=DIRECTION('ref_axis',(-4.24099588001204E-33,-5.4780741346636E-16,
-1.));
#20393=DIRECTION('center_axis',(-6.12303176911189E-17,-1.,5.4780741346636E-16));
#20394=DIRECTION('ref_axis',(-4.24099588001204E-33,-5.4780741346636E-16,
-1.));
#20395=DIRECTION('',(6.12303176911189E-17,1.,-5.4780741346636E-16));
#20396=DIRECTION('center_axis',(-6.12303176911189E-17,-1.,5.4780741346636E-16));
#20397=DIRECTION('ref_axis',(-4.24099588001204E-33,-5.4780741346636E-16,
-1.));
#20398=DIRECTION('center_axis',(-0.993081091300346,-0.108852122504348,-0.0440586146855738));
#20399=DIRECTION('ref_axis',(-0.0460861135957196,0.706355459430216,-0.706355459430145));
#20400=DIRECTION('center_axis',(0.0392783824307495,-0.24484604714314,-0.968766030510981));
#20401=DIRECTION('ref_axis',(-0.0234136567132537,0.969022486825046,-0.245860164944867));
#20402=DIRECTION('center_axis',(0.997833402867506,0.0628604513358008,0.0194181301806716));
#20403=DIRECTION('ref_axis',(0.0307704812544108,-0.706771949600093,0.706771949600333));
#20404=DIRECTION('center_axis',(1.,-6.12303176911189E-17,0.));
#20405=DIRECTION('ref_axis',(0.,1.,0.));
#20406=DIRECTION('center_axis',(-1.,6.12303176911189E-17,0.));
#20407=DIRECTION('ref_axis',(6.12303176911189E-17,1.,0.));
#20408=DIRECTION('center_axis',(5.76857827429812E-17,0.942111439531992,
-0.335299918733898));
#20409=DIRECTION('ref_axis',(8.70539504324123E-32,-0.335299918733898,-0.942111439531992));
#20410=DIRECTION('center_axis',(1.,-6.12303176911189E-17,0.));
#20411=DIRECTION('ref_axis',(6.12303176911189E-17,1.,0.));
#20412=DIRECTION('center_axis',(0.,-0.942111439531976,-0.335299918733941));
#20413=DIRECTION('ref_axis',(0.,0.335299918733941,-0.942111439531976));
#20414=DIRECTION('center_axis',(0.,-0.844082777626919,0.53621289103641));
#20415=DIRECTION('ref_axis',(1.,1.81846874723086E-15,2.82341200227949E-15));
#20416=DIRECTION('center_axis',(0.,-0.844082777626919,0.53621289103641));
#20417=DIRECTION('ref_axis',(-1.,0.,0.));
#20418=DIRECTION('',(0.,0.844082777626919,-0.53621289103641));
#20419=DIRECTION('center_axis',(0.,-0.844082777626919,0.53621289103641));
#20420=DIRECTION('ref_axis',(0.,0.53621289103641,0.844082777626919));
#20421=DIRECTION('',(0.,0.844082777626919,-0.53621289103641));
#20422=DIRECTION('center_axis',(-1.,-3.40699396374318E-16,-5.3631402309558E-16));
#20423=DIRECTION('ref_axis',(5.3631402309558E-16,1.82721863935746E-31,-1.));
#20424=DIRECTION('',(1.,3.40699396374318E-16,5.3631402309558E-16));
#20425=DIRECTION('center_axis',(-0.707106781186508,0.379159771411456,0.596856655942839));
#20426=DIRECTION('ref_axis',(0.707106781186587,0.379159771411817,0.596856655942516));
#20427=DIRECTION('',(-1.,-3.40699396374318E-16,-5.3631402309558E-16));
#20428=DIRECTION('center_axis',(0.,1.,0.));
#20429=DIRECTION('ref_axis',(0.,0.,-1.));
#20430=DIRECTION('',(0.,-1.,0.));
#20431=DIRECTION('center_axis',(0.,1.,0.));
#20432=DIRECTION('ref_axis',(0.,0.,1.));
#20433=DIRECTION('center_axis',(-1.,0.,0.));
#20434=DIRECTION('ref_axis',(0.,0.,-1.));
#20435=DIRECTION('center_axis',(-1.,6.12303176911189E-17,0.));
#20436=DIRECTION('ref_axis',(6.12303176911189E-17,1.,0.));
#20437=DIRECTION('',(1.,0.,0.));
#20438=DIRECTION('center_axis',(1.,-6.12303176911189E-17,0.));
#20439=DIRECTION('ref_axis',(6.12303176911189E-17,1.,0.));
#20440=DIRECTION('',(1.,0.,0.));
#20441=DIRECTION('center_axis',(0.,0.,1.));
#20442=DIRECTION('ref_axis',(0.502661025164392,0.864483599486238,0.));
#20443=DIRECTION('center_axis',(0.,0.,-1.));
#20444=DIRECTION('ref_axis',(1.,0.,0.));
#20445=DIRECTION('center_axis',(8.47625784656822E-14,0.707106781186507,
0.707106781186588));
#20446=DIRECTION('ref_axis',(-2.64990011864105E-13,-0.707106781186588,0.707106781186507));
#20447=DIRECTION('center_axis',(0.,0.707106781186548,0.707106781186548));
#20448=DIRECTION('ref_axis',(0.,0.707106781186548,-0.707106781186548));
#20449=DIRECTION('center_axis',(0.0242120578352017,0.225844330253542,-0.973862472193951));
#20450=DIRECTION('ref_axis',(0.0389083137551034,-0.973622857458564,-0.224821428149));
#20451=DIRECTION('',(0.,-0.707106781186548,-0.707106781186548));
#20452=DIRECTION('center_axis',(1.96528009851118E-14,-1.,-3.48447557928277E-14));
#20453=DIRECTION('ref_axis',(8.37468481768744E-12,3.48447557929923E-14,
-1.));
#20454=DIRECTION('center_axis',(0.,0.,1.));
#20455=DIRECTION('ref_axis',(-1.,0.,0.));
#20456=DIRECTION('center_axis',(0.,0.,1.));
#20457=DIRECTION('ref_axis',(-1.,0.,0.));
#20458=DIRECTION('center_axis',(0.,-0.707106781186553,-0.707106781186542));
#20459=DIRECTION('ref_axis',(-1.91958678679309E-15,0.707106781186542,-0.707106781186553));
#20460=DIRECTION('center_axis',(0.,0.,1.));
#20461=DIRECTION('ref_axis',(-1.,0.,0.));
#20462=DIRECTION('',(0.,0.,1.));
#20463=DIRECTION('center_axis',(0.,0.,1.));
#20464=DIRECTION('ref_axis',(-1.,0.,0.));
#20465=DIRECTION('center_axis',(0.,0.,1.));
#20466=DIRECTION('ref_axis',(-1.,0.,0.));
#20467=DIRECTION('center_axis',(0.,0.,-1.));
#20468=DIRECTION('ref_axis',(1.,0.,0.));
#20469=DIRECTION('',(0.,0.,1.));
#20470=DIRECTION('center_axis',(0.,0.,-1.));
#20471=DIRECTION('ref_axis',(-1.,0.,0.));
#20472=DIRECTION('center_axis',(6.12303176911189E-17,1.,-5.4780741346636E-16));
#20473=DIRECTION('ref_axis',(-9.26409749374061E-33,-5.4780741346636E-16,
-1.));
#20474=DIRECTION('center_axis',(-6.12303176911189E-17,-1.,5.4780741346636E-16));
#20475=DIRECTION('ref_axis',(1.47760280201776E-47,-5.4780741346636E-16,
-1.));
#20476=DIRECTION('',(6.12303176911189E-17,1.,-5.4780741346636E-16));
#20477=DIRECTION('center_axis',(-6.12303176911189E-17,-1.,5.4780741346636E-16));
#20478=DIRECTION('ref_axis',(2.87506473943675E-33,-5.4780741346636E-16,
-1.));
#20479=DIRECTION('center_axis',(0.,1.,0.));
#20480=DIRECTION('ref_axis',(1.,0.,0.));
#20481=DIRECTION('center_axis',(-1.17140016801371E-14,-0.844082777626922,
0.536212891036405));
#20482=DIRECTION('ref_axis',(-7.91994057259303E-30,-0.536212891036405,-0.844082777626922));
#20483=DIRECTION('center_axis',(0.,-0.536212891036385,-0.844082777626935));
#20484=DIRECTION('ref_axis',(0.,-0.844082777626935,0.536212891036385));
#20485=DIRECTION('center_axis',(-0.707106781186563,-0.379159771411482,-0.596856655942757));
#20486=DIRECTION('ref_axis',(-0.645019472682982,9.40542767458206E-16,0.764166133677598));
#20487=DIRECTION('center_axis',(-1.,0.,0.));
#20488=DIRECTION('ref_axis',(0.,0.,-1.));
#20489=DIRECTION('center_axis',(-1.,0.,0.));
#20490=DIRECTION('ref_axis',(0.,0.,-1.));
#20491=DIRECTION('',(1.,0.,0.));
#20492=DIRECTION('center_axis',(-1.,0.,0.));
#20493=DIRECTION('ref_axis',(0.,0.,1.));
#20494=DIRECTION('',(-1.,0.,0.));
#20495=DIRECTION('center_axis',(-0.707106781186547,0.379159771411489,0.596856655942772));
#20496=DIRECTION('ref_axis',(-0.645019472683,-1.15352107484122E-15,-0.764166133677583));
#20497=DIRECTION('center_axis',(-0.707106781186548,0.379159771411488,0.596856655942771));
#20498=DIRECTION('ref_axis',(-0.645019472682999,-1.68179175522602E-15,-0.764166133677584));
#20499=DIRECTION('',(0.707106781186547,-0.379159771411489,-0.596856655942772));
#20500=DIRECTION('center_axis',(-0.707106781186554,0.379159771411484,0.596856655942767));
#20501=DIRECTION('ref_axis',(0.645019472682992,-2.55583619520875E-15,0.76416613367759));
#20502=DIRECTION('',(-0.707106781186547,0.379159771411489,0.596856655942772));
#20503=DIRECTION('center_axis',(0.,1.,0.));
#20504=DIRECTION('ref_axis',(1.,0.,0.));
#20505=DIRECTION('center_axis',(-1.1714001680137E-14,0.84408277762692,-0.536212891036409));
#20506=DIRECTION('ref_axis',(-1.67319991007564E-29,0.536212891036409,0.84408277762692));
#20507=DIRECTION('center_axis',(0.,0.536212891036392,0.844082777626931));
#20508=DIRECTION('ref_axis',(0.,0.844082777626931,-0.536212891036392));
#20509=DIRECTION('center_axis',(1.,0.,0.));
#20510=DIRECTION('ref_axis',(0.,0.,1.));
#20511=DIRECTION('center_axis',(-0.707106781186233,-0.379159771411426,-0.596856655943184));
#20512=DIRECTION('ref_axis',(0.707106781186862,-0.379159771413722,-0.59685665594098));
#20513=DIRECTION('',(-1.,0.,0.));
#20514=DIRECTION('',(1.,0.,0.));
#20515=DIRECTION('center_axis',(0.,1.,0.));
#20516=DIRECTION('ref_axis',(1.,0.,0.));
#20517=DIRECTION('center_axis',(0.,-0.536212891036408,-0.844082777626921));
#20518=DIRECTION('ref_axis',(0.,0.844082777626921,-0.536212891036408));
#20519=DIRECTION('center_axis',(0.,0.844082777626921,-0.536212891036408));
#20520=DIRECTION('ref_axis',(0.,0.536212891036408,0.844082777626921));
#20521=DIRECTION('center_axis',(-1.,6.12303176911189E-17,0.));
#20522=DIRECTION('ref_axis',(-6.12303176911189E-17,-1.,0.));
#20523=DIRECTION('center_axis',(-1.,6.12303176911189E-17,0.));
#20524=DIRECTION('ref_axis',(-6.12303176911189E-17,-1.,0.));
#20525=DIRECTION('',(-1.,6.12303176911189E-17,0.));
#20526=DIRECTION('center_axis',(1.,-6.12303176911189E-17,0.));
#20527=DIRECTION('ref_axis',(-6.12303176911189E-17,-1.,0.));
#20528=DIRECTION('center_axis',(-1.,0.,0.));
#20529=DIRECTION('ref_axis',(0.,0.,-1.));
#20530=DIRECTION('',(1.,0.,0.));
#20531=DIRECTION('center_axis',(1.,0.,0.));
#20532=DIRECTION('ref_axis',(0.,0.,-1.));
#20533=DIRECTION('',(-1.,0.,0.));
#20534=DIRECTION('center_axis',(0.,0.,1.));
#20535=DIRECTION('ref_axis',(-1.,0.,0.));
#20536=DIRECTION('center_axis',(8.67361737988403E-16,0.,-1.));
#20537=DIRECTION('ref_axis',(-1.,0.,-8.67361737988403E-16));
#20538=DIRECTION('',(0.,0.,-1.));
#20539=DIRECTION('',(0.,0.,1.));
#20540=DIRECTION('center_axis',(-1.,6.12303176911189E-17,0.));
#20541=DIRECTION('ref_axis',(6.12303176911189E-17,1.,0.));
#20542=DIRECTION('center_axis',(-1.,6.12303176911189E-17,0.));
#20543=DIRECTION('ref_axis',(-6.12303176911189E-17,-1.,0.));
#20544=DIRECTION('',(-1.,6.12303176911189E-17,0.));
#20545=DIRECTION('center_axis',(-1.,6.12303176911189E-17,0.));
#20546=DIRECTION('ref_axis',(6.12303176911189E-17,1.,0.));
#20547=DIRECTION('',(-1.,6.12303176911189E-17,0.));
#20548=DIRECTION('center_axis',(-1.,6.12303176911189E-17,0.));
#20549=DIRECTION('ref_axis',(-6.12303176911189E-17,-1.,0.));
#20550=DIRECTION('center_axis',(0.,1.,0.));
#20551=DIRECTION('ref_axis',(0.,0.,-1.));
#20552=DIRECTION('',(0.,-1.,0.));
#20553=DIRECTION('center_axis',(0.,-1.,0.));
#20554=DIRECTION('ref_axis',(-1.,0.,0.));
#20555=DIRECTION('',(0.,-1.,0.));
#20556=DIRECTION('center_axis',(0.,1.,0.));
#20557=DIRECTION('ref_axis',(0.,0.,-1.));
#20558=DIRECTION('center_axis',(0.,-1.,0.));
#20559=DIRECTION('ref_axis',(-1.,0.,0.));
#20560=DIRECTION('',(0.,1.,0.));
#20561=DIRECTION('center_axis',(0.,-1.,0.));
#20562=DIRECTION('ref_axis',(0.,0.,-1.));
#20563=DIRECTION('center_axis',(1.,0.,0.));
#20564=DIRECTION('ref_axis',(0.,0.,1.));
#20565=DIRECTION('',(-1.,0.,0.));
#20566=DIRECTION('center_axis',(-1.,6.12303176911189E-17,0.));
#20567=DIRECTION('ref_axis',(-6.12303176911189E-17,-1.,0.));
#20568=DIRECTION('center_axis',(1.,-9.50125619344947E-18,-2.21695977847154E-17));
#20569=DIRECTION('ref_axis',(-2.21695977847154E-17,2.10639028258311E-34,
-1.));
#20570=DIRECTION('center_axis',(1.,-9.50125619344947E-18,-2.21695977847154E-17));
#20571=DIRECTION('ref_axis',(-2.21695977847154E-17,2.10639028258311E-34,
-1.));
#20572=DIRECTION('',(1.,-9.50125619344947E-18,-2.21695977847154E-17));
#20573=DIRECTION('center_axis',(-1.,9.50125619344947E-18,2.21695977847154E-17));
#20574=DIRECTION('ref_axis',(-2.21695977847154E-17,2.10639028258311E-34,
-1.));
#20575=DIRECTION('center_axis',(-6.12303176911189E-17,-1.,5.4780741346636E-16));
#20576=DIRECTION('ref_axis',(0.,-5.80034886334776E-16,-1.));
#20577=DIRECTION('center_axis',(-1.,6.12303176911188E-17,-1.22464679914735E-16));
#20578=DIRECTION('ref_axis',(-1.22464679914735E-16,5.43782705938852E-16,
1.));
#20579=DIRECTION('center_axis',(-6.12303176911189E-17,-1.,5.4780741346636E-16));
#20580=DIRECTION('ref_axis',(-4.87050097983572E-33,-5.4780741346636E-16,
-1.));
#20581=DIRECTION('center_axis',(-6.12303176911189E-17,-1.,5.4780741346636E-16));
#20582=DIRECTION('ref_axis',(3.00804750808099E-33,-5.4780741346636E-16,
-1.));
#20583=DIRECTION('',(-1.00331952890699E-16,-0.936329177569045,0.351123441588391));
#20584=DIRECTION('center_axis',(-6.12303176911189E-17,-1.,5.4780741346636E-16));
#20585=DIRECTION('ref_axis',(3.00804750808099E-33,-5.4780741346636E-16,
-1.));
#20586=DIRECTION('center_axis',(-6.12303176911189E-17,-1.,5.4780741346636E-16));
#20587=DIRECTION('ref_axis',(0.,-5.07530525542929E-16,-1.));
#20588=DIRECTION('center_axis',(1.,-6.12303176911188E-17,1.22464679914735E-16));
#20589=DIRECTION('ref_axis',(-1.22464679914735E-16,5.07530525542929E-16,
1.));
#20590=DIRECTION('center_axis',(0.,1.,0.));
#20591=DIRECTION('ref_axis',(0.,0.,-1.));
#20592=DIRECTION('center_axis',(0.,-1.,0.));
#20593=DIRECTION('ref_axis',(-1.,0.,0.));
#20594=DIRECTION('',(0.,1.,0.));
#20595=DIRECTION('center_axis',(0.,-1.,0.));
#20596=DIRECTION('ref_axis',(0.,0.,-1.));
#20597=DIRECTION('center_axis',(0.,0.707106781186548,0.707106781186548));
#20598=DIRECTION('ref_axis',(0.,0.707106781186548,-0.707106781186548));
#20599=DIRECTION('center_axis',(0.,0.707106781186548,0.707106781186548));
#20600=DIRECTION('ref_axis',(-1.,0.,0.));
#20601=DIRECTION('',(0.,0.707106781186548,0.707106781186548));
#20602=DIRECTION('center_axis',(0.,0.707106781186548,0.707106781186548));
#20603=DIRECTION('ref_axis',(-1.,0.,0.));
#20604=DIRECTION('center_axis',(0.,0.,1.));
#20605=DIRECTION('ref_axis',(1.,0.,0.));
#20606=DIRECTION('center_axis',(0.,0.707106781186548,0.707106781186548));
#20607=DIRECTION('ref_axis',(1.,0.,0.));
#20608=DIRECTION('center_axis',(-1.,9.50125619344947E-18,2.21695977847154E-17));
#20609=DIRECTION('ref_axis',(9.50125619344947E-18,1.,-1.28981852722485E-50));
#20610=DIRECTION('center_axis',(1.,0.,0.));
#20611=DIRECTION('ref_axis',(0.,0.296692407913666,-0.954973096524918));
#20612=DIRECTION('',(-1.,0.,0.));
#20613=DIRECTION('center_axis',(-1.,6.12303176911189E-17,0.));
#20614=DIRECTION('ref_axis',(-6.12303176911189E-17,-1.,0.));
#20615=DIRECTION('center_axis',(1.,0.,0.));
#20616=DIRECTION('ref_axis',(0.,0.,1.));
#20617=DIRECTION('',(1.,0.,0.));
#20618=DIRECTION('center_axis',(-1.,6.12303176911189E-17,0.));
#20619=DIRECTION('ref_axis',(-6.12303176911189E-17,-1.,0.));
#20620=DIRECTION('center_axis',(0.763478425075362,0.,-0.645833333333334));
#20621=DIRECTION('ref_axis',(0.,-1.,0.));
#20622=DIRECTION('',(0.,-1.,0.));
#20623=DIRECTION('',(-0.645833333333334,0.,-0.763478425075362));
#20624=DIRECTION('',(0.645833333333334,0.,0.763478425075362));
#20625=DIRECTION('center_axis',(0.,1.,0.));
#20626=DIRECTION('ref_axis',(0.,0.,-1.));
#20627=DIRECTION('',(0.,-1.,0.));
#20628=DIRECTION('center_axis',(0.,1.,0.));
#20629=DIRECTION('ref_axis',(0.,0.,-1.));
#20630=DIRECTION('center_axis',(0.,-1.,0.));
#20631=DIRECTION('ref_axis',(-1.,0.,0.));
#20632=DIRECTION('center_axis',(0.,-1.,0.));
#20633=DIRECTION('ref_axis',(0.,0.,-1.));
#20634=DIRECTION('center_axis',(0.,-1.,0.));
#20635=DIRECTION('ref_axis',(-1.,0.,0.));
#20636=DIRECTION('',(-0.645833333333333,0.,0.763478425075362));
#20637=DIRECTION('',(0.645833333333334,0.,-0.763478425075362));
#20638=DIRECTION('center_axis',(0.,-1.,0.));
#20639=DIRECTION('ref_axis',(1.,0.,0.));
#20640=DIRECTION('',(-0.645833333333334,0.,-0.763478425075362));
#20641=DIRECTION('center_axis',(0.763478425075362,0.,0.645833333333333));
#20642=DIRECTION('ref_axis',(0.,-1.,0.));
#20643=DIRECTION('',(0.,-1.,0.));
#20644=DIRECTION('',(0.645833333333333,0.,-0.763478425075362));
#20645=DIRECTION('center_axis',(0.,1.,0.));
#20646=DIRECTION('ref_axis',(3.21624529935327E-16,0.,1.));
#20647=DIRECTION('',(0.,-1.,0.));
#20648=DIRECTION('center_axis',(0.,1.,0.));
#20649=DIRECTION('ref_axis',(0.,0.,-1.));
#20650=DIRECTION('center_axis',(-0.763478425075362,0.,0.645833333333334));
#20651=DIRECTION('ref_axis',(0.,1.,0.));
#20652=DIRECTION('',(0.,-1.,0.));
#20653=DIRECTION('',(0.645833333333334,0.,0.763478425075362));
#20654=DIRECTION('center_axis',(0.,1.,0.));
#20655=DIRECTION('ref_axis',(0.,0.,-1.));
#20656=DIRECTION('',(0.,-1.,0.));
#20657=DIRECTION('center_axis',(0.,1.,0.));
#20658=DIRECTION('ref_axis',(0.,0.,-1.));
#20659=DIRECTION('center_axis',(1.,0.,0.));
#20660=DIRECTION('ref_axis',(0.,1.,0.));
#20661=DIRECTION('',(0.,0.939692620785908,-0.342020143325669));
#20662=DIRECTION('center_axis',(0.00295110397743048,-0.889977818593701,
0.45599426903911));
#20663=DIRECTION('ref_axis',(-7.26976717678396E-18,0.455996254682473,0.88998169403396));
#20664=DIRECTION('center_axis',(0.999864261635529,0.,-0.0164759917467061));
#20665=DIRECTION('ref_axis',(0.0164759917467061,0.,0.999864261635529));
#20666=DIRECTION('center_axis',(0.999864261635529,0.,-0.0164759917467083));
#20667=DIRECTION('ref_axis',(-0.0164759917467083,0.,-0.999864261635529));
#20668=DIRECTION('center_axis',(0.999865821664235,1.8733920536864E-13,-0.0163810459893322));
#20669=DIRECTION('ref_axis',(-0.0163810459893322,1.88332865382296E-28,-0.999865821664235));
#20670=DIRECTION('center_axis',(-0.189008920572759,0.,-0.981975370334674));
#20671=DIRECTION('ref_axis',(-0.981975370334674,0.,0.189008920572759));
#20672=DIRECTION('center_axis',(0.,-1.,0.));
#20673=DIRECTION('ref_axis',(0.,0.,-1.));
#20674=DIRECTION('center_axis',(-0.0588235294117643,8.6585981177414E-16,
-0.998268396969244));
#20675=DIRECTION('ref_axis',(-0.998268396969244,-2.36797261535997E-32,0.0588235294117643));
#20676=DIRECTION('center_axis',(0.,-1.,0.));
#20677=DIRECTION('ref_axis',(0.,0.,-1.));
#20678=DIRECTION('center_axis',(0.,1.,0.));
#20679=DIRECTION('ref_axis',(1.,0.,0.));
#20680=DIRECTION('center_axis',(1.,-6.12303176911189E-17,0.));
#20681=DIRECTION('ref_axis',(-6.12303176911189E-17,-1.,0.));
#20682=DIRECTION('center_axis',(0.,-1.,0.));
#20683=DIRECTION('ref_axis',(0.,0.,-1.));
#20684=DIRECTION('center_axis',(0.645833333333334,0.,0.763478425075362));
#20685=DIRECTION('ref_axis',(-0.763478425075362,0.,0.645833333333334));
#20686=DIRECTION('center_axis',(0.645833333333334,0.,-0.763478425075362));
#20687=DIRECTION('ref_axis',(-0.763478425075362,0.,-0.645833333333334));
#20688=DIRECTION('center_axis',(0.,-1.,0.));
#20689=DIRECTION('ref_axis',(0.,0.,-1.));
#20690=DIRECTION('center_axis',(0.,1.,0.));
#20691=DIRECTION('ref_axis',(1.,0.,0.));
#20692=DIRECTION('center_axis',(-1.,-7.44144872161806E-15,-1.1714001680137E-14));
#20693=DIRECTION('ref_axis',(-1.1714001680137E-14,1.61017035136602E-29,
1.));
#20694=DIRECTION('center_axis',(2.91984586184824E-15,-0.844082777626921,
0.536212891036408));
#20695=DIRECTION('ref_axis',(1.11963091130469E-29,-0.536212891036408,-0.844082777626921));
#20696=DIRECTION('center_axis',(-0.707106781186551,-0.379159771411502,-0.596856655942759));
#20697=DIRECTION('ref_axis',(0.645019472682989,9.66631051215658E-16,-0.764166133677592));
#20698=DIRECTION('center_axis',(-1.,0.,0.));
#20699=DIRECTION('ref_axis',(0.,-0.21769688453124,0.976016427354269));
#20700=DIRECTION('',(1.,0.,0.));
#20701=DIRECTION('',(-1.,0.,0.));
#20702=DIRECTION('center_axis',(-1.06260198549818E-16,-0.844082777626919,
0.53621289103641));
#20703=DIRECTION('ref_axis',(3.01348942600866E-31,0.53621289103641,0.844082777626919));
#20704=DIRECTION('center_axis',(-3.74339213057462E-16,-0.844082777626916,
0.536212891036415));
#20705=DIRECTION('ref_axis',(-1.14237476972092E-30,0.536212891036415,0.844082777626916));
#20706=DIRECTION('',(7.1769990995421E-17,0.844082777626919,-0.53621289103641));
#20707=DIRECTION('',(-1.06260198549818E-16,-0.844082777626919,0.53621289103641));
#20708=DIRECTION('center_axis',(0.,1.,0.));
#20709=DIRECTION('ref_axis',(1.,0.,0.));
#20710=DIRECTION('center_axis',(0.,0.,-1.));
#20711=DIRECTION('ref_axis',(-1.,0.,0.));
#20712=DIRECTION('center_axis',(-1.,0.,0.));
#20713=DIRECTION('ref_axis',(0.,0.,1.));
#20714=DIRECTION('center_axis',(0.,-1.,0.));
#20715=DIRECTION('ref_axis',(0.,0.,1.));
#20716=DIRECTION('center_axis',(0.,0.,-1.));
#20717=DIRECTION('ref_axis',(1.,0.,0.));
#20718=DIRECTION('center_axis',(0.,0.,-1.));
#20719=DIRECTION('ref_axis',(1.,0.,0.));
#20720=DIRECTION('',(0.,0.,1.));
#20721=DIRECTION('',(0.,0.,-1.));
#20722=DIRECTION('center_axis',(-1.,0.,0.));
#20723=DIRECTION('ref_axis',(0.,0.,-1.));
#20724=DIRECTION('center_axis',(0.763478425075353,-1.69136608464776E-14,
0.645833333333344));
#20725=DIRECTION('ref_axis',(0.645833333333344,-3.74756545942938E-12,-0.763478425075353));
#20726=DIRECTION('',(1.,0.,0.));
#20727=DIRECTION('',(-1.,0.,0.));
#20728=DIRECTION('center_axis',(0.,1.,0.));
#20729=DIRECTION('ref_axis',(1.,0.,0.));
#20730=DIRECTION('center_axis',(0.,1.,0.));
#20731=DIRECTION('ref_axis',(0.,0.,1.));
#20732=DIRECTION('center_axis',(-1.,0.,0.));
#20733=DIRECTION('ref_axis',(0.,0.,1.));
#20734=DIRECTION('center_axis',(6.12303176911189E-17,1.,0.));
#20735=DIRECTION('ref_axis',(1.,-6.12303176911189E-17,0.));
#20736=DIRECTION('center_axis',(0.,1.,0.));
#20737=DIRECTION('ref_axis',(0.,0.,-1.));
#20738=DIRECTION('',(-6.12303176911189E-17,-1.,0.));
#20739=DIRECTION('',(6.12303176911189E-17,1.,0.));
#20740=DIRECTION('center_axis',(-1.,0.,0.));
#20741=DIRECTION('ref_axis',(0.,0.,-1.));
#20742=DIRECTION('center_axis',(0.763478425075345,1.20977462004704E-13,
0.645833333333353));
#20743=DIRECTION('ref_axis',(0.645833333333353,2.41075408440725E-12,-0.763478425075345));
#20744=DIRECTION('',(1.,0.,0.));
#20745=DIRECTION('',(-1.,0.,0.));
#20746=DIRECTION('center_axis',(0.,1.,0.));
#20747=DIRECTION('ref_axis',(1.,0.,0.));
#20748=DIRECTION('center_axis',(0.,-1.38777878078144E-14,1.));
#20749=DIRECTION('ref_axis',(0.,-1.,-1.38777878078144E-14));
#20750=DIRECTION('center_axis',(-1.,0.,0.));
#20751=DIRECTION('ref_axis',(0.,0.,1.));
#20752=DIRECTION('center_axis',(-8.49741356322415E-31,-1.38777878078145E-14,
1.));
#20753=DIRECTION('ref_axis',(-4.72949161117447E-59,1.,1.38777878078145E-14));
#20754=DIRECTION('center_axis',(1.2440942836624E-13,0.844082777626929,-0.536212891036395));
#20755=DIRECTION('ref_axis',(-6.70739907751221E-13,0.536212891036395,0.844082777626929));
#20756=DIRECTION('',(8.49741356322415E-31,1.38777878078145E-14,-1.));
#20757=DIRECTION('',(-8.49741356322415E-31,-1.38777878078145E-14,1.));
#20758=DIRECTION('center_axis',(3.28324856682327E-17,0.53621289103641,0.844082777626919));
#20759=DIRECTION('ref_axis',(-9.30104503460367E-32,0.844082777626919,-0.53621289103641));
#20760=DIRECTION('',(-3.28324856682327E-17,-0.53621289103641,-0.844082777626919));
#20761=DIRECTION('center_axis',(1.05472713558318E-13,-0.876416821790961,
-0.481553272735044));
#20762=DIRECTION('ref_axis',(-1.50588472234195E-12,0.481553272735044,-0.876416821790961));
#20763=DIRECTION('',(3.28324856682327E-17,0.53621289103641,0.844082777626919));
#20764=DIRECTION('center_axis',(0.,0.,1.));
#20765=DIRECTION('ref_axis',(1.,0.,0.));
#20766=DIRECTION('center_axis',(0.,0.844082777626921,-0.536212891036408));
#20767=DIRECTION('ref_axis',(0.,-0.536212891036408,-0.844082777626921));
#20768=DIRECTION('center_axis',(0.,-0.536212891036408,-0.844082777626921));
#20769=DIRECTION('ref_axis',(0.,0.844082777626921,-0.536212891036408));
#20770=DIRECTION('center_axis',(-1.,0.,0.));
#20771=DIRECTION('ref_axis',(0.,0.,-1.));
#20772=DIRECTION('center_axis',(5.16834566316983E-17,0.844082777626919,
-0.536212891036411));
#20773=DIRECTION('ref_axis',(-1.89077532649189E-31,-0.536212891036411,-0.844082777626919));
#20774=DIRECTION('',(-5.16834566316983E-17,-0.844082777626919,0.536212891036411));
#20775=DIRECTION('',(5.16834566316983E-17,0.844082777626919,-0.536212891036411));
#20776=DIRECTION('center_axis',(7.85046229341887E-17,0.844082777626919,
-0.536212891036411));
#20777=DIRECTION('ref_axis',(-2.87429797914763E-31,-0.536212891036411,-0.844082777626919));
#20778=DIRECTION('center_axis',(5.54022035325046E-15,0.84408277762691,-0.536212891036424));
#20779=DIRECTION('ref_axis',(-1.55850943745324E-30,-0.536212891036424,-0.84408277762691));
#20780=DIRECTION('',(-5.55111512312579E-17,-0.844082777626919,0.536212891036411));
#20781=DIRECTION('center_axis',(-3.06958154707117E-15,0.844082777626921,
-0.536212891036408));
#20782=DIRECTION('ref_axis',(-1.81691724756689E-31,0.536212891036408,0.844082777626921));
#20783=DIRECTION('',(7.85046229341887E-17,0.844082777626919,-0.536212891036411));
#20784=DIRECTION('center_axis',(0.,0.,1.));
#20785=DIRECTION('ref_axis',(1.,0.,0.));
#20786=DIRECTION('center_axis',(-1.,2.34280033602742E-14,-1.48828974432361E-14));
#20787=DIRECTION('ref_axis',(-2.34280033602742E-14,-1.,6.44068140546378E-29));
#20788=DIRECTION('center_axis',(-0.707106781186557,0.379159771411482,0.596856655942765));
#20789=DIRECTION('ref_axis',(-0.645019472682989,1.25388061323787E-15,-0.764166133677592));
#20790=DIRECTION('center_axis',(-1.,0.,0.));
#20791=DIRECTION('ref_axis',(0.,0.,-1.));
#20792=DIRECTION('',(1.,0.,0.));
#20793=DIRECTION('',(-1.,0.,0.));
#20794=DIRECTION('center_axis',(0.707106781186547,-0.379159771411489,-0.596856655942772));
#20795=DIRECTION('ref_axis',(0.645019472683,1.15352107484122E-15,0.764166133677583));
#20796=DIRECTION('',(0.707106781186547,-0.379159771411489,-0.596856655942772));
#20797=DIRECTION('center_axis',(-0.707106781186551,0.37915977141147,0.596856655942779));
#20798=DIRECTION('ref_axis',(0.645019472683002,9.5350569374018E-17,0.764166133677581));
#20799=DIRECTION('',(-0.707106781186547,0.379159771411489,0.596856655942772));
#20800=DIRECTION('center_axis',(5.16834566316983E-17,0.844082777626919,
-0.536212891036411));
#20801=DIRECTION('ref_axis',(-7.00354623150013E-33,-0.536212891036411,-0.844082777626919));
#20802=DIRECTION('center_axis',(0.,0.844082777626919,-0.53621289103641));
#20803=DIRECTION('ref_axis',(0.,-0.53621289103641,-0.844082777626919));
#20804=DIRECTION('',(-5.16834566316983E-17,-0.844082777626919,0.536212891036411));
#20805=DIRECTION('',(2.77555756156288E-17,0.844082777626919,-0.536212891036411));
#20806=DIRECTION('center_axis',(0.,1.,0.));
#20807=DIRECTION('ref_axis',(-0.9069232251638,0.,0.42129593358884));
#20808=DIRECTION('center_axis',(-1.32984495616866E-14,-0.536212891036413,
-0.844082777626917));
#20809=DIRECTION('ref_axis',(-6.77246941118238E-30,0.844082777626917,-0.536212891036413));
#20810=DIRECTION('center_axis',(3.28324856682327E-17,0.53621289103641,0.844082777626919));
#20811=DIRECTION('ref_axis',(1.02431542274941E-31,0.844082777626919,-0.53621289103641));
#20812=DIRECTION('',(3.28324856682327E-17,0.53621289103641,0.844082777626919));
#20813=DIRECTION('',(-3.28324856682327E-17,-0.53621289103641,-0.844082777626919));
#20814=DIRECTION('center_axis',(-3.28324856682327E-17,-0.53621289103641,
-0.844082777626919));
#20815=DIRECTION('ref_axis',(9.30104503460367E-32,-0.844082777626919,0.53621289103641));
#20816=DIRECTION('',(-3.28324856682327E-17,-0.53621289103641,-0.844082777626919));
#20817=DIRECTION('center_axis',(-1.2947686397577E-14,-0.279210693180882,
-0.960229862487858));
#20818=DIRECTION('ref_axis',(-1.21180702059432E-11,0.960229862487858,-0.279210693180882));
#20819=DIRECTION('',(3.28324856682327E-17,0.53621289103641,0.844082777626919));
#20820=DIRECTION('center_axis',(0.,1.,0.));
#20821=DIRECTION('ref_axis',(1.,0.,0.));
#20822=DIRECTION('center_axis',(-3.28324856682327E-17,-0.53621289103641,
-0.844082777626919));
#20823=DIRECTION('ref_axis',(-1.02431542274941E-31,-0.844082777626919,0.53621289103641));
#20824=DIRECTION('',(-3.28324856682327E-17,-0.53621289103641,-0.844082777626919));
#20825=DIRECTION('center_axis',(-5.85700084006849E-15,0.536212891036413,
0.844082777626917));
#20826=DIRECTION('ref_axis',(-2.92088988510645E-30,-0.844082777626917,0.536212891036413));
#20827=DIRECTION('',(3.28324856682327E-17,0.53621289103641,0.844082777626919));
#20828=DIRECTION('center_axis',(0.,1.,0.));
#20829=DIRECTION('ref_axis',(-0.906923225163802,0.,-0.421295933588834));
#20830=DIRECTION('center_axis',(-0.707106781186551,-0.379159771411477,-0.596856655942775));
#20831=DIRECTION('ref_axis',(-0.645019472682999,-2.94711224947621E-16,0.764166133677583));
#20832=DIRECTION('center_axis',(0.,-0.844082777626922,0.536212891036405));
#20833=DIRECTION('ref_axis',(0.,0.536212891036405,0.844082777626922));
#20834=DIRECTION('center_axis',(0.707106781186547,0.379159771411489,0.596856655942772));
#20835=DIRECTION('ref_axis',(-0.645019472683,1.15352107484122E-15,0.764166133677583));
#20836=DIRECTION('center_axis',(-0.707106781186541,-0.379159771411494,-0.596856655942776));
#20837=DIRECTION('ref_axis',(0.645019472683004,1.45000042130455E-15,-0.764166133677579));
#20838=DIRECTION('',(0.707106781186547,0.379159771411489,0.596856655942772));
#20839=DIRECTION('',(-0.707106781186547,-0.379159771411489,-0.596856655942772));
#20840=DIRECTION('center_axis',(-0.707106781186547,-0.379159771411489,-0.596856655942772));
#20841=DIRECTION('ref_axis',(-0.499999999999993,-0.32875021042458,0.801201160224947));
#20842=DIRECTION('',(0.707106781186547,0.379159771411489,0.596856655942772));
#20843=DIRECTION('',(-0.707106781186546,-0.37915977141149,-0.596856655942772));
#20844=DIRECTION('center_axis',(-5.16834566316983E-17,-0.844082777626919,
0.53621289103641));
#20845=DIRECTION('ref_axis',(4.60389737147646E-33,0.53621289103641,0.844082777626919));
#20846=DIRECTION('',(5.16834566316983E-17,0.844082777626919,-0.53621289103641));
#20847=DIRECTION('',(-5.55111512312577E-17,-0.844082777626919,0.53621289103641));
#20848=DIRECTION('center_axis',(3.28324856682327E-17,0.53621289103641,0.844082777626919));
#20849=DIRECTION('ref_axis',(1.02431542274941E-31,0.844082777626919,-0.53621289103641));
#20850=DIRECTION('',(3.28324856682327E-17,0.53621289103641,0.844082777626919));
#20851=DIRECTION('center_axis',(0.707106781186648,-0.379159771411277,-0.596856655942787));
#20852=DIRECTION('ref_axis',(0.707106781186447,0.379159771409511,0.596856655944146));
#20853=DIRECTION('',(-3.28324856682327E-17,-0.53621289103641,-0.844082777626919));
#20854=DIRECTION('center_axis',(0.,-1.,0.));
#20855=DIRECTION('ref_axis',(0.,0.,-1.));
#20856=DIRECTION('',(-0.645833333333334,0.,0.763478425075362));
#20857=DIRECTION('center_axis',(-1.,6.12303176911189E-17,0.));
#20858=DIRECTION('ref_axis',(0.,0.,1.));
#20859=DIRECTION('',(-5.16834566316983E-17,-0.844082777626919,0.53621289103641));
#20860=DIRECTION('',(3.28324856682327E-17,0.53621289103641,0.844082777626919));
#20861=DIRECTION('',(-6.12303176911189E-17,-1.,0.));
#20862=DIRECTION('',(3.28324856682327E-17,0.53621289103641,0.844082777626919));
#20863=DIRECTION('center_axis',(-1.,6.12303176911189E-17,0.));
#20864=DIRECTION('ref_axis',(-6.12303176911189E-17,-1.,0.));
#20865=DIRECTION('center_axis',(0.,1.,1.38777878078145E-14));
#20866=DIRECTION('ref_axis',(0.,1.38777878078145E-14,-1.));
#20867=DIRECTION('',(-8.49741356322415E-31,-1.38777878078145E-14,1.));
#20868=DIRECTION('',(-1.,0.,0.));
#20869=DIRECTION('',(1.,0.,0.));
#20870=DIRECTION('center_axis',(0.,0.,-1.));
#20871=DIRECTION('ref_axis',(0.,-1.,0.));
#20872=DIRECTION('',(6.12303176911189E-17,1.,0.));
#20873=DIRECTION('center_axis',(0.,0.,1.));
#20874=DIRECTION('ref_axis',(-1.,0.,0.));
#20875=DIRECTION('',(1.,0.,0.));
#20876=DIRECTION('center_axis',(4.09272608780354E-15,5.36063096661746E-15,
-1.));
#20877=DIRECTION('ref_axis',(1.,8.41575319003231E-13,4.09272608780805E-15));
#20878=DIRECTION('',(0.,-1.,0.));
#20879=DIRECTION('',(1.,0.,0.));
#20880=DIRECTION('center_axis',(0.,0.393919298579167,0.919145030018058));
#20881=DIRECTION('ref_axis',(1.,0.,0.));
#20882=DIRECTION('center_axis',(-2.8065169850844E-7,0.393919438749702,0.919144969944916));
#20883=DIRECTION('ref_axis',(-0.918388540903831,0.36368697754103,-0.155866193587968));
#20884=DIRECTION('center_axis',(-2.74470711777249E-6,0.393918529530603,
0.919145359605821));
#20885=DIRECTION('ref_axis',(0.773783494589027,0.582233610477103,-0.249525802939077));
#20886=DIRECTION('',(1.,0.,0.));
#20887=DIRECTION('',(5.62795421922187E-17,0.919145030018058,-0.393919298579167));
#20888=DIRECTION('center_axis',(0.,0.707106781186548,0.707106781186548));
#20889=DIRECTION('ref_axis',(-0.0433996118379072,-0.706440540205727,0.706440540205727));
#20890=DIRECTION('center_axis',(0.,0.707106781186548,0.707106781186548));
#20891=DIRECTION('ref_axis',(1.,0.,0.));
#20892=DIRECTION('center_axis',(1.,-6.12303176911189E-17,0.));
#20893=DIRECTION('ref_axis',(-6.12303176911189E-17,-1.,0.));
#20894=DIRECTION('',(0.,0.,1.));
#20895=DIRECTION('',(0.,1.,0.));
#20896=DIRECTION('',(0.,0.,1.));
#20897=DIRECTION('center_axis',(0.,0.,-1.));
#20898=DIRECTION('ref_axis',(0.,-1.,0.));
#20899=DIRECTION('',(1.,0.,0.));
#20900=DIRECTION('',(1.,0.,0.));
#20901=DIRECTION('center_axis',(-1.63807337386231E-14,2.73218531703445E-14,
1.));
#20902=DIRECTION('ref_axis',(-6.24102255372086E-12,-1.,2.73218531702423E-14));
#20903=DIRECTION('center_axis',(0.,0.,1.));
#20904=DIRECTION('ref_axis',(-1.,0.,0.));
#20905=DIRECTION('center_axis',(5.57758659674859E-13,0.707106781185667,
0.707106781187428));
#20906=DIRECTION('ref_axis',(1.7011908926004E-10,-0.707106781187428,0.707106781185667));
#20907=DIRECTION('center_axis',(0.,0.707106781186548,0.707106781186548));
#20908=DIRECTION('ref_axis',(1.,0.,0.));
#20909=DIRECTION('center_axis',(0.,0.707106781186548,0.707106781186548));
#20910=DIRECTION('ref_axis',(1.,0.,0.));
#20911=DIRECTION('center_axis',(1.,-6.12303176911189E-17,0.));
#20912=DIRECTION('ref_axis',(0.,-1.,-3.82599934640054E-15));
#20913=DIRECTION('center_axis',(-5.76857827429812E-17,-0.942111439531993,
0.335299918733896));
#20914=DIRECTION('ref_axis',(-2.18993762695094E-31,0.335299918733896,0.942111439531992));
#20915=DIRECTION('center_axis',(1.,-6.12303176911189E-17,0.));
#20916=DIRECTION('ref_axis',(6.12303176911189E-17,1.,0.));
#20917=DIRECTION('center_axis',(0.,0.942111439531991,0.335299918733899));
#20918=DIRECTION('ref_axis',(0.,-0.335299918733899,0.942111439531991));
#20919=DIRECTION('center_axis',(0.,-0.393919298579169,-0.919145030018057));
#20920=DIRECTION('ref_axis',(0.,-0.919145030018057,0.393919298579169));
#20921=DIRECTION('center_axis',(-4.29577406892133E-7,-0.393919484948488,
-0.919144950145369));
#20922=DIRECTION('ref_axis',(0.716472147339189,-0.641210067193636,0.274804133550978));
#20923=DIRECTION('',(-5.62795421922186E-17,-0.919145030018057,0.393919298579169));
#20924=DIRECTION('center_axis',(0.,1.,0.));
#20925=DIRECTION('ref_axis',(-0.733899982512709,0.,-0.679257547376432));
#20926=DIRECTION('center_axis',(-1.,6.12303176911189E-17,0.));
#20927=DIRECTION('ref_axis',(0.,0.,1.));
#20928=DIRECTION('center_axis',(-1.,6.12303176911189E-17,0.));
#20929=DIRECTION('ref_axis',(0.,0.,1.));
#20930=DIRECTION('center_axis',(-1.,6.12303176911189E-17,0.));
#20931=DIRECTION('ref_axis',(-6.12303176911189E-17,-1.,0.));
#20932=DIRECTION('center_axis',(-1.,6.12303176911189E-17,0.));
#20933=DIRECTION('ref_axis',(0.,0.976016427354256,0.217696884531301));
#20934=DIRECTION('center_axis',(0.,-0.536212891036408,-0.844082777626921));
#20935=DIRECTION('ref_axis',(0.,0.844082777626921,-0.536212891036408));
#20936=DIRECTION('center_axis',(-1.,6.12303176911189E-17,0.));
#20937=DIRECTION('ref_axis',(-6.12303176911189E-17,-1.,0.));
#20938=DIRECTION('center_axis',(0.,0.844082777626921,-0.536212891036408));
#20939=DIRECTION('ref_axis',(0.,-0.536212891036408,-0.844082777626921));
#20940=DIRECTION('center_axis',(-1.,0.,0.));
#20941=DIRECTION('ref_axis',(0.,0.,-1.));
#20942=DIRECTION('',(1.,0.,0.));
#20943=DIRECTION('center_axis',(-1.,0.,0.));
#20944=DIRECTION('ref_axis',(0.,0.,1.));
#20945=DIRECTION('',(-1.,0.,0.));
#20946=DIRECTION('center_axis',(-5.16834566316983E-17,-0.844082777626919,
0.53621289103641));
#20947=DIRECTION('ref_axis',(1.42644336347277E-31,0.53621289103641,0.844082777626919));
#20948=DIRECTION('',(5.16834566316983E-17,0.844082777626919,-0.53621289103641));
#20949=DIRECTION('center_axis',(0.,0.,1.));
#20950=DIRECTION('ref_axis',(1.,0.,0.));
#20951=DIRECTION('center_axis',(6.35380838599017E-16,-0.53621289103641,
-0.844082777626919));
#20952=DIRECTION('ref_axis',(-2.25177327489712E-32,-0.844082777626919,0.53621289103641));
#20953=DIRECTION('',(-1.,-3.40699396374318E-16,-5.3631402309558E-16));
#20954=DIRECTION('',(0.,0.844082777626919,-0.53621289103641));
#20955=DIRECTION('center_axis',(-0.707106781186548,0.379159771411488,0.596856655942771));
#20956=DIRECTION('ref_axis',(0.472562808991505,0.881296993957235,-5.26365224320196E-17));
#20957=DIRECTION('center_axis',(-3.28324856682327E-17,-0.53621289103641,
-0.844082777626919));
#20958=DIRECTION('ref_axis',(-1.02431542274941E-31,-0.844082777626919,0.53621289103641));
#20959=DIRECTION('',(-3.28324856682327E-17,-0.53621289103641,-0.844082777626919));
#20960=DIRECTION('center_axis',(0.707106781186624,0.37915977141133,0.596856655942782));
#20961=DIRECTION('ref_axis',(0.707106781186471,-0.379159771411251,-0.596856655943013));
#20962=DIRECTION('',(3.28324856682327E-17,0.53621289103641,0.844082777626919));
#20963=DIRECTION('center_axis',(1.,0.,0.));
#20964=DIRECTION('ref_axis',(0.,0.,1.));
#20965=DIRECTION('',(-1.,0.,0.));
#20966=DIRECTION('',(1.,0.,0.));
#20967=DIRECTION('center_axis',(1.,-6.12303176911189E-17,0.));
#20968=DIRECTION('ref_axis',(-6.12303176911189E-17,-1.,0.));
#20969=DIRECTION('center_axis',(0.,0.707106781186548,0.707106781186548));
#20970=DIRECTION('ref_axis',(0.,0.707106781186548,-0.707106781186548));
#20971=DIRECTION('center_axis',(0.,0.,1.));
#20972=DIRECTION('ref_axis',(1.,1.22464679914735E-16,0.));
#20973=DIRECTION('',(0.,0.,1.));
#20974=DIRECTION('',(0.,0.,1.));
#20975=DIRECTION('center_axis',(1.,0.,0.));
#20976=DIRECTION('ref_axis',(0.,0.,1.));
#20977=DIRECTION('center_axis',(-1.07888181684715E-8,1.,-7.76704436521076E-9));
#20978=DIRECTION('ref_axis',(0.988419917866598,9.48528488113968E-9,-0.151743421487022));
#20979=DIRECTION('center_axis',(-4.24666173856902E-7,-0.999999999999844,
3.63117712421864E-7));
#20980=DIRECTION('ref_axis',(0.988473455373134,-4.74745184886749E-7,-0.151394280019001));
#20981=DIRECTION('center_axis',(-0.641555200491106,0.,0.76707687015241));
#20982=DIRECTION('ref_axis',(0.,1.,0.));
#20983=DIRECTION('',(0.76707687015241,0.,0.641555200491106));
#20984=DIRECTION('',(0.76707687015241,0.,0.641555200491106));
#20985=DIRECTION('center_axis',(0.,-1.,0.));
#20986=DIRECTION('ref_axis',(0.,0.,-1.));
#20987=DIRECTION('center_axis',(-6.12303176911189E-17,-1.,0.));
#20988=DIRECTION('ref_axis',(-1.,6.12303176911189E-17,0.));
#20989=DIRECTION('',(6.12303176911189E-17,1.,0.));
#20990=DIRECTION('center_axis',(-9.15914568528454E-14,-0.618483918322797,
0.785797456585397));
#20991=DIRECTION('ref_axis',(6.57167920551881E-13,-0.785797456585397,-0.618483918322797));
#20992=DIRECTION('center_axis',(3.28324856682327E-17,0.53621289103641,0.844082777626919));
#20993=DIRECTION('ref_axis',(-9.30104503460367E-32,0.844082777626919,-0.53621289103641));
#20994=DIRECTION('center_axis',(0.,-0.536212891036408,-0.844082777626921));
#20995=DIRECTION('ref_axis',(0.,0.844082777626921,-0.536212891036408));
#20996=DIRECTION('',(-3.28324856682327E-17,-0.53621289103641,-0.844082777626919));
#20997=DIRECTION('center_axis',(-3.63890463093118E-14,-0.844082777626962,
0.536212891036343));
#20998=DIRECTION('ref_axis',(-1.84413742032711E-5,-0.536212890945164,-0.844082777483432));
#20999=DIRECTION('center_axis',(0.,0.844082777626919,-0.53621289103641));
#21000=DIRECTION('ref_axis',(-1.,0.,0.));
#21001=DIRECTION('',(1.,3.40699396374318E-16,5.3631402309558E-16));
#21002=DIRECTION('',(1.,0.,0.));
#21003=DIRECTION('',(-3.28324856682327E-17,-0.53621289103641,-0.844082777626919));
#21004=DIRECTION('center_axis',(0.,-1.,0.));
#21005=DIRECTION('ref_axis',(0.,0.,-1.));
#21006=DIRECTION('',(-0.645833333333334,0.,-0.763478425075362));
#21007=DIRECTION('',(0.645833333333334,0.,-0.763478425075362));
#21008=DIRECTION('',(0.,0.,1.));
#21009=DIRECTION('center_axis',(0.,-1.,0.));
#21010=DIRECTION('ref_axis',(0.,0.,-1.));
#21011=DIRECTION('',(0.,0.,-1.));
#21012=DIRECTION('',(0.645833333333334,0.,-0.763478425075362));
#21013=DIRECTION('',(0.645833333333334,0.,0.763478425075362));
#21014=DIRECTION('center_axis',(0.,-1.,0.));
#21015=DIRECTION('ref_axis',(0.,0.,-1.));
#21016=DIRECTION('',(-0.645833333333333,0.,0.763478425075362));
#21017=DIRECTION('center_axis',(0.,-1.,0.));
#21018=DIRECTION('ref_axis',(0.,0.,-1.));
#21019=DIRECTION('center_axis',(0.,0.536212891036411,0.844082777626919));
#21020=DIRECTION('ref_axis',(1.,0.,0.));
#21021=DIRECTION('center_axis',(-0.707106781186548,-0.379159771411489,-0.596856655942771));
#21022=DIRECTION('ref_axis',(-0.645019472682998,-1.54058679206033E-17,0.764166133677584));
#21023=DIRECTION('center_axis',(-1.,6.12303176911189E-17,3.08148791101958E-33));
#21024=DIRECTION('ref_axis',(3.08148791101958E-33,0.,1.));
#21025=DIRECTION('',(-6.12303176911189E-17,-1.,1.88680483753071E-49));
#21026=DIRECTION('',(1.9280126729044E-32,3.65204942310907E-16,-1.));
#21027=DIRECTION('',(6.12303176911189E-17,1.,0.));
#21028=DIRECTION('center_axis',(-1.,-4.06251537009573E-12,-1.06264377235447E-13));
#21029=DIRECTION('ref_axis',(4.06239277484557E-12,-0.999999999824389,1.87409114472015E-5));
#21030=DIRECTION('center_axis',(-1.,6.12303176911189E-17,3.08148791101958E-33));
#21031=DIRECTION('ref_axis',(3.08148791101958E-33,0.,1.));
#21032=DIRECTION('center_axis',(-1.,6.12303176911189E-17,3.08148791101958E-33));
#21033=DIRECTION('ref_axis',(3.08148791101958E-33,0.,1.));
#21034=DIRECTION('',(0.,0.844082777626919,-0.53621289103641));
#21035=DIRECTION('center_axis',(0.,-1.,0.));
#21036=DIRECTION('ref_axis',(0.,0.,-1.));
#21037=DIRECTION('center_axis',(0.,-0.53621289103641,-0.844082777626919));
#21038=DIRECTION('ref_axis',(0.,-0.844082777626919,0.53621289103641));
#21039=DIRECTION('center_axis',(0.,1.,3.65204942310907E-16));
#21040=DIRECTION('ref_axis',(0.,3.65204942310907E-16,-1.));
#21041=DIRECTION('',(-1.9280126729044E-32,-3.65204942310907E-16,1.));
#21042=DIRECTION('center_axis',(0.,1.,3.65204942310907E-16));
#21043=DIRECTION('ref_axis',(0.,-3.65204942310907E-16,1.));
#21044=DIRECTION('',(-2.23616146400636E-32,-3.65204942310907E-16,1.));
#21045=DIRECTION('center_axis',(0.,0.53621289103641,0.844082777626919));
#21046=DIRECTION('ref_axis',(1.,0.,0.));
#21047=DIRECTION('center_axis',(-0.763478425075362,0.,-0.645833333333334));
#21048=DIRECTION('ref_axis',(-0.645833333333334,0.,0.763478425075362));
#21049=DIRECTION('',(-0.645833333333334,0.,0.763478425075362));
#21050=DIRECTION('',(-0.645833333333334,0.,0.763478425075362));
#21051=DIRECTION('',(0.,1.,0.));
#21052=DIRECTION('center_axis',(1.,-6.12303176911189E-17,0.));
#21053=DIRECTION('ref_axis',(-6.12303176911189E-17,-1.,0.));
#21054=DIRECTION('',(6.12303176911189E-17,1.,0.));
#21055=DIRECTION('',(0.,0.,-1.));
#21056=DIRECTION('center_axis',(1.,-6.12303176911189E-17,0.));
#21057=DIRECTION('ref_axis',(6.12303176911189E-17,1.,0.));
#21058=DIRECTION('center_axis',(0.,1.,0.));
#21059=DIRECTION('ref_axis',(1.,0.,0.));
#21060=DIRECTION('center_axis',(6.93889390390724E-15,0.,-1.));
#21061=DIRECTION('ref_axis',(-1.,0.,-6.93889390390724E-15));
#21062=DIRECTION('center_axis',(0.,1.,0.));
#21063=DIRECTION('ref_axis',(0.,0.,-1.));
#21064=DIRECTION('center_axis',(0.,1.,0.));
#21065=DIRECTION('ref_axis',(0.,0.,-1.));
#21066=DIRECTION('center_axis',(0.,1.,3.65204942310907E-16));
#21067=DIRECTION('ref_axis',(0.,-3.84077154464919E-16,1.));
#21068=DIRECTION('center_axis',(-0.928461531958395,0.,0.371428571428572));
#21069=DIRECTION('ref_axis',(0.371428571428572,0.,0.928461531958395));
#21070=DIRECTION('center_axis',(1.9280126729044E-32,3.65204942310907E-16,
-1.));
#21071=DIRECTION('ref_axis',(7.04119756982749E-48,-1.,-3.65204942310907E-16));
#21072=DIRECTION('center_axis',(0.,1.,0.));
#21073=DIRECTION('ref_axis',(-0.597614304667194,0.,0.801783725737275));
#21074=DIRECTION('center_axis',(0.,1.,0.));
#21075=DIRECTION('ref_axis',(0.,0.,1.));
#21076=DIRECTION('center_axis',(-1.,0.,0.));
#21077=DIRECTION('ref_axis',(0.,0.,-1.));
#21078=DIRECTION('center_axis',(-1.,-3.40699396374318E-16,-5.3631402309558E-16));
#21079=DIRECTION('ref_axis',(5.3631402309558E-16,1.82721863935746E-31,-1.));
#21080=DIRECTION('center_axis',(0.,0.,1.));
#21081=DIRECTION('ref_axis',(-1.,0.,0.));
#21082=DIRECTION('center_axis',(6.12303176911189E-17,1.,0.));
#21083=DIRECTION('ref_axis',(1.,-6.12303176911189E-17,0.));
#21084=DIRECTION('',(-6.12303176911189E-17,-1.,0.));
#21085=DIRECTION('center_axis',(-0.645833333333334,0.,0.763478425075362));
#21086=DIRECTION('ref_axis',(-0.763478425075362,0.,-0.645833333333334));
#21087=DIRECTION('center_axis',(-0.645833333333334,0.,0.763478425075362));
#21088=DIRECTION('ref_axis',(-0.763478425075362,0.,-0.645833333333334));
#21089=DIRECTION('center_axis',(5.8100520420011E-14,2.63746680760317E-14,
1.));
#21090=DIRECTION('ref_axis',(1.,1.73652799098504E-12,-5.81005204200568E-14));
#21091=DIRECTION('center_axis',(0.645833333333334,0.,0.763478425075362));
#21092=DIRECTION('ref_axis',(-0.763478425075362,0.,0.645833333333334));
#21093=DIRECTION('center_axis',(0.645833333333335,-8.40256683676267E-16,
0.763478425075361));
#21094=DIRECTION('ref_axis',(0.763478425075361,-4.92693589372649E-33,-0.645833333333335));
#21095=DIRECTION('center_axis',(0.,-1.,0.));
#21096=DIRECTION('ref_axis',(-1.22464679914735E-16,0.,1.));
#21097=DIRECTION('center_axis',(0.645833333333334,2.80085561225422E-16,
-0.763478425075361));
#21098=DIRECTION('ref_axis',(-0.763478425075361,-2.0725839158777E-31,-0.645833333333334));
#21099=DIRECTION('center_axis',(0.645833333333333,0.,-0.763478425075362));
#21100=DIRECTION('ref_axis',(0.763478425075362,0.,0.645833333333333));
#21101=DIRECTION('center_axis',(0.645833333333334,-3.36102673470506E-15,
-0.763478425075362));
#21102=DIRECTION('ref_axis',(-0.763478425075362,-1.51941949277112E-30,-0.645833333333334));
#21103=DIRECTION('center_axis',(0.,-1.,0.));
#21104=DIRECTION('ref_axis',(0.,0.,-1.));
#21105=DIRECTION('center_axis',(-0.645833333333334,0.,-0.763478425075362));
#21106=DIRECTION('ref_axis',(-0.763478425075362,0.,0.645833333333334));
#21107=DIRECTION('center_axis',(-0.645833333333334,0.,-0.763478425075362));
#21108=DIRECTION('ref_axis',(0.763478425075362,0.,-0.645833333333334));
#21109=DIRECTION('center_axis',(0.,1.,0.));
#21110=DIRECTION('ref_axis',(1.,0.,0.));
#21111=DIRECTION('center_axis',(0.,1.,0.));
#21112=DIRECTION('ref_axis',(0.,0.,1.));
#21113=DIRECTION('center_axis',(-0.0936591325004365,-0.988529372823465,
-0.11848057209734));
#21114=DIRECTION('ref_axis',(1.42799135152678E-16,0.119003673873871,-0.992893813861544));
#21115=DIRECTION('center_axis',(-0.564981881496666,-0.784698449006113,-0.255036894797377));
#21116=DIRECTION('ref_axis',(0.811534832728152,-0.58430404351578,-3.34937223530467E-16));
#21117=DIRECTION('center_axis',(1.,0.,0.));
#21118=DIRECTION('ref_axis',(0.,0.342020143325671,0.939692620785908));
#21119=DIRECTION('center_axis',(-1.,0.,0.));
#21120=DIRECTION('ref_axis',(0.,0.,-1.));
#21121=DIRECTION('center_axis',(0.,1.,0.));
#21122=DIRECTION('ref_axis',(1.,0.,0.));
#21123=DIRECTION('center_axis',(0.,-1.,0.));
#21124=DIRECTION('ref_axis',(0.,0.,-1.));
#21125=DIRECTION('center_axis',(1.,0.,0.));
#21126=DIRECTION('ref_axis',(0.,1.,0.));
#21127=DIRECTION('',(0.,0.939692620785908,-0.342020143325669));
#21128=DIRECTION('center_axis',(0.,0.342020143325669,0.939692620785908));
#21129=DIRECTION('ref_axis',(1.,0.,0.));
#21130=DIRECTION('center_axis',(0.,-0.844082777626919,0.53621289103641));
#21131=DIRECTION('ref_axis',(-1.,0.,0.));
#21132=DIRECTION('',(-1.,0.,0.));
#21133=DIRECTION('center_axis',(0.,-0.84408277762692,0.536212891036408));
#21134=DIRECTION('ref_axis',(-3.60441158372807E-15,-0.536212891036408,-0.84408277762692));
#21135=DIRECTION('',(-1.,0.,0.));
#21136=DIRECTION('center_axis',(0.,0.,-1.));
#21137=DIRECTION('ref_axis',(1.,0.,0.));
#21138=DIRECTION('center_axis',(0.,0.,1.));
#21139=DIRECTION('ref_axis',(1.,0.,0.));
#21140=DIRECTION('center_axis',(0.,0.,1.));
#21141=DIRECTION('ref_axis',(1.,0.,0.));
#21142=DIRECTION('axis',(0.,0.,1.));
#21143=DIRECTION('refdir',(1.,0.,0.));
#21144=DIRECTION('center_axis',(1.,-1.E-15,0.));
#21145=DIRECTION('ref_axis',(9.91270557701032E-31,9.91270557701032E-16,
1.));
#21146=DIRECTION('center_axis',(1.,-1.E-15,0.));
#21147=DIRECTION('ref_axis',(9.91270557701032E-31,9.91270557701032E-16,
1.));
#21148=DIRECTION('',(-1.,1.E-15,0.));
#21149=DIRECTION('center_axis',(1.,-1.E-15,0.));
#21150=DIRECTION('ref_axis',(9.91270557701032E-31,9.91270557701032E-16,
1.));
#21151=DIRECTION('center_axis',(1.,-1.E-15,0.));
#21152=DIRECTION('ref_axis',(0.,0.,1.));
#21153=DIRECTION('center_axis',(1.,-1.E-15,0.));
#21154=DIRECTION('ref_axis',(0.,0.,1.));
#21155=DIRECTION('',(1.,-1.E-15,0.));
#21156=DIRECTION('center_axis',(-1.,1.E-15,0.));
#21157=DIRECTION('ref_axis',(0.,0.,-1.));
#21158=DIRECTION('center_axis',(1.,-1.E-15,0.));
#21159=DIRECTION('ref_axis',(-1.E-15,-1.,1.E-15));
#21160=DIRECTION('center_axis',(1.,-1.E-15,0.));
#21161=DIRECTION('ref_axis',(-1.E-15,-1.,1.E-15));
#21162=DIRECTION('axis',(0.,0.,1.));
#21163=DIRECTION('refdir',(1.,0.,0.));
#21164=DIRECTION('center_axis',(0.,-1.,0.));
#21165=DIRECTION('ref_axis',(-1.,0.,0.));
#21166=DIRECTION('center_axis',(0.,1.,0.));
#21167=DIRECTION('ref_axis',(-1.,0.,0.));
#21168=DIRECTION('center_axis',(0.,-1.,0.));
#21169=DIRECTION('ref_axis',(-1.,0.,0.));
#21170=DIRECTION('center_axis',(0.,-1.,0.));
#21171=DIRECTION('ref_axis',(-1.,0.,0.));
#21172=DIRECTION('center_axis',(0.,1.,0.));
#21173=DIRECTION('ref_axis',(-1.,0.,0.));
#21174=DIRECTION('center_axis',(0.,-1.,0.));
#21175=DIRECTION('ref_axis',(-1.,0.,0.));
#21176=DIRECTION('center_axis',(0.,-1.,0.));
#21177=DIRECTION('ref_axis',(-1.,0.,0.));
#21178=DIRECTION('center_axis',(0.,1.,0.));
#21179=DIRECTION('ref_axis',(-1.,0.,0.));
#21180=DIRECTION('center_axis',(0.,-1.,0.));
#21181=DIRECTION('ref_axis',(-1.,0.,0.));
#21182=DIRECTION('center_axis',(0.,-1.,0.));
#21183=DIRECTION('ref_axis',(-1.,0.,0.));
#21184=DIRECTION('center_axis',(0.,1.,0.));
#21185=DIRECTION('ref_axis',(-1.,0.,0.));
#21186=DIRECTION('center_axis',(0.,-1.,0.));
#21187=DIRECTION('ref_axis',(-1.,0.,0.));
#21188=DIRECTION('center_axis',(0.,-1.,0.));
#21189=DIRECTION('ref_axis',(0.,0.,1.));
#21190=DIRECTION('',(1.,0.,0.));
#21191=DIRECTION('',(-1.,0.,1.32390688747943E-15));
#21192=DIRECTION('center_axis',(0.,-1.,0.));
#21193=DIRECTION('ref_axis',(0.,0.,1.));
#21194=DIRECTION('',(1.,0.,0.));
#21195=DIRECTION('',(-1.,0.,1.32390688747943E-15));
#21196=DIRECTION('center_axis',(0.,-1.,0.));
#21197=DIRECTION('ref_axis',(-0.999999745434011,0.,-0.000713534802215152));
#21198=DIRECTION('',(0.,1.,0.));
#21199=DIRECTION('',(0.,1.,0.));
#21200=DIRECTION('center_axis',(0.,-1.,0.));
#21201=DIRECTION('ref_axis',(-0.999999925770602,0.,-0.000385303503088288));
#21202=DIRECTION('',(0.,1.,0.));
#21203=DIRECTION('',(0.,1.,0.));
#21204=DIRECTION('center_axis',(-1.32390688747943E-15,0.,-1.));
#21205=DIRECTION('ref_axis',(1.,0.,-1.32390688747943E-15));
#21206=DIRECTION('center_axis',(0.,0.,1.));
#21207=DIRECTION('ref_axis',(0.,-1.,0.));
#21208=DIRECTION('axis',(0.,0.,1.));
#21209=DIRECTION('refdir',(1.,0.,0.));
#21210=DIRECTION('center_axis',(0.,-1.,-1.E-15));
#21211=DIRECTION('ref_axis',(0.,-1.E-15,1.));
#21212=DIRECTION('',(1.0605752387249E-16,-0.500000000000006,-0.866025403784435));
#21213=DIRECTION('center_axis',(0.,1.,1.E-15));
#21214=DIRECTION('ref_axis',(0.,1.E-15,-1.));
#21215=DIRECTION('center_axis',(0.,1.,1.E-15));
#21216=DIRECTION('ref_axis',(0.,1.E-15,-1.));
#21217=DIRECTION('center_axis',(0.,1.,1.E-15));
#21218=DIRECTION('ref_axis',(0.,1.E-15,-1.));
#21219=DIRECTION('center_axis',(0.,1.,1.E-15));
#21220=DIRECTION('ref_axis',(0.,1.E-15,-1.));
#21221=DIRECTION('center_axis',(0.,1.,1.E-15));
#21222=DIRECTION('ref_axis',(0.,1.E-15,-1.));
#21223=DIRECTION('center_axis',(0.,1.,1.E-15));
#21224=DIRECTION('ref_axis',(0.,1.E-15,-1.));
#21225=DIRECTION('center_axis',(0.,-1.,-1.E-15));
#21226=DIRECTION('ref_axis',(0.,-1.E-15,1.));
#21227=DIRECTION('center_axis',(0.,-1.,-1.E-15));
#21228=DIRECTION('ref_axis',(0.,-1.E-15,1.));
#21229=DIRECTION('center_axis',(0.,-1.,-1.E-15));
#21230=DIRECTION('ref_axis',(0.,-1.4210854715202E-15,1.));
#21231=DIRECTION('center_axis',(0.,-1.,-1.E-15));
#21232=DIRECTION('ref_axis',(0.,-1.E-15,1.));
#21233=DIRECTION('center_axis',(1.,-1.22464678641072E-31,1.22464678641072E-16));
#21234=DIRECTION('ref_axis',(1.22464678641072E-16,1.77635683940025E-15,
-1.));
#21235=DIRECTION('center_axis',(0.,-1.,-1.E-15));
#21236=DIRECTION('ref_axis',(0.,-1.E-15,1.));
#21237=DIRECTION('center_axis',(0.,-1.,-1.E-15));
#21238=DIRECTION('ref_axis',(0.,-1.E-15,1.));
#21239=DIRECTION('center_axis',(0.,-1.,-1.E-15));
#21240=DIRECTION('ref_axis',(0.,1.E-15,-1.));
#21241=DIRECTION('',(0.,1.,1.E-15));
#21242=DIRECTION('center_axis',(0.,1.,1.E-15));
#21243=DIRECTION('ref_axis',(0.,1.E-15,-1.));
#21244=DIRECTION('center_axis',(0.,-1.,-1.E-15));
#21245=DIRECTION('ref_axis',(0.,0.,1.));
#21246=DIRECTION('center_axis',(0.,-1.,-1.E-15));
#21247=DIRECTION('ref_axis',(0.,-1.E-15,1.));
#21248=DIRECTION('center_axis',(-1.,1.22464675805151E-31,-1.22464675805151E-16));
#21249=DIRECTION('ref_axis',(1.22464675805151E-16,0.,-1.));
#21250=DIRECTION('center_axis',(0.,-1.,-1.E-15));
#21251=DIRECTION('ref_axis',(0.,1.E-15,-1.));
#21252=DIRECTION('center_axis',(0.,-1.,-1.E-15));
#21253=DIRECTION('ref_axis',(0.,1.E-15,-1.));
#21254=DIRECTION('center_axis',(0.,-1.,-1.E-15));
#21255=DIRECTION('ref_axis',(0.,1.E-15,-1.));
#21256=DIRECTION('',(0.,1.,1.E-15));
#21257=DIRECTION('center_axis',(0.,1.,1.E-15));
#21258=DIRECTION('ref_axis',(0.,1.E-15,-1.));
#21259=DIRECTION('center_axis',(0.,1.,1.E-15));
#21260=DIRECTION('ref_axis',(0.,1.E-15,-1.));
#21261=DIRECTION('center_axis',(0.,-1.,-1.E-15));
#21262=DIRECTION('ref_axis',(0.,0.,1.));
#21263=DIRECTION('center_axis',(0.,-1.,-1.E-15));
#21264=DIRECTION('ref_axis',(0.,-1.E-15,1.));
#21265=DIRECTION('center_axis',(-1.,1.22464683445529E-31,-1.22464683445529E-16));
#21266=DIRECTION('ref_axis',(1.22464683445529E-16,0.,-1.));
#21267=DIRECTION('center_axis',(0.,-1.,-1.E-15));
#21268=DIRECTION('ref_axis',(0.,-1.E-15,1.));
#21269=DIRECTION('center_axis',(0.,-1.,-1.E-15));
#21270=DIRECTION('ref_axis',(0.,-1.E-15,1.));
#21271=DIRECTION('',(-8.65956056235494E-17,0.707106781186546,0.707106781186549));
#21272=DIRECTION('center_axis',(0.,1.,1.E-15));
#21273=DIRECTION('ref_axis',(0.,1.E-15,-1.));
#21274=DIRECTION('center_axis',(0.,-1.,-1.E-15));
#21275=DIRECTION('ref_axis',(0.,-1.E-15,1.));
#21276=DIRECTION('',(-4.03364556963302E-17,0.944200181445821,0.329372156318165));
#21277=DIRECTION('center_axis',(0.,-1.,-1.E-15));
#21278=DIRECTION('ref_axis',(0.,-1.E-15,1.));
#21279=DIRECTION('center_axis',(0.,-1.,-1.E-15));
#21280=DIRECTION('ref_axis',(1.22464679914735E-16,1.E-15,-1.));
#21281=DIRECTION('center_axis',(0.,-1.,-1.E-15));
#21282=DIRECTION('ref_axis',(0.,-1.E-15,1.));
#21283=DIRECTION('center_axis',(0.,-1.,-1.E-15));
#21284=DIRECTION('ref_axis',(0.,-1.E-15,1.));
#21285=DIRECTION('center_axis',(0.,-1.,-1.E-15));
#21286=DIRECTION('ref_axis',(0.,-1.E-15,1.));
#21287=DIRECTION('center_axis',(0.,-1.,-1.E-15));
#21288=DIRECTION('ref_axis',(0.,-1.E-15,1.));
#21289=DIRECTION('center_axis',(0.,-1.,-1.E-15));
#21290=DIRECTION('ref_axis',(0.,-1.E-15,1.));
#21291=DIRECTION('center_axis',(0.,1.,1.E-15));
#21292=DIRECTION('ref_axis',(-1.,0.,0.));
#21293=DIRECTION('',(0.499999999999983,-8.96640562630007E-16,0.866025403784448));
#21294=DIRECTION('',(1.,-6.12303176911189E-17,-6.12303176911189E-32));
#21295=DIRECTION('center_axis',(0.,-1.,-1.E-15));
#21296=DIRECTION('ref_axis',(0.,-1.E-15,1.));
#21297=DIRECTION('center_axis',(0.,-1.,-1.E-15));
#21298=DIRECTION('ref_axis',(0.,-1.E-15,1.));
#21299=DIRECTION('center_axis',(0.,-1.,-1.E-15));
#21300=DIRECTION('ref_axis',(0.,-1.E-15,1.));
#21301=DIRECTION('center_axis',(0.,-1.,-1.E-15));
#21302=DIRECTION('ref_axis',(0.,-1.E-15,1.));
#21303=DIRECTION('center_axis',(0.,1.,1.E-15));
#21304=DIRECTION('ref_axis',(-1.,0.,0.));
#21305=DIRECTION('',(1.,-6.12303176911189E-17,-6.12303176911189E-32));
#21306=DIRECTION('',(0.499999999999983,8.3541024493889E-16,-0.866025403784448));
#21307=DIRECTION('center_axis',(0.,1.,1.E-15));
#21308=DIRECTION('ref_axis',(-1.,0.,0.));
#21309=DIRECTION('',(0.499999999999983,8.3541024493889E-16,-0.866025403784448));
#21310=DIRECTION('',(-0.499999999999983,8.96640562630007E-16,-0.866025403784448));
#21311=DIRECTION('center_axis',(0.,-1.,-1.E-15));
#21312=DIRECTION('ref_axis',(0.,-1.E-15,1.));
#21313=DIRECTION('center_axis',(0.,1.E-15,-1.));
#21314=DIRECTION('ref_axis',(1.,0.,0.));
#21315=DIRECTION('',(1.,-6.12303176911189E-17,-6.12303176911189E-32));
#21316=DIRECTION('',(0.,-1.,-1.E-15));
#21317=DIRECTION('',(0.,-1.,-1.E-15));
#21318=DIRECTION('',(-1.,0.,0.));
#21319=DIRECTION('center_axis',(-0.866025403784448,4.99999999999983E-16,
-0.499999999999983));
#21320=DIRECTION('ref_axis',(-2.30491487599793E-32,-1.,-1.E-15));
#21321=DIRECTION('',(0.499999999999983,8.3541024493889E-16,-0.866025403784448));
#21322=DIRECTION('',(0.,-1.,-1.E-15));
#21323=DIRECTION('',(-0.499999999999983,-8.66025403784449E-16,0.866025403784448));
#21324=DIRECTION('center_axis',(-0.866025403784448,-4.99999999999983E-16,
0.499999999999983));
#21325=DIRECTION('ref_axis',(-2.30491487599793E-32,1.,1.E-15));
#21326=DIRECTION('',(-0.499999999999983,8.96640562630007E-16,-0.866025403784448));
#21327=DIRECTION('',(-0.499999999999983,8.96640562630007E-16,-0.866025403784448));
#21328=DIRECTION('',(0.,-1.,-1.E-15));
#21329=DIRECTION('',(0.499999999999983,-8.66025403784449E-16,0.866025403784448));
#21330=DIRECTION('center_axis',(0.,-1.E-15,1.));
#21331=DIRECTION('ref_axis',(0.,1.,1.E-15));
#21332=DIRECTION('',(-1.,6.12303176911189E-17,6.12303176911189E-32));
#21333=DIRECTION('',(-1.,6.12303176911189E-17,6.12303176911189E-32));
#21334=DIRECTION('',(-1.,6.12303176911189E-17,6.12303176911189E-32));
#21335=DIRECTION('',(0.,-1.,-1.E-15));
#21336=DIRECTION('',(1.,0.,0.));
#21337=DIRECTION('center_axis',(0.866025403784448,4.99999999999983E-16,
-0.499999999999983));
#21338=DIRECTION('ref_axis',(-0.499999999999983,8.66025403784449E-16,-0.866025403784448));
#21339=DIRECTION('',(0.499999999999983,-8.96640562630007E-16,0.866025403784448));
#21340=DIRECTION('',(0.,-1.,-1.E-15));
#21341=DIRECTION('',(0.499999999999983,-8.96640562630007E-16,0.866025403784448));
#21342=DIRECTION('',(-0.499999999999983,8.66025403784449E-16,-0.866025403784448));
#21343=DIRECTION('center_axis',(0.866025403784448,-4.99999999999983E-16,
0.499999999999983));
#21344=DIRECTION('ref_axis',(-2.30491487599793E-32,-1.,-1.E-15));
#21345=DIRECTION('',(-0.499999999999983,-8.3541024493889E-16,0.866025403784448));
#21346=DIRECTION('',(-0.499999999999983,-8.3541024493889E-16,0.866025403784448));
#21347=DIRECTION('',(-0.499999999999983,-8.3541024493889E-16,0.866025403784448));
#21348=DIRECTION('',(0.499999999999983,8.66025403784449E-16,-0.866025403784448));
#21349=DIRECTION('center_axis',(0.,1.,1.E-15));
#21350=DIRECTION('ref_axis',(-1.,0.,0.));
#21351=DIRECTION('center_axis',(0.,1.,1.E-15));
#21352=DIRECTION('ref_axis',(-1.,0.,0.));
#21353=DIRECTION('center_axis',(0.,1.,1.E-15));
#21354=DIRECTION('ref_axis',(-1.,0.,0.));
#21355=DIRECTION('center_axis',(0.,1.,1.E-15));
#21356=DIRECTION('ref_axis',(-1.,0.,0.));
#21357=DIRECTION('',(0.,0.,1.));
#21358=DIRECTION('',(1.,0.,0.));
#21359=DIRECTION('',(0.,0.,1.));
#21360=DIRECTION('',(1.,0.,0.));
#21361=DIRECTION('',(0.,0.,1.));
#21362=DIRECTION('',(1.,0.,0.));
#21363=DIRECTION('',(0.,0.,1.));
#21364=DIRECTION('',(1.,0.,0.));
#21365=DIRECTION('',(0.,0.,1.));
#21366=DIRECTION('',(1.,0.,0.));
#21367=DIRECTION('',(0.,0.,1.));
#21368=DIRECTION('',(1.,0.,0.));
#21369=DIRECTION('',(0.,0.,1.));
#21370=DIRECTION('',(1.,0.,0.));
#21371=DIRECTION('',(0.,0.,1.));
#21372=DIRECTION('',(1.,0.,0.));
#21373=DIRECTION('',(0.,0.,1.));
#21374=DIRECTION('',(1.,0.,0.));
#21375=DIRECTION('',(0.,0.,1.));
#21376=DIRECTION('',(1.,0.,0.));
#21377=DIRECTION('',(0.,0.,1.));
#21378=DIRECTION('',(1.,0.,0.));
#21379=DIRECTION('',(0.,0.,1.));
#21380=DIRECTION('',(1.,0.,0.));
#21381=DIRECTION('',(0.872322309961348,-0.488930550344967,0.000839334894752671));
#21382=DIRECTION('',(-0.4309815049242,-0.768119965562789,0.473546894105632));
#21383=DIRECTION('',(0.,0.,1.));
#21384=DIRECTION('',(1.,0.,0.));
#21385=DIRECTION('',(0.,0.,1.));
#21386=DIRECTION('',(1.,0.,0.));
#21387=CARTESIAN_POINT('',(0.,0.,0.));
#21388=CARTESIAN_POINT('',(0.,0.,0.));
#21389=CARTESIAN_POINT('Origin',(-21.1807292643367,67.0504890645402,23.2726194591173));
#21390=CARTESIAN_POINT('',(-18.4019669354104,62.2805003312476,20.1761396184593));
#21391=CARTESIAN_POINT('Origin',(-21.6117107692609,66.2823690989774,23.746166353223));
#21392=CARTESIAN_POINT('',(-17.540003925562,63.8167402623731,19.229045830248));
#21393=CARTESIAN_POINT('Origin',(-17.9709854304862,63.0486202968104,19.7025927243536));
#21394=CARTESIAN_POINT('Origin',(-20.7497477594125,67.818609030103,22.7990725650117));
#21395=CARTESIAN_POINT('Origin',(-19.370606943655,70.2765929199039,21.2837225038737));
#21396=CARTESIAN_POINT('',(-20.4706781590466,58.5935244965462,22.4491647101663));
#21397=CARTESIAN_POINT('',(-16.1608631098046,66.2747241521741,17.71369576911));
#21398=CARTESIAN_POINT('Origin',(-23.680421992897,62.595393264276,26.01919144493));
#21399=CARTESIAN_POINT('Origin',(-19.370606943655,70.2765929199039,21.2837225038737));
#21400=CARTESIAN_POINT('',(-16.0315686583273,66.5051601418429,17.5716317008783));
#21401=CARTESIAN_POINT('Origin',(-19.2413124921778,70.5070289095728,21.141658435642));
#21402=CARTESIAN_POINT('',(-16.1608631098046,66.2747241521741,17.71369576911));
#21403=CARTESIAN_POINT('Origin',(-26.7094064904571,75.8640834081228,29.4304205240279));
#21404=CARTESIAN_POINT('',(-35.1523449475666,57.3165090584927,38.6916365627459));
#21405=CARTESIAN_POINT('Origin',(-36.3078527277528,58.7571818148754,39.9768461872608));
#21406=CARTESIAN_POINT('',(-28.6876223737037,68.8383085419345,31.5884331511614));
#21407=CARTESIAN_POINT('',(-25.5538987102709,74.42341065174,28.145210899513));
#21408=CARTESIAN_POINT('Origin',(-29.8431301538898,70.2789812983173,32.8736427756763));
#21409=CARTESIAN_POINT('Origin',(-44.6514843000067,41.123844669555,31.2333209653637));
#21410=CARTESIAN_POINT('',(-56.5796715376924,43.0865205259419,23.5608863644389));
#21411=CARTESIAN_POINT('Origin',(-55.0389944974442,41.1656235174316,21.8472735317523));
#21412=CARTESIAN_POINT('',(-46.1921613402549,43.0447416780653,32.9469337980503));
#21413=CARTESIAN_POINT('',(-46.1921613402549,43.0447416780653,32.9469337980503));
#21414=CARTESIAN_POINT('Origin',(-44.6514843000067,41.123844669555,31.2333209653637));
#21415=CARTESIAN_POINT('Origin',(-30.14514456676,51.0735937808341,33.1223948565145));
#21416=CARTESIAN_POINT('',(-33.9968371673805,55.8758363021099,37.4064269382309));
#21417=CARTESIAN_POINT('Origin',(-30.14514456676,51.0735937808341,33.1223948565145));
#21418=CARTESIAN_POINT('',(-37.1511444364363,46.7539638900993,40.8566862547723));
#21419=CARTESIAN_POINT('',(-33.9968371673805,55.8758363021099,37.4064269382309));
#21420=CARTESIAN_POINT('',(-34.1986576758722,40.5370964920739,33.4596727214903));
#21421=CARTESIAN_POINT('Origin',(-34.4549596160019,43.3923941252062,37.8578637975708));
#21422=CARTESIAN_POINT('',(-38.7920691336964,46.2641048771473,38.5686790961612));
#21423=CARTESIAN_POINT('Ctrl Pts',(-34.1986576758724,40.5370964920741,33.45967272149));
#21424=CARTESIAN_POINT('Ctrl Pts',(-34.4388615494162,40.8333519186998,33.1851139522211));
#21425=CARTESIAN_POINT('Ctrl Pts',(-34.6772423136203,41.1581168909091,32.9429616455856));
#21426=CARTESIAN_POINT('Ctrl Pts',(-35.1372914510471,41.801250072958,32.5593008372811));
#21427=CARTESIAN_POINT('Ctrl Pts',(-35.3897505951037,42.1636734305047,32.3895385975851));
#21428=CARTESIAN_POINT('Ctrl Pts',(-35.909488224246,42.9090203866848,32.1640747104879));
#21429=CARTESIAN_POINT('Ctrl Pts',(-36.1772556001164,43.2919128390833,32.1093985180926));
#21430=CARTESIAN_POINT('Ctrl Pts',(-36.6333809306673,43.9313791060147,32.1273079452342));
#21431=CARTESIAN_POINT('Ctrl Pts',(-36.8589905041216,44.2427361852693,32.1806242970088));
#21432=CARTESIAN_POINT('Ctrl Pts',(-37.2963729868296,44.8287243856034,32.4038996940975));
#21433=CARTESIAN_POINT('Ctrl Pts',(-37.508133475892,45.1030694943354,32.5746329487417));
#21434=CARTESIAN_POINT('Ctrl Pts',(-37.8722215204345,45.5570099486458,32.9795886461766));
#21435=CARTESIAN_POINT('Ctrl Pts',(-38.0527564083383,45.7717738461373,33.2451845991546));
#21436=CARTESIAN_POINT('Ctrl Pts',(-38.3624638742306,46.1172481196795,33.8528574732792));
#21437=CARTESIAN_POINT('Ctrl Pts',(-38.4919084454301,46.2485681404971,34.1944488943104));
#21438=CARTESIAN_POINT('Ctrl Pts',(-38.7074431493876,46.4465192669056,34.9235910712811));
#21439=CARTESIAN_POINT('Ctrl Pts',(-38.8006550994683,46.5136913570681,35.3797652993612));
#21440=CARTESIAN_POINT('Ctrl Pts',(-38.912980144043,46.5563922963369,36.3082387598139));
#21441=CARTESIAN_POINT('Ctrl Pts',(-38.93244337546,46.5329983810086,36.7804457429138));
#21442=CARTESIAN_POINT('Ctrl Pts',(-38.9129366855058,46.4391280537729,37.6540984000036));
#21443=CARTESIAN_POINT('Ctrl Pts',(-38.8718148058301,46.3603030101108,38.1156512344973));
#21444=CARTESIAN_POINT('Ctrl Pts',(-38.7920691336965,46.2641048771474,38.5686790961607));
#21445=CARTESIAN_POINT('Origin',(-34.4549596160019,43.3923941252062,37.8578637975708));
#21446=CARTESIAN_POINT('Origin',(-30.14514456676,51.0735937808341,33.1223948565145));
#21447=CARTESIAN_POINT('',(-15.2504730073405,57.296061780678,25.0955865772773));
#21448=CARTESIAN_POINT('',(-31.8377985837207,68.1554663069955,27.6138057991849));
#21449=CARTESIAN_POINT('Origin',(-23.680421992897,62.595393264276,26.01919144493));
#21450=CARTESIAN_POINT('',(-21.7151955812034,45.7742622972361,32.1987899888618));
#21451=CARTESIAN_POINT('',(-21.7151955812034,45.7742622972361,32.1987899888618));
#21452=CARTESIAN_POINT('',(-38.3025211575837,56.6336668235536,34.7170092107694));
#21453=CARTESIAN_POINT('Origin',(-30.14514456676,51.0735937808341,33.1223948565145));
#21454=CARTESIAN_POINT('',(-38.3025211575837,56.6336668235536,34.7170092107694));
#21455=CARTESIAN_POINT('Origin',(-37.9028116553955,37.2474344007039,41.6462389504159));
#21456=CARTESIAN_POINT('',(-38.3363435749778,44.6416339848016,42.1589402135628));
#21457=CARTESIAN_POINT('Origin',(-35.6401587544779,41.2800642198147,39.1601177563349));
#21458=CARTESIAN_POINT('',(-38.6265215709417,44.4465365776215,42.1063169921011));
#21459=CARTESIAN_POINT('Origin',(-32.946681053115,37.9218104167842,36.1642663517435));
#21460=CARTESIAN_POINT('',(-33.2402691976586,37.7310239811241,36.1154759879024));
#21461=CARTESIAN_POINT('Origin',(-35.7479041307745,41.0880342285179,39.2785044798877));
#21462=CARTESIAN_POINT('',(-32.9439739341091,37.9184944550155,36.1612952991598));
#21463=CARTESIAN_POINT('Origin',(-38.3336988439063,44.6382773263309,42.1559586889937));
#21464=CARTESIAN_POINT('Origin',(-35.6401587545408,41.2800642199063,39.1601177563553));
#21465=CARTESIAN_POINT('Origin',(-40.1823782592027,41.1368009396544,35.2368865760798));
#21466=CARTESIAN_POINT('',(-48.8866349100272,38.6188758778939,23.2308060524478));
#21467=CARTESIAN_POINT('Origin',(-50.9408709636915,41.1800718892409,25.5156231626966));
#21468=CARTESIAN_POINT('',(-38.1281422055384,38.5756049283073,32.952069465831));
#21469=CARTESIAN_POINT('',(-38.1281422055384,38.5756049283073,32.952069465831));
#21470=CARTESIAN_POINT('Origin',(-40.1823782592027,41.1368009396544,35.2368865760798));
#21471=CARTESIAN_POINT('Origin',(-40.0919488391595,41.2979694404271,35.1375259990993));
#21472=CARTESIAN_POINT('',(-42.3546017400116,37.2653396212225,37.6236471931538));
#21473=CARTESIAN_POINT('Origin',(-40.0919488391595,41.2979694404271,35.1375259990993));
#21474=CARTESIAN_POINT('',(-41.7981279794346,37.2631014686576,38.1264711628116));
#21475=CARTESIAN_POINT('',(-42.3546017400116,37.2653396212225,37.6236471931539));
#21476=CARTESIAN_POINT('Origin',(-35.6400470347534,41.2800655852767,39.1600770240352));
#21477=CARTESIAN_POINT('Origin',(-35.6401289648185,41.2801677346543,39.1601681504663));
#21478=CARTESIAN_POINT('Origin',(-40.1823782592027,41.1368009396544,35.2368865760798));
#21479=CARTESIAN_POINT('',(-51.320302201284,37.9647877832075,19.9549241160537));
#21480=CARTESIAN_POINT('Origin',(-53.9087310201022,41.19200870292,22.8338953245219));
#21481=CARTESIAN_POINT('',(-48.3524421448733,37.9528509695284,22.6366519542284));
#21482=CARTESIAN_POINT('',(-37.5939494403844,37.9095800199419,32.3579153676115));
#21483=CARTESIAN_POINT('Origin',(-50.9408709636915,41.1800718892409,25.5156231626966));
#21484=CARTESIAN_POINT('Origin',(-53.9087310201022,41.19200870292,22.8338953245219));
#21485=CARTESIAN_POINT('',(-52.967442487592,38.6352889967025,19.5434302749577));
#21486=CARTESIAN_POINT('',(-51.320302201284,37.9647877832074,19.9549241160537));
#21487=CARTESIAN_POINT('Origin',(-55.0216785412562,41.1964850080496,21.8282473852064));
#21488=CARTESIAN_POINT('Origin',(-17.0720934772965,71.2619488126406,18.7443506111377));
#21489=CARTESIAN_POINT('',(-17.2046121060751,71.4924445117698,18.892034549701));
#21490=CARTESIAN_POINT('Origin',(-17.0505444020503,71.3003548109187,18.7206732664324));
#21491=CARTESIAN_POINT('',(-17.2261611813213,71.4540385134916,18.9157118944063));
#21492=CARTESIAN_POINT('',(-17.2261611813213,71.4540385134916,18.9157118944063));
#21493=CARTESIAN_POINT('Origin',(-17.0720934772965,71.2619488126406,18.7443506111377));
#21494=CARTESIAN_POINT('Origin',(-19.1263295309608,73.8231448239877,21.0291677213865));
#21495=CARTESIAN_POINT('',(-19.2588481597394,74.0536405231169,21.1768516599498));
#21496=CARTESIAN_POINT('Origin',(-19.1047804557146,73.8615508222658,21.0054903766812));
#21497=CARTESIAN_POINT('',(-19.2803972349856,74.0152345248387,21.2005290046551));
#21498=CARTESIAN_POINT('',(-19.2803972349856,74.0152345248387,21.2005290046551));
#21499=CARTESIAN_POINT('Origin',(-19.1263295309608,73.8231448239877,21.0291677213865));
#21500=CARTESIAN_POINT('Origin',(-19.370606943655,70.2765929199039,21.2837225038737));
#21501=CARTESIAN_POINT('',(-16.0234263752182,70.0197568052452,17.578264711308));
#21502=CARTESIAN_POINT('Origin',(-18.0776624288824,72.5809528165923,19.8630818215568));
#21503=CARTESIAN_POINT('',(-15.8079356227561,70.4038167880266,17.3414912642552));
#21504=CARTESIAN_POINT('',(-17.3163708899908,67.7153969085568,18.9989053936249));
#21505=CARTESIAN_POINT('Origin',(-17.8621716764203,72.9650127993737,19.626308374504));
#21506=CARTESIAN_POINT('Origin',(-18.1854078051135,72.3889228252016,19.9814685450832));
#21507=CARTESIAN_POINT('',(-16.1976283734343,68.931487338264,17.7662094666325));
#21508=CARTESIAN_POINT('Origin',(-18.5086439338066,71.8128328510295,20.3366287156624));
#21509=CARTESIAN_POINT('',(-15.551156116048,70.0836672866082,17.0558891254741));
#21510=CARTESIAN_POINT('Origin',(-15.8743922447412,69.5075773124361,17.4110492960533));
#21511=CARTESIAN_POINT('Origin',(-17.8621716764203,72.9650127993737,19.626308374504));
#21512=CARTESIAN_POINT('Origin',(-19.370606943655,70.2765929199039,21.2837225038737));
#21513=CARTESIAN_POINT('',(-16.3516960774591,69.123577039115,17.9375707499012));
#21514=CARTESIAN_POINT('Origin',(-18.5086439338066,71.8128328510295,20.3366287156624));
#21515=CARTESIAN_POINT('',(-16.9981683348454,67.9713970907709,18.6478910910597));
#21516=CARTESIAN_POINT('',(-17.2136590873075,67.5873371079895,18.8846645381125));
#21517=CARTESIAN_POINT('Origin',(-19.1551161911929,70.6606529026853,21.0469490568209));
#21518=CARTESIAN_POINT('Origin',(-19.1551161911929,70.6606529026853,21.0469490568209));
#21519=CARTESIAN_POINT('',(-16.9733950822979,67.548871400251,18.6185938760227));
#21520=CARTESIAN_POINT('Origin',(-19.2844106426702,70.4302169130165,21.1890131250526));
#21521=CARTESIAN_POINT('',(-16.9981683348454,67.9713970907709,18.6478910910597));
#21522=CARTESIAN_POINT('Origin',(-19.370606943655,70.2765929199039,21.2837225038737));
#21523=CARTESIAN_POINT('',(-16.305768364857,66.7164826965632,17.8760283151918));
#21524=CARTESIAN_POINT('Origin',(-19.2844106426702,70.4302169130165,21.1890131250526));
#21525=CARTESIAN_POINT('',(-16.2626702143646,66.7932946931195,17.8286736257813));
#21526=CARTESIAN_POINT('',(-16.3919646658418,66.5628587034506,17.970737694013));
#21527=CARTESIAN_POINT('Origin',(-19.2413124921778,70.5070289095728,21.141658435642));
#21528=CARTESIAN_POINT('Origin',(-16.9733950822979,67.548871400251,18.6185938760227));
#21529=CARTESIAN_POINT('Origin',(-16.3516960774591,69.123577039115,17.9375707499012));
#21530=CARTESIAN_POINT('Origin',(-15.8079356227561,70.4038167880266,17.3414912642552));
#21531=CARTESIAN_POINT('Origin',(-19.1263295309608,73.8231448239877,21.0291677213865));
#21532=CARTESIAN_POINT('Origin',(-17.0720934772965,71.2619488126406,18.7443506111377));
#21533=CARTESIAN_POINT('Origin',(-5.87326165443273,62.5237723822018,42.109558473978));
#21534=CARTESIAN_POINT('',(-10.1675813678396,57.8258167527581,46.8411576859596));
#21535=CARTESIAN_POINT('',(-10.4261702707941,57.3649447734205,47.125285822423));
#21536=CARTESIAN_POINT('',(-10.1675813678396,57.8258167527581,46.8411576859596));
#21537=CARTESIAN_POINT('',(-11.2974111973549,59.234474558999,48.0978070965964));
#21538=CARTESIAN_POINT('',(-11.2974111973549,59.234474558999,48.0978070965964));
#21539=CARTESIAN_POINT('',(-11.5560001003095,58.7736025796614,48.3819352330598));
#21540=CARTESIAN_POINT('',(-11.5560001003095,58.7736025796614,48.3819352330598));
#21541=CARTESIAN_POINT('',(-10.4261702707941,57.3649447734205,47.125285822423));
#21542=CARTESIAN_POINT('Origin',(-11.2974111973549,59.234474558999,48.0978070965964));
#21543=CARTESIAN_POINT('',(-17.975096324279,59.2613323897769,42.0639194607034));
#21544=CARTESIAN_POINT('',(-16.8452664947637,57.852674583536,40.8072700500666));
#21545=CARTESIAN_POINT('',(-17.975096324279,59.2613323897769,42.0639194607034));
#21546=CARTESIAN_POINT('',(-11.2974111973549,59.234474558999,48.0978070965964));
#21547=CARTESIAN_POINT('',(-10.1675813678396,57.8258167527581,46.8411576859596));
#21548=CARTESIAN_POINT('Origin',(-11.5560001003095,58.7736025796614,48.3819352330598));
#21549=CARTESIAN_POINT('',(-18.2336852272336,58.8004604104392,42.3480475971668));
#21550=CARTESIAN_POINT('',(-18.2336852272336,58.8004604104392,42.3480475971668));
#21551=CARTESIAN_POINT('',(-11.5560001003095,58.7736025796614,48.3819352330598));
#21552=CARTESIAN_POINT('Origin',(-10.4261702707941,57.3649447734205,47.125285822423));
#21553=CARTESIAN_POINT('',(-17.1038553977182,57.3918026041983,41.0913981865299));
#21554=CARTESIAN_POINT('',(-17.1038553977182,57.3918026041983,41.0913981865299));
#21555=CARTESIAN_POINT('',(-10.4261702707941,57.3649447734205,47.125285822423));
#21556=CARTESIAN_POINT('Origin',(-5.13129664033005,62.520788178782,42.7799904335217));
#21557=CARTESIAN_POINT('',(-10.3946991891447,50.8066601566478,48.5528405346573));
#21558=CARTESIAN_POINT('',(-10.9118769950537,49.8849161979724,49.121096807584));
#21559=CARTESIAN_POINT('',(-10.3946991891447,50.8066601566478,48.5528405346573));
#21560=CARTESIAN_POINT('',(-11.9353762293929,52.7275571651581,50.2664533673438));
#21561=CARTESIAN_POINT('',(-11.9353762293929,52.7275571651581,50.2664533673438));
#21562=CARTESIAN_POINT('',(-12.452554035302,51.8058132064827,50.8347096402706));
#21563=CARTESIAN_POINT('',(-12.452554035302,51.8058132064827,50.8347096402706));
#21564=CARTESIAN_POINT('',(-10.9118769950537,49.8849161979724,49.121096807584));
#21565=CARTESIAN_POINT('Origin',(-12.452554035302,51.8058132064827,50.8347096402706));
#21566=CARTESIAN_POINT('',(-19.4412226714045,52.6037752062431,43.6568431507283));
#21567=CARTESIAN_POINT('',(-19.3550263704197,52.7573991993557,43.5621337719072));
#21568=CARTESIAN_POINT('',(-19.8722041763287,51.8356552406803,44.1303900448339));
#21569=CARTESIAN_POINT('',(-19.1302391622261,51.8326710372606,44.8008220043776));
#21570=CARTESIAN_POINT('',(-17.7308133709229,48.3627022768391,49.9487268457994));
#21571=CARTESIAN_POINT('',(-12.452554035302,51.8058132064827,50.8347096402706));
#21572=CARTESIAN_POINT('',(-11.9353762293929,52.7275571651581,50.2664533673438));
#21573=CARTESIAN_POINT('Origin',(-10.9118769950537,49.8849161979724,49.121096807584));
#21574=CARTESIAN_POINT('',(-17.5895621219778,49.9117740287503,43.087209171691));
#21575=CARTESIAN_POINT('',(-17.5895621219778,49.9117740287503,43.087209171691));
#21576=CARTESIAN_POINT('',(-10.9118769950537,49.8849161979724,49.121096807584));
#21577=CARTESIAN_POINT('Origin',(-0.643450268341849,55.6976051691234,40.0202968711604));
#21578=CARTESIAN_POINT('',(-1.75639778949586,55.702081474253,39.0146489318449));
#21579=CARTESIAN_POINT('',(-9.17604793052264,55.7319235084507,32.3103293364082));
#21580=CARTESIAN_POINT('',(-0.643450268341849,55.6976051691234,40.0202968711604));
#21581=CARTESIAN_POINT('',(-6.92817584858623,46.4846418874996,44.6972116611125));
#21582=CARTESIAN_POINT('',(-6.92817584858623,46.4846418874996,44.6972116611125));
#21583=CARTESIAN_POINT('',(-14.347825989613,46.5144839216971,37.9928920656758));
#21584=CARTESIAN_POINT('',(-5.81522832743221,46.4801655823699,45.702859600428));
#21585=CARTESIAN_POINT('',(-9.17604793052264,55.7319235084507,32.3103293364082));
#21586=CARTESIAN_POINT('Origin',(-9.11717398970701,66.2625387159302,49.4451674509366));
#21587=CARTESIAN_POINT('',(-10.230121510861,66.2670150210598,48.4395195116211));
#21588=CARTESIAN_POINT('',(-17.6497716518878,66.2968570552574,41.7351999161844));
#21589=CARTESIAN_POINT('',(-9.11717398970701,66.2625387159302,49.4451674509366));
#21590=CARTESIAN_POINT('',(-1.75639778949586,55.702081474253,39.0146489318449));
#21591=CARTESIAN_POINT('',(-17.6497716518878,66.2968570552574,41.7351999161844));
#21592=CARTESIAN_POINT('Origin',(-14.2889520487974,57.0450991291767,55.1277301802041));
#21593=CARTESIAN_POINT('',(-15.4018995699514,57.0495754343063,54.1220822408886));
#21594=CARTESIAN_POINT('',(-22.8215497109782,57.0794174685039,47.417762645452));
#21595=CARTESIAN_POINT('',(-14.2889520487974,57.0450991291767,55.1277301802041));
#21596=CARTESIAN_POINT('',(-10.230121510861,66.2670150210598,48.4395195116211));
#21597=CARTESIAN_POINT('',(-22.8215497109782,57.0794174685039,47.417762645452));
#21598=CARTESIAN_POINT('Origin',(-21.8109151771594,55.9930238221405,35.1010433319011));
#21599=CARTESIAN_POINT('',(-12.4413136191775,55.6742799812288,32.9405810371301));
#21600=CARTESIAN_POINT('',(-9.17604793052264,55.7319235084507,32.3103293364082));
#21601=CARTESIAN_POINT('',(-18.8608012868784,63.6780175166885,40.0806345066575));
#21602=CARTESIAN_POINT('',(-12.4413136191775,55.6742799812288,32.9405810371301));
#21603=CARTESIAN_POINT('',(-17.6497716518878,66.2968570552574,41.7351999161844));
#21604=CARTESIAN_POINT('Origin',(-22.9095517405797,64.7463307123084,30.2097137451623));
#21605=CARTESIAN_POINT('',(-16.1046564110332,49.1452602739451,36.965729637028));
#21606=CARTESIAN_POINT('',(-14.347825989613,46.5144839216971,37.9928920656758));
#21607=CARTESIAN_POINT('',(-16.1046564110332,49.1452602739451,36.965729637028));
#21608=CARTESIAN_POINT('Origin',(-5.81522832743221,46.4801655823699,45.702859600428));
#21609=CARTESIAN_POINT('',(-15.4018995699514,57.0495754343063,54.1220822408886));
#21610=CARTESIAN_POINT('',(-14.347825989613,46.5144839216971,37.9928920656758));
#21611=CARTESIAN_POINT('Origin',(-24.2157427890632,62.2160260775154,25.9631512684015));
#21612=CARTESIAN_POINT('',(-22.524144078734,57.1489978094048,44.1057831065554));
#21613=CARTESIAN_POINT('',(-22.524144078734,57.1489978094048,44.1057831065554));
#21614=CARTESIAN_POINT('',(-17.8143493301715,50.8365021908454,41.8485209392206));
#21615=CARTESIAN_POINT('',(-14.347825989613,46.5144839216971,37.9928920656758));
#21616=CARTESIAN_POINT('',(-19.3550263704197,52.7573991993557,43.5621337719072));
#21617=CARTESIAN_POINT('',(-22.8215497109782,57.0794174685039,47.417762645452));
#21618=CARTESIAN_POINT('Origin',(-19.4430284000212,60.4243124431602,26.3540848716175));
#21619=CARTESIAN_POINT('',(-18.8608012868784,63.6780175166885,40.0806345066575));
#21620=CARTESIAN_POINT('Origin',(-12.4413136191775,55.6742799812288,32.9405810371301));
#21621=CARTESIAN_POINT('',(-13.1832786332802,55.6772641846486,32.2701490775864));
#21622=CARTESIAN_POINT('',(-19.602766300981,63.6810017201083,39.4102025471138));
#21623=CARTESIAN_POINT('',(-13.1832786332802,55.6772641846486,32.2701490775864));
#21624=CARTESIAN_POINT('',(-18.8608012868784,63.6780175166885,40.0806345066575));
#21625=CARTESIAN_POINT('',(-12.4413136191775,55.6742799812288,32.9405810371301));
#21626=CARTESIAN_POINT('Origin',(-16.1046564110332,49.1452602739451,36.965729637028));
#21627=CARTESIAN_POINT('',(-16.8466214251358,49.1482444773649,36.2952976774843));
#21628=CARTESIAN_POINT('',(-16.8466214251358,49.1482444773649,36.2952976774843));
#21629=CARTESIAN_POINT('',(-16.1046564110332,49.1452602739451,36.965729637028));
#21630=CARTESIAN_POINT('Origin',(-22.524144078734,57.1489978094048,44.1057831065554));
#21631=CARTESIAN_POINT('',(-23.2661090928367,57.1519820128245,43.4353511470117));
#21632=CARTESIAN_POINT('',(-23.2661090928367,57.1519820128245,43.4353511470117));
#21633=CARTESIAN_POINT('',(-22.524144078734,57.1489978094048,44.1057831065554));
#21634=CARTESIAN_POINT('Origin',(-18.8608012868784,63.6780175166885,40.0806345066575));
#21635=CARTESIAN_POINT('',(-19.602766300981,63.6810017201083,39.4102025471138));
#21636=CARTESIAN_POINT('Origin',(-49.2169449439947,44.2525517514921,23.6214355862741));
#21637=CARTESIAN_POINT('Origin',(-4.01834911917603,62.5163118736524,43.7856383728372));
#21638=CARTESIAN_POINT('',(-12.872141271287,57.2368305732657,53.5606034227024));
#21639=CARTESIAN_POINT('',(-12.8464633206162,57.2048156231239,53.5320432088243));
#21640=CARTESIAN_POINT('',(-5.16875607004592,47.6323455307141,44.9925392592695));
#21641=CARTESIAN_POINT('',(-8.96762977629839,64.117895313189,49.2701211618736));
#21642=CARTESIAN_POINT('',(-7.4591945090637,66.8063151926587,47.6127070325039));
#21643=CARTESIAN_POINT('',(-8.9933077269692,64.1499102633308,49.2986813757517));
#21644=CARTESIAN_POINT('',(-9.7636462470933,65.110358767586,50.155487792095));
#21645=CARTESIAN_POINT('',(-13.5186135286733,56.0846506249215,54.2709237638608));
#21646=CARTESIAN_POINT('Origin',(-20.5885881684815,57.5590446260281,44.948685785673));
#21647=CARTESIAN_POINT('',(-20.5885881684815,57.5590446260281,44.948685785673));
#21648=CARTESIAN_POINT('',(-12.7979555204034,57.5277104901207,51.9882213608815));
#21649=CARTESIAN_POINT('',(-20.5885881684815,57.5590446260281,44.948685785673));
#21650=CARTESIAN_POINT('',(-6.63524735941056,49.8441224560794,45.1337700301351));
#21651=CARTESIAN_POINT('',(-12.7979555204034,57.5277104901207,51.9882213608815));
#21652=CARTESIAN_POINT('',(-14.4258800074887,49.8754565919869,38.0942344549266));
#21653=CARTESIAN_POINT('',(-14.4258800074887,49.8754565919869,38.0942344549266));
#21654=CARTESIAN_POINT('',(-20.5885881684815,57.5590446260281,44.948685785673));
#21655=CARTESIAN_POINT('Origin',(-14.4258800074887,49.8754565919869,38.0942344549266));
#21656=CARTESIAN_POINT('',(-6.54195230665701,49.6127912053846,45.4769636862299));
#21657=CARTESIAN_POINT('',(-8.26791078259758,53.8924193432378,39.1278810484763));
#21658=CARTESIAN_POINT('',(-3.26649286923312,55.4505029436618,41.8780072910271));
#21659=CARTESIAN_POINT('',(-6.41265785517975,49.8432271950535,45.3348996179982));
#21660=CARTESIAN_POINT('',(-3.61837682494118,55.2209622150189,41.8189417713957));
#21661=CARTESIAN_POINT('',(-13.8816588664263,48.5260242962674,40.0961974488129));
#21662=CARTESIAN_POINT('',(-11.4090094730193,55.2522963509264,34.7794061961872));
#21663=CARTESIAN_POINT('',(-11.4090094730193,55.2522963509264,34.7794061961872));
#21664=CARTESIAN_POINT('',(-14.4258800074887,49.8754565919869,38.0942344549266));
#21665=CARTESIAN_POINT('Origin',(-10.1675813678396,57.8258167527581,46.8411576859596));
#21666=CARTESIAN_POINT('',(-16.8452664947637,57.852674583536,40.8072700500666));
#21667=CARTESIAN_POINT('Origin',(-6.41265785517975,49.8432271950535,45.3348996179982));
#21668=CARTESIAN_POINT('',(-5.96477254084083,48.6248089851111,45.8779058894909));
#21669=CARTESIAN_POINT('',(-6.62440655891647,49.7539315225666,45.4196862286212));
#21670=CARTESIAN_POINT('',(-2.08593899652305,55.5378886751762,41.6159838425402));
#21671=CARTESIAN_POINT('',(-0.577503729288366,58.226308554646,39.9585697131705));
#21672=CARTESIAN_POINT('',(-7.37032299817759,55.1467334960166,42.7888507071959));
#21673=CARTESIAN_POINT('Origin',(-11.4090094730193,55.2522963509264,34.7794061961872));
#21674=CARTESIAN_POINT('',(-9.78108498593402,62.9045502490602,48.673393102142));
#21675=CARTESIAN_POINT('',(-3.61837682494118,55.2209622150189,41.8189417713957));
#21676=CARTESIAN_POINT('',(-17.5717176340121,62.9358843849677,41.6338575269335));
#21677=CARTESIAN_POINT('',(-17.5717176340121,62.9358843849677,41.6338575269335));
#21678=CARTESIAN_POINT('',(-11.4090094730193,55.2522963509264,34.7794061961872));
#21679=CARTESIAN_POINT('Origin',(-12.7979555204034,57.5277104901207,51.9882213608815));
#21680=CARTESIAN_POINT('',(-12.7046604676499,57.2963792394259,52.3314150169762));
#21681=CARTESIAN_POINT('',(-15.5190612257151,64.274871968718,41.9784063914501));
#21682=CARTESIAN_POINT('',(-12.2117267406717,57.6146718103806,48.1578027310283));
#21683=CARTESIAN_POINT('',(-5.16875607004592,47.6323455307141,44.9925392592695));
#21684=CARTESIAN_POINT('Origin',(-3.61837682494118,55.2209622150189,41.8189417713957));
#21685=CARTESIAN_POINT('',(-9.7636462470933,65.110358767586,50.155487792095));
#21686=CARTESIAN_POINT('',(-9.42920103022596,63.1340909777031,48.7324586217735));
#21687=CARTESIAN_POINT('',(-9.49513978078704,62.9935475012051,48.6556496874734));
#21688=CARTESIAN_POINT('',(-15.9390542108251,58.8875874978093,47.6397465085924));
#21689=CARTESIAN_POINT('Origin',(-12.5509467813568,62.5506302129796,36.075670838085));
#21690=CARTESIAN_POINT('',(-17.9005456311563,50.6828781977328,41.9432303180417));
#21691=CARTESIAN_POINT('',(-17.8143493301715,50.8365021908454,41.8485209392206));
#21692=CARTESIAN_POINT('',(-18.6708841512804,51.643326701988,42.800036734385));
#21693=CARTESIAN_POINT('Origin',(-17.5717176340121,62.9358843849677,41.6338575269335));
#21694=CARTESIAN_POINT('',(-9.55849548170321,62.9036549880343,48.8745226900051));
#21695=CARTESIAN_POINT('',(-17.5717176340121,62.9358843849677,41.6338575269335));
#21696=CARTESIAN_POINT('Origin',(-18.6708841512804,51.643326701988,42.800036734385));
#21697=CARTESIAN_POINT('',(-16.3767264361818,46.9044677697183,47.5487267009233));
#21698=CARTESIAN_POINT('Origin',(-4.01834911917603,62.5163118736524,43.7856383728372));
#21699=CARTESIAN_POINT('',(-2.06026104585225,55.5058737250344,41.5874236286621));
#21700=CARTESIAN_POINT('',(-9.7636462470933,65.110358767586,50.155487792095));
#21701=CARTESIAN_POINT('',(-5.93909459017002,48.5927940349693,45.8493456756128));
#21702=CARTESIAN_POINT('',(-5.16875607004592,47.6323455307141,44.9925392592695));
#21703=CARTESIAN_POINT('',(-1.41378878846595,56.6580536733786,40.8771032875037));
#21704=CARTESIAN_POINT('Origin',(-1.75639778949586,55.702081474253,39.0146489318449));
#21705=CARTESIAN_POINT('',(-1.75639778949586,55.702081474253,39.0146489318449));
#21706=CARTESIAN_POINT('',(-6.92817584858623,46.4846418874996,44.6972116611125));
#21707=CARTESIAN_POINT('Origin',(-6.92817584858623,46.4846418874996,44.6972116611125));
#21708=CARTESIAN_POINT('',(-6.12611914151519,57.7361776104907,52.0633265742058));
#21709=CARTESIAN_POINT('',(-15.4018995699514,57.0495754343063,54.1220822408886));
#21710=CARTESIAN_POINT('Origin',(-10.230121510861,66.2670150210598,48.4395195116211));
#21711=CARTESIAN_POINT('',(-10.230121510861,66.2670150210598,48.4395195116211));
#21712=CARTESIAN_POINT('Origin',(-10.3946991891447,50.8066601566478,48.5528405346573));
#21713=CARTESIAN_POINT('',(-10.3946991891447,50.8066601566478,48.5528405346573));
#21714=CARTESIAN_POINT('Origin',(-15.4018995699514,57.0495754343063,54.1220822408886));
#21715=CARTESIAN_POINT('Origin',(-40.0919488391595,41.2979694404271,35.1375259990993));
#21716=CARTESIAN_POINT('Ctrl Pts',(-41.7981279794346,37.2631014686576,38.1264711628116));
#21717=CARTESIAN_POINT('Ctrl Pts',(-41.7981279794346,37.2631014686576,38.1264711628116));
#21718=CARTESIAN_POINT('Ctrl Pts',(-41.7981279794346,37.2631014686576,38.1264711628116));
#21719=CARTESIAN_POINT('Ctrl Pts',(-41.7981279794346,37.2631014686576,38.1264711628116));
#21720=CARTESIAN_POINT('Ctrl Pts',(-41.7981279794346,37.2631014686576,38.1264711628116));
#21721=CARTESIAN_POINT('Ctrl Pts',(-41.7981279794346,37.2631014686576,38.1264711628116));
#21722=CARTESIAN_POINT('Ctrl Pts',(-41.7981279794346,37.2631014686576,38.1264711628116));
#21723=CARTESIAN_POINT('Ctrl Pts',(-41.7981279794346,37.2631014686576,38.1264711628116));
#21724=CARTESIAN_POINT('Ctrl Pts',(-41.7981279794346,37.2631014686576,38.1264711628116));
#21725=CARTESIAN_POINT('Ctrl Pts',(-41.7981279794346,37.2631014686576,38.1264711628116));
#21726=CARTESIAN_POINT('Ctrl Pts',(-41.7981279794346,37.2631014686576,38.1264711628116));
#21727=CARTESIAN_POINT('Ctrl Pts',(-41.7981279794346,37.2631014686576,38.1264711628116));
#21728=CARTESIAN_POINT('Ctrl Pts',(-41.7981279794346,37.2631014686576,38.1264711628116));
#21729=CARTESIAN_POINT('Ctrl Pts',(-41.7981279794346,37.2631014686576,38.1264711628116));
#21730=CARTESIAN_POINT('Ctrl Pts',(-41.7981279794346,37.2631014686576,38.1264711628116));
#21731=CARTESIAN_POINT('Ctrl Pts',(-41.7981279794346,37.2631014686576,38.1264711628116));
#21732=CARTESIAN_POINT('Ctrl Pts',(-41.7981279794346,37.2631014686576,38.1264711628116));
#21733=CARTESIAN_POINT('Ctrl Pts',(-41.7981279794346,37.2631014686576,38.1264711628116));
#21734=CARTESIAN_POINT('Ctrl Pts',(-41.7981279794346,37.2631014686576,38.1264711628116));
#21735=CARTESIAN_POINT('Ctrl Pts',(-41.7981279794346,37.2631014686576,38.1264711628116));
#21736=CARTESIAN_POINT('Ctrl Pts',(-41.7981279794346,37.2631014686576,38.1264711628116));
#21737=CARTESIAN_POINT('Ctrl Pts',(-41.7981279794346,37.2631014686576,38.1264711628116));
#21738=CARTESIAN_POINT('Ctrl Pts',(-41.7981279794346,37.2631014686576,38.1264711628116));
#21739=CARTESIAN_POINT('Ctrl Pts',(-41.7981279794346,37.2631014686576,38.1264711628116));
#21740=CARTESIAN_POINT('Ctrl Pts',(-41.7981279794346,37.2631014686576,38.1264711628116));
#21741=CARTESIAN_POINT('Ctrl Pts',(-41.7981279794346,37.2631014686576,38.1264711628116));
#21742=CARTESIAN_POINT('Ctrl Pts',(-41.7981279794346,37.2631014686576,38.1264711628116));
#21743=CARTESIAN_POINT('Ctrl Pts',(-41.7981279794346,37.2631014686576,38.1264711628116));
#21744=CARTESIAN_POINT('Ctrl Pts',(-41.7981279794346,37.2631014686576,38.1264711628116));
#21745=CARTESIAN_POINT('Ctrl Pts',(-41.7981279794346,37.2631014686576,38.1264711628116));
#21746=CARTESIAN_POINT('Ctrl Pts',(-41.7981279794346,37.2631014686576,38.1264711628116));
#21747=CARTESIAN_POINT('Ctrl Pts',(-41.7981279794346,37.2631014686576,38.1264711628116));
#21748=CARTESIAN_POINT('Ctrl Pts',(-41.7981279794346,37.2631014686576,38.1264711628116));
#21749=CARTESIAN_POINT('Ctrl Pts',(-41.7981279794346,37.2631014686576,38.1264711628116));
#21750=CARTESIAN_POINT('Ctrl Pts',(-41.7981279794346,37.2631014686576,38.1264711628116));
#21751=CARTESIAN_POINT('Ctrl Pts',(-41.7981279794346,37.2631014686576,38.1264711628116));
#21752=CARTESIAN_POINT('Ctrl Pts',(-41.7981279794346,37.2631014686576,38.1264711628116));
#21753=CARTESIAN_POINT('Ctrl Pts',(-41.7981279794346,37.2631014686576,38.1264711628116));
#21754=CARTESIAN_POINT('Ctrl Pts',(-41.7981279794346,37.2631014686576,38.1264711628116));
#21755=CARTESIAN_POINT('Ctrl Pts',(-41.7981279794346,37.2631014686576,38.1264711628116));
#21756=CARTESIAN_POINT('Ctrl Pts',(-41.7981279794346,37.2631014686576,38.1264711628116));
#21757=CARTESIAN_POINT('Ctrl Pts',(-41.7981279794346,37.2631014686576,38.1264711628116));
#21758=CARTESIAN_POINT('Ctrl Pts',(-41.7981279794346,37.2631014686576,38.1264711628116));
#21759=CARTESIAN_POINT('Ctrl Pts',(-41.7981279794346,37.2631014686576,38.1264711628116));
#21760=CARTESIAN_POINT('Ctrl Pts',(-41.7981279794346,37.2631014686576,38.1264711628116));
#21761=CARTESIAN_POINT('Ctrl Pts',(-41.7981279794346,37.2631014686576,38.1264711628116));
#21762=CARTESIAN_POINT('Ctrl Pts',(-41.7981279794346,37.2631014686576,38.1264711628116));
#21763=CARTESIAN_POINT('Ctrl Pts',(-41.7981279794346,37.2631014686576,38.1264711628116));
#21764=CARTESIAN_POINT('Ctrl Pts',(-41.7981279794346,37.2631014686576,38.1264711628116));
#21765=CARTESIAN_POINT('Ctrl Pts',(-41.7903142026293,37.2533591778441,38.1177800387672));
#21766=CARTESIAN_POINT('Ctrl Pts',(-41.7904177506121,37.2535524312197,38.1179992662862));
#21767=CARTESIAN_POINT('Ctrl Pts',(-41.790521298595,37.2537456845954,38.1182184938053));
#21768=CARTESIAN_POINT('Ctrl Pts',(-41.7906248465778,37.253938937971,38.1184377213244));
#21769=CARTESIAN_POINT('Ctrl Pts',(-41.7907283026149,37.2541320197466,38.1186567541796));
#21770=CARTESIAN_POINT('Ctrl Pts',(-41.790831758652,37.2543251015223,38.1188757870348));
#21771=CARTESIAN_POINT('Ctrl Pts',(-41.790935214689,37.2545181832979,38.1190948198901));
#21772=CARTESIAN_POINT('Ctrl Pts',(-41.7910386707261,37.2547112650735,38.1193138527453));
#21773=CARTESIAN_POINT('Ctrl Pts',(-41.7911421267631,37.2549043468491,38.1195328856005));
#21774=CARTESIAN_POINT('Ctrl Pts',(-41.7912455828002,37.2550974286247,38.1197519184557));
#21775=CARTESIAN_POINT('Ctrl Pts',(-41.7913490388372,37.2552905104004,38.1199709513109));
#21776=CARTESIAN_POINT('Ctrl Pts',(-41.7914524948743,37.255483592176,38.1201899841661));
#21777=CARTESIAN_POINT('Ctrl Pts',(-41.7915559509113,37.2556766739516,38.1204090170214));
#21778=CARTESIAN_POINT('Ctrl Pts',(-41.7916594069484,37.2558697557272,38.1206280498766));
#21779=CARTESIAN_POINT('Ctrl Pts',(-41.7917628629855,37.2560628375028,38.1208470827318));
#21780=CARTESIAN_POINT('Ctrl Pts',(-41.7918663190225,37.2562559192784,38.121066115587));
#21781=CARTESIAN_POINT('Ctrl Pts',(-41.7919697750596,37.2564490010541,38.1212851484422));
#21782=CARTESIAN_POINT('Ctrl Pts',(-41.7920732310966,37.2566420828297,38.1215041812975));
#21783=CARTESIAN_POINT('Ctrl Pts',(-41.7921766871337,37.2568351646053,38.1217232141527));
#21784=CARTESIAN_POINT('Ctrl Pts',(-41.7922801431707,37.2570282463809,38.1219422470079));
#21785=CARTESIAN_POINT('Ctrl Pts',(-41.7923835992078,37.2572213281565,38.1221612798631));
#21786=CARTESIAN_POINT('Ctrl Pts',(-41.7924870552448,37.2574144099322,38.1223803127183));
#21787=CARTESIAN_POINT('Ctrl Pts',(-41.7925905112819,37.2576074917078,38.1225993455735));
#21788=CARTESIAN_POINT('Ctrl Pts',(-41.792693967319,37.2578005734834,38.1228183784288));
#21789=CARTESIAN_POINT('Ctrl Pts',(-41.792797423356,37.257993655259,38.123037411284));
#21790=CARTESIAN_POINT('Ctrl Pts',(-41.7929008793931,37.2581867370346,38.1232564441392));
#21791=CARTESIAN_POINT('Ctrl Pts',(-41.7930043354301,37.2583798188103,38.1234754769944));
#21792=CARTESIAN_POINT('Ctrl Pts',(-41.7931077914672,37.2585729005859,38.1236945098496));
#21793=CARTESIAN_POINT('Ctrl Pts',(-41.7932112475042,37.2587659823615,38.1239135427048));
#21794=CARTESIAN_POINT('Ctrl Pts',(-41.7933147035413,37.2589590641371,38.1241325755601));
#21795=CARTESIAN_POINT('Ctrl Pts',(-41.7934181595783,37.2591521459127,38.1243516084153));
#21796=CARTESIAN_POINT('Ctrl Pts',(-41.7935216156154,37.2593452276883,38.1245706412705));
#21797=CARTESIAN_POINT('Ctrl Pts',(-41.7936250716524,37.259538309464,38.1247896741257));
#21798=CARTESIAN_POINT('Ctrl Pts',(-41.7937285276895,37.2597313912396,38.1250087069809));
#21799=CARTESIAN_POINT('Ctrl Pts',(-41.7938319837265,37.2599244730152,38.1252277398362));
#21800=CARTESIAN_POINT('Ctrl Pts',(-41.7939354397636,37.2601175547908,38.1254467726914));
#21801=CARTESIAN_POINT('Ctrl Pts',(-41.7940388958007,37.2603106365664,38.1256658055466));
#21802=CARTESIAN_POINT('Ctrl Pts',(-41.7941423518377,37.2605037183421,38.1258848384018));
#21803=CARTESIAN_POINT('Ctrl Pts',(-41.7942458078748,37.2606968001177,38.126103871257));
#21804=CARTESIAN_POINT('Ctrl Pts',(-41.7943492639118,37.2608898818933,38.1263229041122));
#21805=CARTESIAN_POINT('Ctrl Pts',(-41.7944527199489,37.2610829636689,38.1265419369675));
#21806=CARTESIAN_POINT('Ctrl Pts',(-41.7945561759859,37.2612760454445,38.1267609698227));
#21807=CARTESIAN_POINT('Ctrl Pts',(-41.794659632023,37.2614691272201,38.1269800026779));
#21808=CARTESIAN_POINT('Ctrl Pts',(-41.7947630880601,37.2616622089958,38.1271990355331));
#21809=CARTESIAN_POINT('Ctrl Pts',(-41.7948665440971,37.2618552907714,38.1274180683883));
#21810=CARTESIAN_POINT('Ctrl Pts',(-41.7949700001342,37.262048372547,38.1276371012436));
#21811=CARTESIAN_POINT('Ctrl Pts',(-41.7950734561712,37.2622414543226,38.1278561340988));
#21812=CARTESIAN_POINT('Ctrl Pts',(-41.7951769122083,37.2624345360982,38.128075166954));
#21813=CARTESIAN_POINT('Ctrl Pts',(-41.7952803682453,37.2626276178739,38.1282941998092));
#21814=CARTESIAN_POINT('Ctrl Pts',(-41.7821095414117,37.2432764801138,38.1087531709748));
#21815=CARTESIAN_POINT('Ctrl Pts',(-41.7823253824494,37.2436690259226,38.1091992802783));
#21816=CARTESIAN_POINT('Ctrl Pts',(-41.7825411862613,37.2440616379331,38.1096453486643));
#21817=CARTESIAN_POINT('Ctrl Pts',(-41.7827569528505,37.244454316149,38.1100913761369));
#21818=CARTESIAN_POINT('Ctrl Pts',(-41.7829725278491,37.2448466456847,38.1105370075579));
#21819=CARTESIAN_POINT('Ctrl Pts',(-41.783188065691,37.2452390413084,38.1109825981382));
#21820=CARTESIAN_POINT('Ctrl Pts',(-41.7834035663794,37.2456315030234,38.111428147882));
#21821=CARTESIAN_POINT('Ctrl Pts',(-41.7836190670678,37.2460239647385,38.1118736976259));
#21822=CARTESIAN_POINT('Ctrl Pts',(-41.7838345306026,37.246416492545,38.1123192065333));
#21823=CARTESIAN_POINT('Ctrl Pts',(-41.7840499569867,37.2468090864466,38.1127646746086));
#21824=CARTESIAN_POINT('Ctrl Pts',(-41.7842653833709,37.2472016803483,38.1132101426838));
#21825=CARTESIAN_POINT('Ctrl Pts',(-41.7844807726045,37.247594340345,38.1136555699269));
#21826=CARTESIAN_POINT('Ctrl Pts',(-41.7846961246904,37.2479870664405,38.114100956342));
#21827=CARTESIAN_POINT('Ctrl Pts',(-41.7849114767764,37.248379792536,38.1145463427572));
#21828=CARTESIAN_POINT('Ctrl Pts',(-41.7851267917147,37.2487725847303,38.1149916883443));
#21829=CARTESIAN_POINT('Ctrl Pts',(-41.7853420695084,37.2491654430271,38.1154369931077));
#21830=CARTESIAN_POINT('Ctrl Pts',(-41.7855573473021,37.2495583013238,38.1158822978712));
#21831=CARTESIAN_POINT('Ctrl Pts',(-41.7857725879511,37.2499512257232,38.1163275618108));
#21832=CARTESIAN_POINT('Ctrl Pts',(-41.7859877914583,37.2503442162287,38.1167727849309));
#21833=CARTESIAN_POINT('Ctrl Pts',(-41.7862029949656,37.2507372067343,38.117218008051));
#21834=CARTESIAN_POINT('Ctrl Pts',(-41.7864181613311,37.251130263346,38.1176631903516));
#21835=CARTESIAN_POINT('Ctrl Pts',(-41.7866332905579,37.2515233860677,38.1181083318368));
#21836=CARTESIAN_POINT('Ctrl Pts',(-41.7868484197847,37.2519165087895,38.1185534733219));
#21837=CARTESIAN_POINT('Ctrl Pts',(-41.7870635118726,37.2523096976213,38.1189985739917));
#21838=CARTESIAN_POINT('Ctrl Pts',(-41.7872785668247,37.2527029525669,38.1194436338503));
#21839=CARTESIAN_POINT('Ctrl Pts',(-41.7874936217768,37.2530962075124,38.1198886937088));
#21840=CARTESIAN_POINT('Ctrl Pts',(-41.787708639593,37.2534895285718,38.1203337127562));
#21841=CARTESIAN_POINT('Ctrl Pts',(-41.7879236202762,37.2538829157488,38.1207786909964));
#21842=CARTESIAN_POINT('Ctrl Pts',(-41.7881386009594,37.2542763029258,38.1212236692367));
#21843=CARTESIAN_POINT('Ctrl Pts',(-41.7883535445096,37.2546697562204,38.1216686066698));
#21844=CARTESIAN_POINT('Ctrl Pts',(-41.7885684509297,37.2550632756365,38.1221135033));
#21845=CARTESIAN_POINT('Ctrl Pts',(-41.7887833573499,37.2554567950526,38.1225583999302));
#21846=CARTESIAN_POINT('Ctrl Pts',(-41.7889982266399,37.2558503805902,38.1230032557575));
#21847=CARTESIAN_POINT('Ctrl Pts',(-41.7892130588027,37.2562440322531,38.1234480707859));
#21848=CARTESIAN_POINT('Ctrl Pts',(-41.7894278909654,37.2566376839161,38.1238928858142));
#21849=CARTESIAN_POINT('Ctrl Pts',(-41.789642686001,37.2570314017044,38.1243376600438));
#21850=CARTESIAN_POINT('Ctrl Pts',(-41.7898574439121,37.2574251856219,38.1247823934785));
#21851=CARTESIAN_POINT('Ctrl Pts',(-41.7900722018233,37.2578189695394,38.1252271269133));
#21852=CARTESIAN_POINT('Ctrl Pts',(-41.79028692261,37.2582128195863,38.1256718195533));
#21853=CARTESIAN_POINT('Ctrl Pts',(-41.7905016062752,37.2586067357663,38.1261164714026));
#21854=CARTESIAN_POINT('Ctrl Pts',(-41.7907162899404,37.2590006519463,38.1265611232519));
#21855=CARTESIAN_POINT('Ctrl Pts',(-41.7909309364841,37.2593946342595,38.1270057343105));
#21856=CARTESIAN_POINT('Ctrl Pts',(-41.791145545909,37.2597886827099,38.1274503045824));
#21857=CARTESIAN_POINT('Ctrl Pts',(-41.7913601553339,37.2601827311602,38.1278948748544));
#21858=CARTESIAN_POINT('Ctrl Pts',(-41.7915747276401,37.2605768457478,38.1283394043397));
#21859=CARTESIAN_POINT('Ctrl Pts',(-41.7917892628303,37.2609710264765,38.1287838930424));
#21860=CARTESIAN_POINT('Ctrl Pts',(-41.7920037980206,37.2613652072052,38.1292283817452));
#21861=CARTESIAN_POINT('Ctrl Pts',(-41.7922182960949,37.2617594540751,38.1296728296653));
#21862=CARTESIAN_POINT('Ctrl Pts',(-41.7924327570561,37.2621537670901,38.1301172368068));
#21863=CARTESIAN_POINT('Ctrl Pts',(-41.7734797039072,37.2328485512714,38.0993780694756));
#21864=CARTESIAN_POINT('Ctrl Pts',(-41.7738174367737,37.2334462429607,38.1000591182637));
#21865=CARTESIAN_POINT('Ctrl Pts',(-41.7741550496373,37.2340441517543,38.100740036031));
#21866=CARTESIAN_POINT('Ctrl Pts',(-41.7744925424411,37.2346422775518,38.1014208226628));
#21867=CARTESIAN_POINT('Ctrl Pts',(-41.7748297355669,37.2352398722414,38.1021010047876));
#21868=CARTESIAN_POINT('Ctrl Pts',(-41.775166808846,37.2358376835495,38.1027810560098));
#21869=CARTESIAN_POINT('Ctrl Pts',(-41.7755037622217,37.2364357113757,38.103460976215));
#21870=CARTESIAN_POINT('Ctrl Pts',(-41.7758407155975,37.2370337392019,38.1041408964203));
#21871=CARTESIAN_POINT('Ctrl Pts',(-41.7761775490699,37.2376319835463,38.1048206856085));
#21872=CARTESIAN_POINT('Ctrl Pts',(-41.7765142625823,37.2382304443082,38.1055003436656));
#21873=CARTESIAN_POINT('Ctrl Pts',(-41.7768509760948,37.2388289050702,38.1061800017226));
#21874=CARTESIAN_POINT('Ctrl Pts',(-41.7771875696473,37.2394275822497,38.1068595286485));
#21875=CARTESIAN_POINT('Ctrl Pts',(-41.7775240431833,37.2400264757463,38.1075389243291));
#21876=CARTESIAN_POINT('Ctrl Pts',(-41.7778605167192,37.2406253692429,38.1082183200096));
#21877=CARTESIAN_POINT('Ctrl Pts',(-41.7781968702387,37.2412244790565,38.1088975844447));
#21878=CARTESIAN_POINT('Ctrl Pts',(-41.7785331036852,37.2418238050864,38.1095767175204));
#21879=CARTESIAN_POINT('Ctrl Pts',(-41.7788693371317,37.2424231311163,38.1102558505961));
#21880=CARTESIAN_POINT('Ctrl Pts',(-41.7792054505051,37.2430226733626,38.1109348523123));
#21881=CARTESIAN_POINT('Ctrl Pts',(-41.7795414437491,37.2436224317244,38.1116137225549));
#21882=CARTESIAN_POINT('Ctrl Pts',(-41.779877436993,37.2442221900863,38.1122925927975));
#21883=CARTESIAN_POINT('Ctrl Pts',(-41.7802133101075,37.2448221645638,38.1129713315665));
#21884=CARTESIAN_POINT('Ctrl Pts',(-41.7805490630361,37.245422355056,38.113649938748));
#21885=CARTESIAN_POINT('Ctrl Pts',(-41.7808848159646,37.2460225455484,38.1143285459293));
#21886=CARTESIAN_POINT('Ctrl Pts',(-41.7812204487072,37.2466229520555,38.1150070215231));
#21887=CARTESIAN_POINT('Ctrl Pts',(-41.7815559612075,37.2472235744765,38.1156853654153));
#21888=CARTESIAN_POINT('Ctrl Pts',(-41.7818914737078,37.2478241968974,38.1163637093074));
#21889=CARTESIAN_POINT('Ctrl Pts',(-41.7822268659657,37.2484250352323,38.117041921498));
#21890=CARTESIAN_POINT('Ctrl Pts',(-41.782562137925,37.2490260893802,38.1177200018729));
#21891=CARTESIAN_POINT('Ctrl Pts',(-41.7828974098843,37.2496271435281,38.1183980822478));
#21892=CARTESIAN_POINT('Ctrl Pts',(-41.7832325615449,37.250228413489,38.1190760308072));
#21893=CARTESIAN_POINT('Ctrl Pts',(-41.7835675928505,37.2508298991617,38.1197538474371));
#21894=CARTESIAN_POINT('Ctrl Pts',(-41.7839026241561,37.2514313848345,38.120431664067));
#21895=CARTESIAN_POINT('Ctrl Pts',(-41.7842375351068,37.2520330862192,38.1211093487674));
#21896=CARTESIAN_POINT('Ctrl Pts',(-41.7845723256461,37.2526350032147,38.1217869014244));
#21897=CARTESIAN_POINT('Ctrl Pts',(-41.7849071161855,37.2532369202102,38.1224644540814));
#21898=CARTESIAN_POINT('Ctrl Pts',(-41.7852417863136,37.2538390528166,38.1231418746951));
#21899=CARTESIAN_POINT('Ctrl Pts',(-41.7855763359742,37.2544414009326,38.1238191631516));
#21900=CARTESIAN_POINT('Ctrl Pts',(-41.7859108856348,37.2550437490486,38.1244964516081));
#21901=CARTESIAN_POINT('Ctrl Pts',(-41.7862453148279,37.2556463126744,38.1251736079073));
#21902=CARTESIAN_POINT('Ctrl Pts',(-41.7865796234973,37.2562490917085,38.1258506319357));
#21903=CARTESIAN_POINT('Ctrl Pts',(-41.7869139321667,37.2568518707426,38.126527655964));
#21904=CARTESIAN_POINT('Ctrl Pts',(-41.7872481203125,37.257454865185,38.1272045477214));
#21905=CARTESIAN_POINT('Ctrl Pts',(-41.7875821878784,37.2580580749346,38.1278813070941));
#21906=CARTESIAN_POINT('Ctrl Pts',(-41.7879162554443,37.2586612846843,38.1285580664668));
#21907=CARTESIAN_POINT('Ctrl Pts',(-41.7882502024303,37.259264709741,38.1292346934548));
#21908=CARTESIAN_POINT('Ctrl Pts',(-41.7885840287804,37.2598683500034,38.1299111879444));
#21909=CARTESIAN_POINT('Ctrl Pts',(-41.7889178551305,37.2604719902658,38.130587682434));
#21910=CARTESIAN_POINT('Ctrl Pts',(-41.7892515608447,37.2610758457339,38.1312640444252));
#21911=CARTESIAN_POINT('Ctrl Pts',(-41.7895851458668,37.2616799163063,38.1319402738044));
#21912=CARTESIAN_POINT('Ctrl Pts',(-41.771322244531,37.2302415690607,38.0970342941008));
#21913=CARTESIAN_POINT('Ctrl Pts',(-41.7716904503549,37.2308905472201,38.0977740777601));
#21914=CARTESIAN_POINT('Ctrl Pts',(-41.7720585154814,37.2315397802096,38.0985137078727));
#21915=CARTESIAN_POINT('Ctrl Pts',(-41.7724264398387,37.2321892679025,38.0992531842943));
#21916=CARTESIAN_POINT('Ctrl Pts',(-41.7727940374963,37.2328381788805,38.0999920040951));
#21917=CARTESIAN_POINT('Ctrl Pts',(-41.7731614946347,37.2334873441097,38.1007306704778));
#21918=CARTESIAN_POINT('Ctrl Pts',(-41.7735288111823,37.2341367634638,38.1014691832983));
#21919=CARTESIAN_POINT('Ctrl Pts',(-41.7738961277299,37.2347861828177,38.1022076961189));
#21920=CARTESIAN_POINT('Ctrl Pts',(-41.7742633036867,37.2354358562966,38.1029460553773));
#21921=CARTESIAN_POINT('Ctrl Pts',(-41.7746303389812,37.2360857837736,38.1036842609298));
#21922=CARTESIAN_POINT('Ctrl Pts',(-41.7749973742757,37.2367357112507,38.1044224664823));
#21923=CARTESIAN_POINT('Ctrl Pts',(-41.7753642689079,37.2373858927259,38.1051605183289));
#21924=CARTESIAN_POINT('Ctrl Pts',(-41.7757310228065,37.2380363280728,38.1058984163258));
#21925=CARTESIAN_POINT('Ctrl Pts',(-41.776097776705,37.2386867634196,38.1066363143227));
#21926=CARTESIAN_POINT('Ctrl Pts',(-41.7764643898697,37.239337452638,38.1073740584699));
#21927=CARTESIAN_POINT('Ctrl Pts',(-41.7768308622294,37.2399883956012,38.1081116486236));
#21928=CARTESIAN_POINT('Ctrl Pts',(-41.7771973345891,37.2406393385644,38.1088492387774));
#21929=CARTESIAN_POINT('Ctrl Pts',(-41.7775636661437,37.2412905352724,38.1095866749377));
#21930=CARTESIAN_POINT('Ctrl Pts',(-41.7779298568218,37.2419419855984,38.1103239569609));
#21931=CARTESIAN_POINT('Ctrl Pts',(-41.7782960474999,37.2425934359243,38.1110612389841));
#21932=CARTESIAN_POINT('Ctrl Pts',(-41.7786620973016,37.2432451398683,38.1117983668703));
#21933=CARTESIAN_POINT('Ctrl Pts',(-41.7790280061556,37.2438970973032,38.1125353404757));
#21934=CARTESIAN_POINT('Ctrl Pts',(-41.7793939150096,37.2445490547381,38.1132723140812));
#21935=CARTESIAN_POINT('Ctrl Pts',(-41.7797596829158,37.245201265664,38.114009133406));
#21936=CARTESIAN_POINT('Ctrl Pts',(-41.7801253098032,37.2458537299538,38.1147457983065));
#21937=CARTESIAN_POINT('Ctrl Pts',(-41.7804909366905,37.2465061942437,38.1154824632071));
#21938=CARTESIAN_POINT('Ctrl Pts',(-41.7808564225589,37.2471589118975,38.1162189736834));
#21939=CARTESIAN_POINT('Ctrl Pts',(-41.7812217673372,37.247811882788,38.1169553295921));
#21940=CARTESIAN_POINT('Ctrl Pts',(-41.7815871121155,37.2484648536787,38.1176916855007));
#21941=CARTESIAN_POINT('Ctrl Pts',(-41.7819523158038,37.249118077806,38.1184278868416));
#21942=CARTESIAN_POINT('Ctrl Pts',(-41.7823173783307,37.249771555043,38.1191639334714));
#21943=CARTESIAN_POINT('Ctrl Pts',(-41.7826824408577,37.2504250322799,38.1198999801012));
#21944=CARTESIAN_POINT('Ctrl Pts',(-41.7830473622235,37.2510787626264,38.1206358720198));
#21945=CARTESIAN_POINT('Ctrl Pts',(-41.783412142357,37.2517327459551,38.121371609084));
#21946=CARTESIAN_POINT('Ctrl Pts',(-41.7837769224905,37.2523867292838,38.1221073461482));
#21947=CARTESIAN_POINT('Ctrl Pts',(-41.7841415613918,37.2530409655946,38.1228429283579));
#21948=CARTESIAN_POINT('Ctrl Pts',(-41.7845060589897,37.2536954547603,38.1235783555698));
#21949=CARTESIAN_POINT('Ctrl Pts',(-41.7848705565877,37.254349943926,38.1243137827817));
#21950=CARTESIAN_POINT('Ctrl Pts',(-41.7852349128824,37.2550046859463,38.1250490549959));
#21951=CARTESIAN_POINT('Ctrl Pts',(-41.7855991278029,37.255659680694,38.125784172069));
#21952=CARTESIAN_POINT('Ctrl Pts',(-41.7859633427234,37.2563146754416,38.1265192891421));
#21953=CARTESIAN_POINT('Ctrl Pts',(-41.7863274162696,37.2569699229165,38.1272542510741));
#21954=CARTESIAN_POINT('Ctrl Pts',(-41.7866913483708,37.2576254229908,38.127989057722));
#21955=CARTESIAN_POINT('Ctrl Pts',(-41.7870552804719,37.2582809230653,38.1287238643699));
#21956=CARTESIAN_POINT('Ctrl Pts',(-41.7874190711279,37.2589366757393,38.1294585157335));
#21957=CARTESIAN_POINT('Ctrl Pts',(-41.787782720268,37.2595926808851,38.1301930116699));
#21958=CARTESIAN_POINT('Ctrl Pts',(-41.788146369408,37.260248686031,38.1309275076062));
#21959=CARTESIAN_POINT('Ctrl Pts',(-41.7885098770322,37.2609049436486,38.1316618481152));
#21960=CARTESIAN_POINT('Ctrl Pts',(-41.7888732430695,37.2615614536103,38.1323960330538));
#21961=CARTESIAN_POINT('Ctrl Pts',(-41.7691382140772,37.2276131212637,38.0946687739682));
#21962=CARTESIAN_POINT('Ctrl Pts',(-41.7695374927977,37.2283137491982,38.095467795755));
#21963=CARTESIAN_POINT('Ctrl Pts',(-41.7699366072763,37.2290146749967,38.0962666383926));
#21964=CARTESIAN_POINT('Ctrl Pts',(-41.7703355574223,37.2297158984997,38.097065301699));
#21965=CARTESIAN_POINT('Ctrl Pts',(-41.770734153319,37.2304164993487,38.0978632558295));
#21966=CARTESIAN_POINT('Ctrl Pts',(-41.7711325851747,37.2311173973738,38.0986610309469));
#21967=CARTESIAN_POINT('Ctrl Pts',(-41.7715308528989,37.2318185924153,38.0994586268701));
#21968=CARTESIAN_POINT('Ctrl Pts',(-41.7719291206231,37.2325197874568,38.1002562227932));
#21969=CARTESIAN_POINT('Ctrl Pts',(-41.7723272242156,37.2332212795149,38.1010536395219));
#21970=CARTESIAN_POINT('Ctrl Pts',(-41.7727251635862,37.2339230684298,38.1018508768749));
#21971=CARTESIAN_POINT('Ctrl Pts',(-41.7731231029567,37.2346248573449,38.1026481142279));
#21972=CARTESIAN_POINT('Ctrl Pts',(-41.7735208781052,37.2353269431168,38.1034451722051));
#21973=CARTESIAN_POINT('Ctrl Pts',(-41.7739184889412,37.236029325586,38.1042420506252));
#21974=CARTESIAN_POINT('Ctrl Pts',(-41.7743160997773,37.2367317080551,38.1050389290454));
#21975=CARTESIAN_POINT('Ctrl Pts',(-41.7747135463009,37.2374343872215,38.1058356279085));
#21976=CARTESIAN_POINT('Ctrl Pts',(-41.7751108284216,37.2381373629254,38.1066321470333));
#21977=CARTESIAN_POINT('Ctrl Pts',(-41.7755081105424,37.2388403386292,38.1074286661581));
#21978=CARTESIAN_POINT('Ctrl Pts',(-41.7759052282603,37.2395436108705,38.1082250055445));
#21979=CARTESIAN_POINT('Ctrl Pts',(-41.7763021814853,37.2402471794891,38.1090211650117));
#21980=CARTESIAN_POINT('Ctrl Pts',(-41.7766991347102,37.2409507481079,38.1098173244787));
#21981=CARTESIAN_POINT('Ctrl Pts',(-41.777095923442,37.241654613104,38.1106133040264));
#21982=CARTESIAN_POINT('Ctrl Pts',(-41.7774925475906,37.2423587743175,38.1114091034736));
#21983=CARTESIAN_POINT('Ctrl Pts',(-41.7778891717392,37.2430629355309,38.1122049029208));
#21984=CARTESIAN_POINT('Ctrl Pts',(-41.7782856313045,37.2437673929618,38.1130005222675));
#21985=CARTESIAN_POINT('Ctrl Pts',(-41.7786819261965,37.2444721464497,38.1137959613327));
#21986=CARTESIAN_POINT('Ctrl Pts',(-41.7790782210884,37.2451768999376,38.114591400398));
#21987=CARTESIAN_POINT('Ctrl Pts',(-41.7794743513071,37.2458819494826,38.1153866591818));
#21988=CARTESIAN_POINT('Ctrl Pts',(-41.7798703167622,37.2465872949244,38.1161817375032));
#21989=CARTESIAN_POINT('Ctrl Pts',(-41.7802662822174,37.2472926403662,38.1169768158246));
#21990=CARTESIAN_POINT('Ctrl Pts',(-41.7806620829091,37.2479982817048,38.1177717136837));
#21991=CARTESIAN_POINT('Ctrl Pts',(-41.7810577187476,37.2487042187795,38.1185664308996));
#21992=CARTESIAN_POINT('Ctrl Pts',(-41.7814533545859,37.2494101558543,38.1193611481155));
#21993=CARTESIAN_POINT('Ctrl Pts',(-41.7818488255709,37.2501163886654,38.1201556846882));
#21994=CARTESIAN_POINT('Ctrl Pts',(-41.7822441316126,37.250822917052,38.1209500404371));
#21995=CARTESIAN_POINT('Ctrl Pts',(-41.7826394376543,37.2515294454386,38.1217443961859));
#21996=CARTESIAN_POINT('Ctrl Pts',(-41.7830345787528,37.2522362694009,38.1225385711109));
#21997=CARTESIAN_POINT('Ctrl Pts',(-41.7834295548181,37.252943388778,38.1233325650312));
#21998=CARTESIAN_POINT('Ctrl Pts',(-41.7838245308834,37.2536505081552,38.1241265589516));
#21999=CARTESIAN_POINT('Ctrl Pts',(-41.7842193419157,37.2543579229471,38.1249203718674));
#22000=CARTESIAN_POINT('Ctrl Pts',(-41.7846139878251,37.255065632993,38.1257140035981));
#22001=CARTESIAN_POINT('Ctrl Pts',(-41.7850086337345,37.255773343039,38.1265076353288));
#22002=CARTESIAN_POINT('Ctrl Pts',(-41.785403114521,37.2564813483389,38.1273010858744));
#22003=CARTESIAN_POINT('Ctrl Pts',(-41.785797430095,37.2571896487317,38.1280943550543));
#22004=CARTESIAN_POINT('Ctrl Pts',(-41.7861917456691,37.2578979491245,38.1288876242342));
#22005=CARTESIAN_POINT('Ctrl Pts',(-41.7865858960306,37.2586065446103,38.1296807120485));
#22006=CARTESIAN_POINT('Ctrl Pts',(-41.78697988109,37.2593154350278,38.1304736183168));
#22007=CARTESIAN_POINT('Ctrl Pts',(-41.7873738661493,37.2600243254453,38.1312665245851));
#22008=CARTESIAN_POINT('Ctrl Pts',(-41.7877676859066,37.2607335107946,38.1320592493073));
#22009=CARTESIAN_POINT('Ctrl Pts',(-41.7881613402722,37.2614429909144,38.1328517923032));
#22010=CARTESIAN_POINT('Ctrl Pts',(-41.766927213444,37.2249631469137,38.0922814953632));
#22011=CARTESIAN_POINT('Ctrl Pts',(-41.7673581756058,37.2257157843197,38.0931402611643));
#22012=CARTESIAN_POINT('Ctrl Pts',(-41.7677889469959,37.2264687682492,38.0939988190038));
#22013=CARTESIAN_POINT('Ctrl Pts',(-41.7682195274985,37.2272220985005,38.0948571686514));
#22014=CARTESIAN_POINT('Ctrl Pts',(-41.7686497256657,37.2279747598295,38.0957147561243));
#22015=CARTESIAN_POINT('Ctrl Pts',(-41.7690797332845,37.2287277668655,38.0965721357748));
#22016=CARTESIAN_POINT('Ctrl Pts',(-41.7695095502396,37.2294811194068,38.0974293073736));
#22017=CARTESIAN_POINT('Ctrl Pts',(-41.7699393671947,37.2302344719482,38.0982864789723));
#22018=CARTESIAN_POINT('Ctrl Pts',(-41.7703689934863,37.2309881699949,38.0991434425192));
#22019=CARTESIAN_POINT('Ctrl Pts',(-41.7707984289993,37.2317422133453,38.1000001977849));
#22020=CARTESIAN_POINT('Ctrl Pts',(-41.7712278645123,37.2324962566957,38.1008569530506));
#22021=CARTESIAN_POINT('Ctrl Pts',(-41.7716571092468,37.2332506453498,38.101713500035));
#22022=CARTESIAN_POINT('Ctrl Pts',(-41.7720861630878,37.2340053791055,38.102569838509));
#22023=CARTESIAN_POINT('Ctrl Pts',(-41.7725152169288,37.2347601128614,38.103426176983));
#22024=CARTESIAN_POINT('Ctrl Pts',(-41.7729440798763,37.2355151917189,38.1042823069466));
#22025=CARTESIAN_POINT('Ctrl Pts',(-41.7733727518156,37.236270615476,38.1051382281704));
#22026=CARTESIAN_POINT('Ctrl Pts',(-41.7738014237548,37.2370260392332,38.1059941493943));
#22027=CARTESIAN_POINT('Ctrl Pts',(-41.7742299046859,37.23778180789,38.1068498618786));
#22028=CARTESIAN_POINT('Ctrl Pts',(-41.774658194494,37.2385379212441,38.1077053653942));
#22029=CARTESIAN_POINT('Ctrl Pts',(-41.775086484302,37.2392940345982,38.1085608689097));
#22030=CARTESIAN_POINT('Ctrl Pts',(-41.7755145829872,37.2400504926497,38.1094161634566));
#22031=CARTESIAN_POINT('Ctrl Pts',(-41.7759424904348,37.240807295196,38.1102712488059));
#22032=CARTESIAN_POINT('Ctrl Pts',(-41.7763703978824,37.2415640977423,38.1111263341552));
#22033=CARTESIAN_POINT('Ctrl Pts',(-41.7767981140925,37.2423212447835,38.1119812103068));
#22034=CARTESIAN_POINT('Ctrl Pts',(-41.7772256389506,37.2430787361169,38.1128358770321));
#22035=CARTESIAN_POINT('Ctrl Pts',(-41.7776531638086,37.2438362274503,38.1136905437573));
#22036=CARTESIAN_POINT('Ctrl Pts',(-41.7780804973147,37.2445940630758,38.1145450010561));
#22037=CARTESIAN_POINT('Ctrl Pts',(-41.7785076393544,37.2453522427908,38.1153992486998));
#22038=CARTESIAN_POINT('Ctrl Pts',(-41.7789347813941,37.2461104225057,38.1162534963434));
#22039=CARTESIAN_POINT('Ctrl Pts',(-41.7793617319673,37.24686894631,38.117107534332));
#22040=CARTESIAN_POINT('Ctrl Pts',(-41.7797884909599,37.2476278140006,38.1179613624368));
#22041=CARTESIAN_POINT('Ctrl Pts',(-41.7802152499525,37.2483866816912,38.1188151905415));
#22042=CARTESIAN_POINT('Ctrl Pts',(-41.7806418173644,37.2491458932681,38.1196688087626));
#22043=CARTESIAN_POINT('Ctrl Pts',(-41.7810681930815,37.2499054485281,38.1205222168715));
#22044=CARTESIAN_POINT('Ctrl Pts',(-41.7814945687986,37.2506650037881,38.1213756249803));
#22045=CARTESIAN_POINT('Ctrl Pts',(-41.7819207528208,37.2514249027313,38.122228822977));
#22046=CARTESIAN_POINT('Ctrl Pts',(-41.7823467450341,37.2521851451541,38.123081810633));
#22047=CARTESIAN_POINT('Ctrl Pts',(-41.7827727372475,37.2529453875769,38.123934798289));
#22048=CARTESIAN_POINT('Ctrl Pts',(-41.7831985376518,37.2537059734796,38.1247875756044));
#22049=CARTESIAN_POINT('Ctrl Pts',(-41.7836241461333,37.2544669026582,38.125640142351));
#22050=CARTESIAN_POINT('Ctrl Pts',(-41.7840497546148,37.2552278318368,38.1264927090977));
#22051=CARTESIAN_POINT('Ctrl Pts',(-41.7844751711734,37.2559891042917,38.1273450652754));
#22052=CARTESIAN_POINT('Ctrl Pts',(-41.7849003956952,37.2567507198189,38.1281972106561));
#22053=CARTESIAN_POINT('Ctrl Pts',(-41.785325620217,37.257512335346,38.1290493560369));
#22054=CARTESIAN_POINT('Ctrl Pts',(-41.7857506527021,37.2582742939455,38.1299012906207));
#22055=CARTESIAN_POINT('Ctrl Pts',(-41.7861754930366,37.2590365954135,38.1307530141794));
#22056=CARTESIAN_POINT('Ctrl Pts',(-41.7866003333711,37.2597988968814,38.1316047377382));
#22057=CARTESIAN_POINT('Ctrl Pts',(-41.7870249815551,37.2605615412178,38.1324562502719));
#22058=CARTESIAN_POINT('Ctrl Pts',(-41.7874494374749,37.2613245282184,38.1333075515526));
#22059=CARTESIAN_POINT('Ctrl Pts',(-41.7658217131275,37.2236381597387,38.0910878560607));
#22060=CARTESIAN_POINT('Ctrl Pts',(-41.7662685170099,37.2244168018805,38.091976493869));
#22061=CARTESIAN_POINT('Ctrl Pts',(-41.7667151168556,37.2251958148755,38.0928649093094));
#22062=CARTESIAN_POINT('Ctrl Pts',(-41.7671615125367,37.2259751985009,38.0937531021275));
#22063=CARTESIAN_POINT('Ctrl Pts',(-41.7676075118391,37.2267538900699,38.0946405062717));
#22064=CARTESIAN_POINT('Ctrl Pts',(-41.7680533073393,37.2275329516114,38.0955276881887));
#22065=CARTESIAN_POINT('Ctrl Pts',(-41.76849889891,37.2283123829026,38.0964146476253));
#22066=CARTESIAN_POINT('Ctrl Pts',(-41.7689444904806,37.2290918141938,38.0973016070618));
#22067=CARTESIAN_POINT('Ctrl Pts',(-41.7693898781217,37.2298716152349,38.0981883440178));
#22068=CARTESIAN_POINT('Ctrl Pts',(-41.7698350617059,37.230651785803,38.0990748582399));
#22069=CARTESIAN_POINT('Ctrl Pts',(-41.7702802452902,37.2314319563711,38.0999613724619));
#22070=CARTESIAN_POINT('Ctrl Pts',(-41.7707252248176,37.2322124964663,38.10084766395));
#22071=CARTESIAN_POINT('Ctrl Pts',(-41.771170000161,37.2329934058654,38.1017337324509));
#22072=CARTESIAN_POINT('Ctrl Pts',(-41.7716147755045,37.2337743152645,38.1026198009518));
#22073=CARTESIAN_POINT('Ctrl Pts',(-41.772059346664,37.2345555939675,38.1035056464656));
#22074=CARTESIAN_POINT('Ctrl Pts',(-41.7725037135125,37.2353372417514,38.104391268739));
#22075=CARTESIAN_POINT('Ctrl Pts',(-41.7729480803611,37.2361188895352,38.1052768910125));
#22076=CARTESIAN_POINT('Ctrl Pts',(-41.7733922428986,37.2369009063998,38.1061622900455));
#22077=CARTESIAN_POINT('Ctrl Pts',(-41.7738362009983,37.2376832921216,38.1070474655853));
#22078=CARTESIAN_POINT('Ctrl Pts',(-41.774280159098,37.2384656778434,38.1079326411252));
#22079=CARTESIAN_POINT('Ctrl Pts',(-41.7747239127597,37.2392484324226,38.1088175931717));
#22080=CARTESIAN_POINT('Ctrl Pts',(-41.7751674618569,37.2400315556353,38.109702321472));
#22081=CARTESIAN_POINT('Ctrl Pts',(-41.775611010954,37.2408146788481,38.1105870497723));
#22082=CARTESIAN_POINT('Ctrl Pts',(-41.7760543554865,37.2415981706944,38.1114715543265));
#22083=CARTESIAN_POINT('Ctrl Pts',(-41.7764974953276,37.2423820309506,38.1123558348817));
#22084=CARTESIAN_POINT('Ctrl Pts',(-41.7769406351687,37.2431658912066,38.113240115437));
#22085=CARTESIAN_POINT('Ctrl Pts',(-41.7773835703185,37.2439501198725,38.1141241719933));
#22086=CARTESIAN_POINT('Ctrl Pts',(-41.7778263006504,37.244734716724,38.1150080042981));
#22087=CARTESIAN_POINT('Ctrl Pts',(-41.7782690309824,37.2455193135755,38.1158918366028));
#22088=CARTESIAN_POINT('Ctrl Pts',(-41.7787115564964,37.2463042786126,38.1167754446561));
#22089=CARTESIAN_POINT('Ctrl Pts',(-41.7791538770661,37.2470896116111,38.1176588282053));
#22090=CARTESIAN_POINT('Ctrl Pts',(-41.7795961976358,37.2478749446096,38.1185422117546));
#22091=CARTESIAN_POINT('Ctrl Pts',(-41.7800383132612,37.2486606455695,38.1194253707998));
#22092=CARTESIAN_POINT('Ctrl Pts',(-41.780480223816,37.2494467142662,38.1203083050887));
#22093=CARTESIAN_POINT('Ctrl Pts',(-41.7809221343707,37.2502327829629,38.1211912393775));
#22094=CARTESIAN_POINT('Ctrl Pts',(-41.7813638398548,37.2510192193965,38.1220739489099));
#22095=CARTESIAN_POINT('Ctrl Pts',(-41.7818053401422,37.2518060233422,38.1229564334338));
#22096=CARTESIAN_POINT('Ctrl Pts',(-41.7822468404294,37.2525928272879,38.1238389179577));
#22097=CARTESIAN_POINT('Ctrl Pts',(-41.7826881355199,37.2533799987457,38.124721177473));
#22098=CARTESIAN_POINT('Ctrl Pts',(-41.7831292252874,37.2541675374908,38.1256032117275));
#22099=CARTESIAN_POINT('Ctrl Pts',(-41.7835703150549,37.2549550762359,38.1264852459821));
#22100=CARTESIAN_POINT('Ctrl Pts',(-41.7840111994995,37.2557429822681,38.1273670549759));
#22101=CARTESIAN_POINT('Ctrl Pts',(-41.7844518784953,37.2565312553624,38.1282486384571));
#22102=CARTESIAN_POINT('Ctrl Pts',(-41.784892557491,37.2573195284568,38.1291302219383));
#22103=CARTESIAN_POINT('Ctrl Pts',(-41.7853330310378,37.2581081686132,38.1300115799068));
#22104=CARTESIAN_POINT('Ctrl Pts',(-41.7857732990099,37.2588971756064,38.1308927121107));
#22105=CARTESIAN_POINT('Ctrl Pts',(-41.786213566982,37.2596861825995,38.1317738443147));
#22106=CARTESIAN_POINT('Ctrl Pts',(-41.7866536293793,37.2604755564294,38.1326547507541));
#22107=CARTESIAN_POINT('Ctrl Pts',(-41.7870934860762,37.2612652968705,38.1335354311773));
#22108=CARTESIAN_POINT('Ctrl Pts',(-41.7647094275776,37.222307870463,38.089888730797));
#22109=CARTESIAN_POINT('Ctrl Pts',(-41.7651722267075,37.2231126056039,38.0908073680508));
#22110=CARTESIAN_POINT('Ctrl Pts',(-41.7656348077892,37.2239177373345,38.091725767728));
#22111=CARTESIAN_POINT('Ctrl Pts',(-41.7660971706813,37.2247232654083,38.0926439295475));
#22112=CARTESIAN_POINT('Ctrl Pts',(-41.7665591230165,37.2255280782106,38.093561276082));
#22113=CARTESIAN_POINT('Ctrl Pts',(-41.7670208575494,37.2263332866526,38.0944783851809));
#22114=CARTESIAN_POINT('Ctrl Pts',(-41.7674823741388,37.2271388904882,38.0953952565644));
#22115=CARTESIAN_POINT('Ctrl Pts',(-41.7679438907283,37.2279444943239,38.0963121279478));
#22116=CARTESIAN_POINT('Ctrl Pts',(-41.7684051893743,37.2287504935532,38.0972287616156));
#22117=CARTESIAN_POINT('Ctrl Pts',(-41.7688662699361,37.2295568879302,38.0981451572879));
#22118=CARTESIAN_POINT('Ctrl Pts',(-41.7693273504978,37.2303632823071,38.0990615529601));
#22119=CARTESIAN_POINT('Ctrl Pts',(-41.7697882129753,37.2311700718315,38.0999777106368));
#22120=CARTESIAN_POINT('Ctrl Pts',(-41.7702488572277,37.231977256257,38.1008936300381));
#22121=CARTESIAN_POINT('Ctrl Pts',(-41.7707095014801,37.2327844406825,38.1018095494393));
#22122=CARTESIAN_POINT('Ctrl Pts',(-41.7711699275075,37.2335920200091,38.1027252305651));
#22123=CARTESIAN_POINT('Ctrl Pts',(-41.7716301351692,37.2343999939901,38.1036406731358));
#22124=CARTESIAN_POINT('Ctrl Pts',(-41.7720903428309,37.235207967971,38.1045561157065));
#22125=CARTESIAN_POINT('Ctrl Pts',(-41.7725503321269,37.2360163366064,38.105471319722));
#22126=CARTESIAN_POINT('Ctrl Pts',(-41.7730101029167,37.2368250996492,38.1063862849029));
#22127=CARTESIAN_POINT('Ctrl Pts',(-41.7734698737066,37.237633862692,38.1073012500838));
#22128=CARTESIAN_POINT('Ctrl Pts',(-41.7739294259903,37.2384430201423,38.1082159764299));
#22129=CARTESIAN_POINT('Ctrl Pts',(-41.7743887596274,37.2392525717529,38.1091304636619));
#22130=CARTESIAN_POINT('Ctrl Pts',(-41.7748480932646,37.2400621233635,38.110044950894));
#22131=CARTESIAN_POINT('Ctrl Pts',(-41.7753072082553,37.2408720691344,38.1109591990119));
#22132=CARTESIAN_POINT('Ctrl Pts',(-41.7757661044592,37.2416824088182,38.1118732077365));
#22133=CARTESIAN_POINT('Ctrl Pts',(-41.7762250006631,37.242492748502,38.1127872164611));
#22134=CARTESIAN_POINT('Ctrl Pts',(-41.7766836780803,37.2433034820986,38.1137009857923));
#22135=CARTESIAN_POINT('Ctrl Pts',(-41.7771421365706,37.2441146093606,38.1146145154509));
#22136=CARTESIAN_POINT('Ctrl Pts',(-41.7776005950609,37.2449257366225,38.1155280451096));
#22137=CARTESIAN_POINT('Ctrl Pts',(-41.7780588346244,37.2457372575497,38.1164413350958));
#22138=CARTESIAN_POINT('Ctrl Pts',(-41.7785168551212,37.2465491718942,38.1173543851306));
#22139=CARTESIAN_POINT('Ctrl Pts',(-41.7789748756179,37.2473610862387,38.1182674351653));
#22140=CARTESIAN_POINT('Ctrl Pts',(-41.7794326770479,37.2481733940007,38.1191802452485));
#22141=CARTESIAN_POINT('Ctrl Pts',(-41.7798902592712,37.2489860949319,38.1200928151015));
#22142=CARTESIAN_POINT('Ctrl Pts',(-41.7803478414945,37.249798795863,38.1210053849544));
#22143=CARTESIAN_POINT('Ctrl Pts',(-41.7808052045112,37.2506118899634,38.1219177145771));
#22144=CARTESIAN_POINT('Ctrl Pts',(-41.7812623481816,37.2514253769846,38.1228298036907));
#22145=CARTESIAN_POINT('Ctrl Pts',(-41.7817194918521,37.2522388640059,38.1237418928044));
#22146=CARTESIAN_POINT('Ctrl Pts',(-41.7821764161762,37.2530527439481,38.124653741409));
#22147=CARTESIAN_POINT('Ctrl Pts',(-41.7826331210144,37.2538670165625,38.1255653492261));
#22148=CARTESIAN_POINT('Ctrl Pts',(-41.7830898258527,37.2546812891769,38.1264769570433));
#22149=CARTESIAN_POINT('Ctrl Pts',(-41.7835463112051,37.2554959544635,38.1273883240729));
#22150=CARTESIAN_POINT('Ctrl Pts',(-41.7840025769323,37.2563110121736,38.1282994500366));
#22151=CARTESIAN_POINT('Ctrl Pts',(-41.7844588426594,37.2571260698838,38.1292105760003));
#22152=CARTESIAN_POINT('Ctrl Pts',(-41.7849148887613,37.2579415200173,38.1301214608981));
#22153=CARTESIAN_POINT('Ctrl Pts',(-41.7853707150985,37.2587573623252,38.1310321044517));
#22154=CARTESIAN_POINT('Ctrl Pts',(-41.7858265414359,37.259573204633,38.1319427480054));
#22155=CARTESIAN_POINT('Ctrl Pts',(-41.7862821480086,37.2603894391152,38.1328531502148));
#22156=CARTESIAN_POINT('Ctrl Pts',(-41.7867375346776,37.2612060655225,38.133763310802));
#22157=CARTESIAN_POINT('Ctrl Pts',(-41.7635903731375,37.2209721633598,38.0886841910433));
#22158=CARTESIAN_POINT('Ctrl Pts',(-41.7640693209891,37.221803081553,38.0896329539864));
#22159=CARTESIAN_POINT('Ctrl Pts',(-41.7645480360178,37.2226344235192,38.090581463325));
#22160=CARTESIAN_POINT('Ctrl Pts',(-41.7650265180668,37.223466188986,38.0915297187483));
#22161=CARTESIAN_POINT('Ctrl Pts',(-41.7655045752459,37.2242972158836,38.0924771321649));
#22162=CARTESIAN_POINT('Ctrl Pts',(-41.7659823998588,37.2251286655302,38.0934242921168));
#22163=CARTESIAN_POINT('Ctrl Pts',(-41.7664599917494,37.2259605376537,38.0943711982946));
#22164=CARTESIAN_POINT('Ctrl Pts',(-41.7669375836398,37.2267924097772,38.0953181044724));
#22165=CARTESIAN_POINT('Ctrl Pts',(-41.7674149428079,37.2276247043777,38.0962647568759));
#22166=CARTESIAN_POINT('Ctrl Pts',(-41.7678920690975,37.228457421183,38.0972111551956));
#22167=CARTESIAN_POINT('Ctrl Pts',(-41.768369195387,37.2292901379882,38.0981575535153));
#22168=CARTESIAN_POINT('Ctrl Pts',(-41.768846088798,37.2301232769982,38.0991036977512));
#22169=CARTESIAN_POINT('Ctrl Pts',(-41.7693227491746,37.2309568379406,38.1000495875938));
#22170=CARTESIAN_POINT('Ctrl Pts',(-41.7697994095511,37.231790398883,38.1009954774365));
#22171=CARTESIAN_POINT('Ctrl Pts',(-41.7702758368932,37.2326243817577,38.1019411128859));
#22172=CARTESIAN_POINT('Ctrl Pts',(-41.7707520310449,37.2334587862921,38.1028864936329));
#22173=CARTESIAN_POINT('Ctrl Pts',(-41.7712282251966,37.2342931908265,38.1038318743798));
#22174=CARTESIAN_POINT('Ctrl Pts',(-41.7717041861582,37.2351280170204,38.1047770004243));
#22175=CARTESIAN_POINT('Ctrl Pts',(-41.7721799137737,37.235963264601,38.1057218714573));
#22176=CARTESIAN_POINT('Ctrl Pts',(-41.7726556413892,37.2367985121816,38.1066667424903));
#22177=CARTESIAN_POINT('Ctrl Pts',(-41.7731311356589,37.2376341811488,38.1076113585118));
#22178=CARTESIAN_POINT('Ctrl Pts',(-41.7736063964271,37.2384702712294,38.1085557192128));
#22179=CARTESIAN_POINT('Ctrl Pts',(-41.7740816571953,37.23930636131,38.1095000799138));
#22180=CARTESIAN_POINT('Ctrl Pts',(-41.774556684462,37.2401428725039,38.1104441852944));
#22181=CARTESIAN_POINT('Ctrl Pts',(-41.7750314780721,37.2409798045376,38.1113880350459));
#22182=CARTESIAN_POINT('Ctrl Pts',(-41.7755062716821,37.2418167365713,38.1123318847973));
#22183=CARTESIAN_POINT('Ctrl Pts',(-41.7759808316353,37.2426540894449,38.1132754789196));
#22184=CARTESIAN_POINT('Ctrl Pts',(-41.7764551577767,37.2434918628844,38.1142188171042));
#22185=CARTESIAN_POINT('Ctrl Pts',(-41.776929483918,37.2443296363239,38.1151621552887));
#22186=CARTESIAN_POINT('Ctrl Pts',(-41.7774035762474,37.2451678303293,38.1161052375356));
#22187=CARTESIAN_POINT('Ctrl Pts',(-41.7778774346097,37.2460064446267,38.1170480635362));
#22188=CARTESIAN_POINT('Ctrl Pts',(-41.7783512929721,37.246845058924,38.117990889537));
#22189=CARTESIAN_POINT('Ctrl Pts',(-41.7788249173675,37.2476840935132,38.1189334592915));
#22190=CARTESIAN_POINT('Ctrl Pts',(-41.7792983076411,37.24852354812,38.1198757724917));
#22191=CARTESIAN_POINT('Ctrl Pts',(-41.7797716979146,37.2493630027266,38.120818085692));
#22192=CARTESIAN_POINT('Ctrl Pts',(-41.7802448540663,37.2502028773509,38.1217601423378));
#22193=CARTESIAN_POINT('Ctrl Pts',(-41.7807177759414,37.251043171718,38.1227019421212));
#22194=CARTESIAN_POINT('Ctrl Pts',(-41.7811906978165,37.251883466085,38.1236437419047));
#22195=CARTESIAN_POINT('Ctrl Pts',(-41.781663385415,37.2527241801949,38.1245852848257));
#22196=CARTESIAN_POINT('Ctrl Pts',(-41.7821358385823,37.2535653137728,38.1255265705763));
#22197=CARTESIAN_POINT('Ctrl Pts',(-41.7826082917497,37.2544064473506,38.126467856327));
#22198=CARTESIAN_POINT('Ctrl Pts',(-41.7830805104859,37.2552480003964,38.1274088849074));
#22199=CARTESIAN_POINT('Ctrl Pts',(-41.7835524946364,37.2560899726349,38.1283496560097));
#22200=CARTESIAN_POINT('Ctrl Pts',(-41.784024478787,37.2569319448734,38.1292904271121));
#22201=CARTESIAN_POINT('Ctrl Pts',(-41.784496228352,37.2577743363046,38.1302309407363));
#22202=CARTESIAN_POINT('Ctrl Pts',(-41.7849677431772,37.2586171466531,38.131171196575));
#22203=CARTESIAN_POINT('Ctrl Pts',(-41.7854392580023,37.2594599570016,38.1321114524136));
#22204=CARTESIAN_POINT('Ctrl Pts',(-41.7859105380876,37.2603031862673,38.1330514504667));
#22205=CARTESIAN_POINT('Ctrl Pts',(-41.7863815832789,37.2611468341745,38.1339911904267));
#22206=CARTESIAN_POINT('Ctrl Pts',(-41.7624713186973,37.2196364562566,38.0874796512896));
#22207=CARTESIAN_POINT('Ctrl Pts',(-41.7629664152707,37.2204935575021,38.088458539922));
#22208=CARTESIAN_POINT('Ctrl Pts',(-41.7634612642464,37.2213511097039,38.089437158922));
#22209=CARTESIAN_POINT('Ctrl Pts',(-41.7639558654523,37.2222091125637,38.0904155079491));
#22210=CARTESIAN_POINT('Ctrl Pts',(-41.7644500274753,37.2230663535568,38.0913929882477));
#22211=CARTESIAN_POINT('Ctrl Pts',(-41.7649439421683,37.2239240444079,38.0923701990528));
#22212=CARTESIAN_POINT('Ctrl Pts',(-41.7654376093599,37.2247821848192,38.0933471400249));
#22213=CARTESIAN_POINT('Ctrl Pts',(-41.7659312765514,37.2256403252306,38.094324080997));
#22214=CARTESIAN_POINT('Ctrl Pts',(-41.7664246962416,37.2264989152021,38.0953007521362));
#22215=CARTESIAN_POINT('Ctrl Pts',(-41.7669178682589,37.2273579544356,38.0962771531033));
#22216=CARTESIAN_POINT('Ctrl Pts',(-41.7674110402762,37.2282169936692,38.0972535540705));
#22217=CARTESIAN_POINT('Ctrl Pts',(-41.7679039646208,37.2290764821649,38.0982296848655));
#22218=CARTESIAN_POINT('Ctrl Pts',(-41.7683966411214,37.2299364196242,38.0992055451495));
#22219=CARTESIAN_POINT('Ctrl Pts',(-41.7688893176221,37.2307963570835,38.1001814054336));
#22220=CARTESIAN_POINT('Ctrl Pts',(-41.7693817462788,37.2316567435063,38.1011569952067));
#22221=CARTESIAN_POINT('Ctrl Pts',(-41.7698739269206,37.2325175785941,38.1021323141299));
#22222=CARTESIAN_POINT('Ctrl Pts',(-41.7703661075624,37.2333784136818,38.1031076330531));
#22223=CARTESIAN_POINT('Ctrl Pts',(-41.7708580401894,37.2342396974344,38.1040826811266));
#22224=CARTESIAN_POINT('Ctrl Pts',(-41.7713497246306,37.2351014295528,38.1050574580117));
#22225=CARTESIAN_POINT('Ctrl Pts',(-41.7718414090719,37.2359631616712,38.1060322348969));
#22226=CARTESIAN_POINT('Ctrl Pts',(-41.7723328453274,37.2368253421553,38.1070067405936));
#22227=CARTESIAN_POINT('Ctrl Pts',(-41.7728240332267,37.2376879707059,38.1079809747636));
#22228=CARTESIAN_POINT('Ctrl Pts',(-41.7733152211259,37.2385505992564,38.1089552089337));
#22229=CARTESIAN_POINT('Ctrl Pts',(-41.7738061606688,37.2394136758734,38.1099291715769));
#22230=CARTESIAN_POINT('Ctrl Pts',(-41.774296851685,37.240277200257,38.1109028623553));
#22231=CARTESIAN_POINT('Ctrl Pts',(-41.7747875427011,37.2411407246407,38.1118765531336));
#22232=CARTESIAN_POINT('Ctrl Pts',(-41.7752779851904,37.242004696791,38.112849972047));
#22233=CARTESIAN_POINT('Ctrl Pts',(-41.7757681789827,37.2428691164081,38.1138231187574));
#22234=CARTESIAN_POINT('Ctrl Pts',(-41.776258372775,37.2437335360252,38.1147962654678));
#22235=CARTESIAN_POINT('Ctrl Pts',(-41.7767483178702,37.244598403109,38.1157691399753));
#22236=CARTESIAN_POINT('Ctrl Pts',(-41.7772380140983,37.2454637173591,38.1167417419419));
#22237=CARTESIAN_POINT('Ctrl Pts',(-41.7777277103263,37.2463290316093,38.1177143439086));
#22238=CARTESIAN_POINT('Ctrl Pts',(-41.7782171576872,37.2471947930257,38.1186866733346));
#22239=CARTESIAN_POINT('Ctrl Pts',(-41.778706356011,37.2480610013081,38.119658729882));
#22240=CARTESIAN_POINT('Ctrl Pts',(-41.7791955543347,37.2489272095904,38.1206307864295));
#22241=CARTESIAN_POINT('Ctrl Pts',(-41.7796845036214,37.2497938647384,38.1216025700986));
#22242=CARTESIAN_POINT('Ctrl Pts',(-41.7801732037012,37.2506609664512,38.1225740805518));
#22243=CARTESIAN_POINT('Ctrl Pts',(-41.7806619037809,37.2515280681641,38.123545591005));
#22244=CARTESIAN_POINT('Ctrl Pts',(-41.7811503546538,37.2523956164418,38.1245168282424));
#22245=CARTESIAN_POINT('Ctrl Pts',(-41.7816385561502,37.2532636109831,38.1254877919266));
#22246=CARTESIAN_POINT('Ctrl Pts',(-41.7821267576466,37.2541316055244,38.1264587556108));
#22247=CARTESIAN_POINT('Ctrl Pts',(-41.7826147097666,37.2550000463293,38.1274294457419));
#22248=CARTESIAN_POINT('Ctrl Pts',(-41.7831024123406,37.2558689330961,38.1283998619829));
#22249=CARTESIAN_POINT('Ctrl Pts',(-41.7835901149147,37.256737819863,38.1293702782238));
#22250=CARTESIAN_POINT('Ctrl Pts',(-41.7840775679428,37.2576071525919,38.1303404205745));
#22251=CARTESIAN_POINT('Ctrl Pts',(-41.7845647712558,37.258476930981,38.1313102886982));
#22252=CARTESIAN_POINT('Ctrl Pts',(-41.7850519745688,37.25934670937,38.1322801568219));
#22253=CARTESIAN_POINT('Ctrl Pts',(-41.7855389281667,37.2602169334193,38.1332497507186));
#22254=CARTESIAN_POINT('Ctrl Pts',(-41.7860256318803,37.2610876028265,38.1342190700514));
#22255=CARTESIAN_POINT('Ctrl Pts',(-41.7613770641789,37.2183331411396,38.0863036281828));
#22256=CARTESIAN_POINT('Ctrl Pts',(-41.7618876562635,37.2192157760948,38.0873122441619));
#22257=CARTESIAN_POINT('Ctrl Pts',(-41.7623979856072,37.2200988899049,38.0883205740934));
#22258=CARTESIAN_POINT('Ctrl Pts',(-41.7629080520215,37.2209824822438,38.0893286176052));
#22259=CARTESIAN_POINT('Ctrl Pts',(-41.7634176655205,37.2218652899938,38.0903357660211));
#22260=CARTESIAN_POINT('Ctrl Pts',(-41.7639270165568,37.222748575423,38.0913426285256));
#22261=CARTESIAN_POINT('Ctrl Pts',(-41.7644361049428,37.223632338206,38.0923492047476));
#22262=CARTESIAN_POINT('Ctrl Pts',(-41.7649451933288,37.224516100989,38.0933557809696));
#22263=CARTESIAN_POINT('Ctrl Pts',(-41.7654540190643,37.2254003411258,38.0943620709091));
#22264=CARTESIAN_POINT('Ctrl Pts',(-41.765962581962,37.2262850582903,38.0953680741951));
#22265=CARTESIAN_POINT('Ctrl Pts',(-41.7664711448597,37.2271697754548,38.0963740774812));
#22266=CARTESIAN_POINT('Ctrl Pts',(-41.7669794449194,37.2280549696471,38.0973797941137));
#22267=CARTESIAN_POINT('Ctrl Pts',(-41.7674874819539,37.2289406405409,38.0983852237221));
#22268=CARTESIAN_POINT('Ctrl Pts',(-41.7679955189883,37.2298263114347,38.0993906533304));
#22269=CARTESIAN_POINT('Ctrl Pts',(-41.7685032929975,37.2307124590299,38.1003957959146));
#22270=CARTESIAN_POINT('Ctrl Pts',(-41.7690108037943,37.231599083,38.1014006511041));
#22271=CARTESIAN_POINT('Ctrl Pts',(-41.7695183145911,37.2324857069701,38.1024055062937));
#22272=CARTESIAN_POINT('Ctrl Pts',(-41.7700255621754,37.233372807315,38.1034100740885));
#22273=CARTESIAN_POINT('Ctrl Pts',(-41.7705325463604,37.2342603837078,38.1044143541183));
#22274=CARTESIAN_POINT('Ctrl Pts',(-41.7710395305453,37.2351479601006,38.1054186341482));
#22275=CARTESIAN_POINT('Ctrl Pts',(-41.7715462513308,37.2360360125412,38.106422626413));
#22276=CARTESIAN_POINT('Ctrl Pts',(-41.7720527085303,37.2369245407023,38.1074263305428));
#22277=CARTESIAN_POINT('Ctrl Pts',(-41.7725591657296,37.2378130688634,38.1084300346726));
#22278=CARTESIAN_POINT('Ctrl Pts',(-41.7730653593429,37.238702072745,38.1094334506673));
#22279=CARTESIAN_POINT('Ctrl Pts',(-41.7735712891834,37.2395915520194,38.110436578157));
#22280=CARTESIAN_POINT('Ctrl Pts',(-41.7740772190239,37.2404810312937,38.1114397056469));
#22281=CARTESIAN_POINT('Ctrl Pts',(-41.7745828850917,37.2413709859609,38.1124425446317));
#22282=CARTESIAN_POINT('Ctrl Pts',(-41.7750882872003,37.2422614156928,38.1134450947419));
#22283=CARTESIAN_POINT('Ctrl Pts',(-41.775593689309,37.2431518454246,38.1144476448522));
#22284=CARTESIAN_POINT('Ctrl Pts',(-41.7760988274585,37.2440427502213,38.1154499060878));
#22285=CARTESIAN_POINT('Ctrl Pts',(-41.7766037014628,37.2449341297543,38.1164518780793));
#22286=CARTESIAN_POINT('Ctrl Pts',(-41.777108575467,37.2458255092872,38.1174538500709));
#22287=CARTESIAN_POINT('Ctrl Pts',(-41.777613185326,37.2467173635565,38.1184555328185));
#22288=CARTESIAN_POINT('Ctrl Pts',(-41.7781175308536,37.2476096922334,38.1194569259527));
#22289=CARTESIAN_POINT('Ctrl Pts',(-41.7786218763813,37.2485020209103,38.1204583190869));
#22290=CARTESIAN_POINT('Ctrl Pts',(-41.7791259575776,37.2493948239948,38.1214594226079));
#22291=CARTESIAN_POINT('Ctrl Pts',(-41.7796297742569,37.2502881011577,38.1224602361465));
#22292=CARTESIAN_POINT('Ctrl Pts',(-41.7801335909362,37.2511813783207,38.1234610496852));
#22293=CARTESIAN_POINT('Ctrl Pts',(-41.7806371430984,37.2520751295621,38.1244615732415));
#22294=CARTESIAN_POINT('Ctrl Pts',(-41.7811404305579,37.2529693545526,38.1254618064468));
#22295=CARTESIAN_POINT('Ctrl Pts',(-41.7816437180174,37.2538635795431,38.126462039652));
#22296=CARTESIAN_POINT('Ctrl Pts',(-41.7821467407742,37.2547582782826,38.1274619825061));
#22297=CARTESIAN_POINT('Ctrl Pts',(-41.7826494986429,37.2556534504414,38.1284616346405));
#22298=CARTESIAN_POINT('Ctrl Pts',(-41.7831522565116,37.2565486226002,38.1294612867749));
#22299=CARTESIAN_POINT('Ctrl Pts',(-41.7836547494923,37.2574442681782,38.1304606481896));
#22300=CARTESIAN_POINT('Ctrl Pts',(-41.7841569773996,37.2583403868454,38.1314597185161));
#22301=CARTESIAN_POINT('Ctrl Pts',(-41.7846592053069,37.2592365055125,38.1324587888427));
#22302=CARTESIAN_POINT('Ctrl Pts',(-41.7851611681409,37.2601330972687,38.1334575680812));
#22303=CARTESIAN_POINT('Ctrl Pts',(-41.7856628657165,37.2610301617836,38.1344560558635));
#22304=CARTESIAN_POINT('Ctrl Pts',(-41.7602656007636,37.217011975673,38.0851109242317));
#22305=CARTESIAN_POINT('Ctrl Pts',(-41.760792130705,37.2179204777448,38.0861495472797));
#22306=CARTESIAN_POINT('Ctrl Pts',(-41.7613183818872,37.2188294882312,38.0871878669253));
#22307=CARTESIAN_POINT('Ctrl Pts',(-41.7618443541036,37.2197390067751,38.088225882761));
#22308=CARTESIAN_POINT('Ctrl Pts',(-41.7623698592811,37.2206477177089,38.0892629768868));
#22309=CARTESIAN_POINT('Ctrl Pts',(-41.7628950859879,37.2215569357985,38.0902997677418));
#22310=CARTESIAN_POINT('Ctrl Pts',(-41.7634200340183,37.2224666606875,38.0913362549198));
#22311=CARTESIAN_POINT('Ctrl Pts',(-41.7639449820487,37.2233763855765,38.0923727420979));
#22312=CARTESIAN_POINT('Ctrl Pts',(-41.7644696514026,37.224286617265,38.0934089255988));
#22313=CARTESIAN_POINT('Ctrl Pts',(-41.7649940418743,37.2251973553961,38.0944448050165));
#22314=CARTESIAN_POINT('Ctrl Pts',(-41.7655184323462,37.2261080935271,38.0954806844343));
#22315=CARTESIAN_POINT('Ctrl Pts',(-41.7660425439358,37.2270193381009,38.0965162597688));
#22316=CARTESIAN_POINT('Ctrl Pts',(-41.7665663764379,37.2279310887602,38.0975515306143));
#22317=CARTESIAN_POINT('Ctrl Pts',(-41.76709020894,37.2288428394195,38.0985868014598));
#22318=CARTESIAN_POINT('Ctrl Pts',(-41.7676137623545,37.2297550961644,38.0996217678161));
#22319=CARTESIAN_POINT('Ctrl Pts',(-41.7681370364763,37.2306678586371,38.1006564292777));
#22320=CARTESIAN_POINT('Ctrl Pts',(-41.7686603105981,37.2315806211098,38.1016910907394));
#22321=CARTESIAN_POINT('Ctrl Pts',(-41.7691833054271,37.2324938893106,38.1027254473063));
#22322=CARTESIAN_POINT('Ctrl Pts',(-41.7697060207585,37.2334076628813,38.1037594985731));
#22323=CARTESIAN_POINT('Ctrl Pts',(-41.7702287360898,37.234321436452,38.1047935498398));
#22324=CARTESIAN_POINT('Ctrl Pts',(-41.7707511719234,37.2352357153927,38.1058272958065));
#22325=CARTESIAN_POINT('Ctrl Pts',(-41.7712733280544,37.2361504993452,38.1068607360678));
#22326=CARTESIAN_POINT('Ctrl Pts',(-41.7717954841855,37.2370652832975,38.1078941763291));
#22327=CARTESIAN_POINT('Ctrl Pts',(-41.772317360614,37.2379805722616,38.1089273108851));
#22328=CARTESIAN_POINT('Ctrl Pts',(-41.7728389571356,37.2388963658785,38.1099601393308));
#22329=CARTESIAN_POINT('Ctrl Pts',(-41.7733605536571,37.2398121594955,38.1109929677765));
#22330=CARTESIAN_POINT('Ctrl Pts',(-41.7738818702715,37.2407284577654,38.112025490112));
#22331=CARTESIAN_POINT('Ctrl Pts',(-41.7744029067746,37.241645260329,38.1130577059326));
#22332=CARTESIAN_POINT('Ctrl Pts',(-41.7749239432777,37.2425620628927,38.1140899217531));
#22333=CARTESIAN_POINT('Ctrl Pts',(-41.7754446996694,37.2434793697501,38.1151218310587));
#22334=CARTESIAN_POINT('Ctrl Pts',(-41.7759651757456,37.2443971805418,38.1161534334449));
#22335=CARTESIAN_POINT('Ctrl Pts',(-41.7764856518219,37.2453149913334,38.1171850358311));
#22336=CARTESIAN_POINT('Ctrl Pts',(-41.7770058475826,37.2462333060593,38.1182163312979));
#22337=CARTESIAN_POINT('Ctrl Pts',(-41.7775257628239,37.2471521243595,38.1192473194412));
#22338=CARTESIAN_POINT('Ctrl Pts',(-41.7780456780652,37.2480709426598,38.1202783075843));
#22339=CARTESIAN_POINT('Ctrl Pts',(-41.7785653127873,37.2489902645343,38.1213089884039));
#22340=CARTESIAN_POINT('Ctrl Pts',(-41.7790846667862,37.2499100896229,38.1223393614959));
#22341=CARTESIAN_POINT('Ctrl Pts',(-41.7796040207851,37.2508299147114,38.123369734588));
#22342=CARTESIAN_POINT('Ctrl Pts',(-41.780123094061,37.2517502430139,38.1243997999524));
#22343=CARTESIAN_POINT('Ctrl Pts',(-41.7806418864104,37.2526710741697,38.1254295571855));
#22344=CARTESIAN_POINT('Ctrl Pts',(-41.7811606787598,37.2535919053255,38.1264593144186));
#22345=CARTESIAN_POINT('Ctrl Pts',(-41.7816791901827,37.2545132393345,38.1274887635205));
#22346=CARTESIAN_POINT('Ctrl Pts',(-41.7821974204759,37.2554350758357,38.1285179040875));
#22347=CARTESIAN_POINT('Ctrl Pts',(-41.782715650769,37.2563569123369,38.1295470446545));
#22348=CARTESIAN_POINT('Ctrl Pts',(-41.7832335999325,37.2572792513303,38.1305758766868));
#22349=CARTESIAN_POINT('Ctrl Pts',(-41.7837512677633,37.2582020924543,38.131604399781));
#22350=CARTESIAN_POINT('Ctrl Pts',(-41.784268935594,37.2591249335783,38.1326329228752));
#22351=CARTESIAN_POINT('Ctrl Pts',(-41.784786322092,37.260048276833,38.1336611370313));
#22352=CARTESIAN_POINT('Ctrl Pts',(-41.7853034270545,37.2609721218564,38.1346890418465));
#22353=CARTESIAN_POINT('Ctrl Pts',(-41.7558197471023,37.2117273138067,38.0803401084276));
#22354=CARTESIAN_POINT('Ctrl Pts',(-41.7564100284709,37.2127392843447,38.0814987597511));
#22355=CARTESIAN_POINT('Ctrl Pts',(-41.7569999670072,37.213751881536,38.082657038253));
#22356=CARTESIAN_POINT('Ctrl Pts',(-41.7575895624321,37.2147651049003,38.0838149433843));
#22357=CARTESIAN_POINT('Ctrl Pts',(-41.7581786343235,37.2157774285695,38.0849718203494));
#22358=CARTESIAN_POINT('Ctrl Pts',(-41.7587673637124,37.2167903773003,38.0861283246066));
#22359=CARTESIAN_POINT('Ctrl Pts',(-41.7593557503204,37.2178039506134,38.0872844556087));
#22360=CARTESIAN_POINT('Ctrl Pts',(-41.7599441369285,37.2188175239264,38.0884405866107));
#22361=CARTESIAN_POINT('Ctrl Pts',(-41.7605321807556,37.2198317218217,38.0895963443575));
#22362=CARTESIAN_POINT('Ctrl Pts',(-41.7611198815238,37.2208465438191,38.0907517283021));
#22363=CARTESIAN_POINT('Ctrl Pts',(-41.761707582292,37.2218613658167,38.0919071122468));
#22364=CARTESIAN_POINT('Ctrl Pts',(-41.7622949400013,37.2228768119163,38.0930621223893));
#22365=CARTESIAN_POINT('Ctrl Pts',(-41.7628819543739,37.2238928816376,38.0942167581831));
#22366=CARTESIAN_POINT('Ctrl Pts',(-41.7634689687465,37.224908951359,38.0953713939769));
#22367=CARTESIAN_POINT('Ctrl Pts',(-41.7640556397825,37.225925644702,38.096525655422));
#22368=CARTESIAN_POINT('Ctrl Pts',(-41.7646419672044,37.2269429611854,38.0976795419723));
#22369=CARTESIAN_POINT('Ctrl Pts',(-41.7652282946264,37.2279602776687,38.0988334285225));
#22370=CARTESIAN_POINT('Ctrl Pts',(-41.7658142784342,37.2289782172926,38.0999869401777));
#22371=CARTESIAN_POINT('Ctrl Pts',(-41.766399918351,37.2299967795751,38.1011400763922));
#22372=CARTESIAN_POINT('Ctrl Pts',(-41.7669855582677,37.2310153418577,38.1022932126067));
#22373=CARTESIAN_POINT('Ctrl Pts',(-41.7675708542934,37.2320345267988,38.1034459733804));
#22374=CARTESIAN_POINT('Ctrl Pts',(-41.7681558061512,37.2330543339164,38.1045983581678));
#22375=CARTESIAN_POINT('Ctrl Pts',(-41.7687407580089,37.234074141034,38.1057507429551));
#22376=CARTESIAN_POINT('Ctrl Pts',(-41.7693253656987,37.2350945703279,38.1069027517562));
#22377=CARTESIAN_POINT('Ctrl Pts',(-41.7699096289443,37.2361156213152,38.1080543840258));
#22378=CARTESIAN_POINT('Ctrl Pts',(-41.7704938921898,37.2371366723026,38.1092060162953));
#22379=CARTESIAN_POINT('Ctrl Pts',(-41.771077810991,37.2381583449833,38.1103572720334));
#22380=CARTESIAN_POINT('Ctrl Pts',(-41.7716613850718,37.2391806388741,38.1115081506952));
#22381=CARTESIAN_POINT('Ctrl Pts',(-41.7722449591525,37.2402029327648,38.112659029357));
#22382=CARTESIAN_POINT('Ctrl Pts',(-41.7728281885128,37.2412258478655,38.1138095309424));
#22383=CARTESIAN_POINT('Ctrl Pts',(-41.773411072877,37.2422493836919,38.1149596549072));
#22384=CARTESIAN_POINT('Ctrl Pts',(-41.773993957241,37.2432729195185,38.1161097788719));
#22385=CARTESIAN_POINT('Ctrl Pts',(-41.7745764966089,37.2442970760708,38.1172595252158));
#22386=CARTESIAN_POINT('Ctrl Pts',(-41.775158690705,37.2453218528644,38.1184088933949));
#22387=CARTESIAN_POINT('Ctrl Pts',(-41.7757408848011,37.246346629658,38.1195582615739));
#22388=CARTESIAN_POINT('Ctrl Pts',(-41.7763227336255,37.2473720266928,38.120707251588));
#22389=CARTESIAN_POINT('Ctrl Pts',(-41.7769042369031,37.2483980434835,38.1218558628935));
#22390=CARTESIAN_POINT('Ctrl Pts',(-41.7774857401807,37.2494240602743,38.123004474199));
#22391=CARTESIAN_POINT('Ctrl Pts',(-41.7780668979113,37.2504506968211,38.1241527067959));
#22392=CARTESIAN_POINT('Ctrl Pts',(-41.7786477098203,37.251477952638,38.1253005601407));
#22393=CARTESIAN_POINT('Ctrl Pts',(-41.7792285217293,37.2525052084549,38.1264484134854));
#22394=CARTESIAN_POINT('Ctrl Pts',(-41.7798089878166,37.253533083542,38.1275958875781));
#22395=CARTESIAN_POINT('Ctrl Pts',(-41.7803891078076,37.254561577413,38.1287429818757));
#22396=CARTESIAN_POINT('Ctrl Pts',(-41.7809692277987,37.2555900712838,38.1298900761733));
#22397=CARTESIAN_POINT('Ctrl Pts',(-41.7815490016936,37.2566191839385,38.1310367906757));
#22398=CARTESIAN_POINT('Ctrl Pts',(-41.782128429218,37.2576489148901,38.1321831248404));
#22399=CARTESIAN_POINT('Ctrl Pts',(-41.7827078567425,37.2586786458416,38.133329459005));
#22400=CARTESIAN_POINT('Ctrl Pts',(-41.7832869378965,37.2597089950899,38.1344754128318));
#22401=CARTESIAN_POINT('Ctrl Pts',(-41.7838656724063,37.2607399621476,38.1356209857784));
#22402=CARTESIAN_POINT('Ctrl Pts',(-41.7513111929665,37.2064115906167,38.0755313098334));
#22403=CARTESIAN_POINT('Ctrl Pts',(-41.751966757934,37.2075273833708,38.0768110311642));
#22404=CARTESIAN_POINT('Ctrl Pts',(-41.7526219045242,37.208643942912,38.0780902979841));
#22405=CARTESIAN_POINT('Ctrl Pts',(-41.7532766323584,37.2097612685937,38.0793691095526));
#22406=CARTESIAN_POINT('Ctrl Pts',(-41.7539307788246,37.210877602142,38.0806467855958));
#22407=CARTESIAN_POINT('Ctrl Pts',(-41.754584507278,37.2119947004709,38.0819240071957));
#22408=CARTESIAN_POINT('Ctrl Pts',(-41.7552378173414,37.2131125629345,38.0832007736143));
#22409=CARTESIAN_POINT('Ctrl Pts',(-41.7558911274048,37.2142304253979,38.0844775400328));
#22410=CARTESIAN_POINT('Ctrl Pts',(-41.7565440190782,37.2153490519962,38.08575385127));
#22411=CARTESIAN_POINT('Ctrl Pts',(-41.7571964919848,37.2164684420825,38.0870297065882));
#22412=CARTESIAN_POINT('Ctrl Pts',(-41.7578489648914,37.2175878321687,38.0883055619064));
#22413=CARTESIAN_POINT('Ctrl Pts',(-41.7585010190312,37.218707985743,38.0895809613056));
#22414=CARTESIAN_POINT('Ctrl Pts',(-41.7591526540278,37.2198289021578,38.0908559040488));
#22415=CARTESIAN_POINT('Ctrl Pts',(-41.7598042890245,37.2209498185725,38.0921308467919));
#22416=CARTESIAN_POINT('Ctrl Pts',(-41.760455504878,37.2220714978278,38.0934053328791));
#22417=CARTESIAN_POINT('Ctrl Pts',(-41.7611063012126,37.2231939392752,38.0946793615737));
#22418=CARTESIAN_POINT('Ctrl Pts',(-41.7617570975472,37.2243163807225,38.0959533902682));
#22419=CARTESIAN_POINT('Ctrl Pts',(-41.7624074743628,37.225439584362,38.0972269615702));
#22420=CARTESIAN_POINT('Ctrl Pts',(-41.763057431284,37.2265635495444,38.0985000747435));
#22421=CARTESIAN_POINT('Ctrl Pts',(-41.7637073882053,37.2276875147267,38.0997731879169));
#22422=CARTESIAN_POINT('Ctrl Pts',(-41.7643569252322,37.2288122414519,38.1010458429616));
#22423=CARTESIAN_POINT('Ctrl Pts',(-41.7650060419899,37.2299377290699,38.1023180391421));
#22424=CARTESIAN_POINT('Ctrl Pts',(-41.7656551587476,37.2310632166879,38.1035902353226));
#22425=CARTESIAN_POINT('Ctrl Pts',(-41.766303855236,37.2321894651987,38.104861972639));
#22426=CARTESIAN_POINT('Ctrl Pts',(-41.7669521310807,37.2333164739512,38.1061332503562));
#22427=CARTESIAN_POINT('Ctrl Pts',(-41.7676004069255,37.2344434827038,38.1074045280734));
#22428=CARTESIAN_POINT('Ctrl Pts',(-41.7682482621266,37.2355712516982,38.1086753461915));
#22429=CARTESIAN_POINT('Ctrl Pts',(-41.7688956963101,37.2366997802825,38.1099457039759));
#22430=CARTESIAN_POINT('Ctrl Pts',(-41.7695431304936,37.2378283088669,38.1112160617603));
#22431=CARTESIAN_POINT('Ctrl Pts',(-41.7701901436595,37.2389575970412,38.112485959211));
#22432=CARTESIAN_POINT('Ctrl Pts',(-41.7708367354343,37.2400876441529,38.1137553955942));
#22433=CARTESIAN_POINT('Ctrl Pts',(-41.7714833272091,37.2412176912646,38.1150248319773));
#22434=CARTESIAN_POINT('Ctrl Pts',(-41.7721294975928,37.2423484973136,38.1162938072928));
#22435=CARTESIAN_POINT('Ctrl Pts',(-41.7727752462124,37.2434800616463,38.1175623208073));
#22436=CARTESIAN_POINT('Ctrl Pts',(-41.773420994832,37.2446116259791,38.1188308343217));
#22437=CARTESIAN_POINT('Ctrl Pts',(-41.7740663216875,37.2457439485957,38.1200988860351));
#22438=CARTESIAN_POINT('Ctrl Pts',(-41.7747112264064,37.2468770288417,38.1213664752145));
#22439=CARTESIAN_POINT('Ctrl Pts',(-41.7753561311253,37.2480101090876,38.1226340643939));
#22440=CARTESIAN_POINT('Ctrl Pts',(-41.7760006137076,37.2491439469631,38.1239011910393));
#22441=CARTESIAN_POINT('Ctrl Pts',(-41.7766446737812,37.2502785418127,38.1251678544182));
#22442=CARTESIAN_POINT('Ctrl Pts',(-41.7772887338548,37.2514131366622,38.1264345177972));
#22443=CARTESIAN_POINT('Ctrl Pts',(-41.7779323714198,37.252548488486,38.1277007179098));
#22444=CARTESIAN_POINT('Ctrl Pts',(-41.7785755861045,37.2536845966279,38.1289664540241));
#22445=CARTESIAN_POINT('Ctrl Pts',(-41.7792188007892,37.2548207047697,38.1302321901384));
#22446=CARTESIAN_POINT('Ctrl Pts',(-41.7798615925936,37.2559575692297,38.1314974622543));
#22447=CARTESIAN_POINT('Ctrl Pts',(-41.7805039611468,37.2570951893507,38.1327622696407));
#22448=CARTESIAN_POINT('Ctrl Pts',(-41.7811463296999,37.2582328094719,38.134027077027));
#22449=CARTESIAN_POINT('Ctrl Pts',(-41.7817882750017,37.2593711852541,38.1352914196837));
#22450=CARTESIAN_POINT('Ctrl Pts',(-41.7824297966815,37.2605103160397,38.1365552968799));
#22451=CARTESIAN_POINT('Ctrl Pts',(-41.7467400817451,37.2010672456454,38.0706862117665));
#22452=CARTESIAN_POINT('Ctrl Pts',(-41.7474624663532,37.2022871437449,38.0720880159783));
#22453=CARTESIAN_POINT('Ctrl Pts',(-41.74818434518,37.2035079719612,38.0734892714123));
#22454=CARTESIAN_POINT('Ctrl Pts',(-41.7489057177088,37.204729729421,38.0748899770657));
#22455=CARTESIAN_POINT('Ctrl Pts',(-41.7496264496923,37.2059504020168,38.0762894389575));
#22456=CARTESIAN_POINT('Ctrl Pts',(-41.7503466762767,37.2071720022066,38.0776883520447));
#22457=CARTESIAN_POINT('Ctrl Pts',(-41.7510663969476,37.2083945291177,38.0790867153282));
#22458=CARTESIAN_POINT('Ctrl Pts',(-41.7517861176184,37.2096170560288,38.0804850786117));
#22459=CARTESIAN_POINT('Ctrl Pts',(-41.7525053323757,37.2108405096613,38.0818828920914));
#22460=CARTESIAN_POINT('Ctrl Pts',(-41.7532240407058,37.2120648891413,38.083280154769));
#22461=CARTESIAN_POINT('Ctrl Pts',(-41.7539427490358,37.2132892686213,38.0846774174467));
#22462=CARTESIAN_POINT('Ctrl Pts',(-41.7546609509386,37.2145145739489,38.0860741293221));
#22463=CARTESIAN_POINT('Ctrl Pts',(-41.7553786459012,37.2157408042489,38.0874702893979));
#22464=CARTESIAN_POINT('Ctrl Pts',(-41.7560963408638,37.2169670345488,38.0888664494737));
#22465=CARTESIAN_POINT('Ctrl Pts',(-41.7568135288862,37.2181941898211,38.0902620577498));
#22466=CARTESIAN_POINT('Ctrl Pts',(-41.7575302094561,37.2194222691894,38.0916571132293));
#22467=CARTESIAN_POINT('Ctrl Pts',(-41.7582468900261,37.2206503485575,38.0930521687089));
#22468=CARTESIAN_POINT('Ctrl Pts',(-41.7589630631436,37.2218793520216,38.094446671392));
#22469=CARTESIAN_POINT('Ctrl Pts',(-41.7596787282971,37.2231092787038,38.0958406202826));
#22470=CARTESIAN_POINT('Ctrl Pts',(-41.7603943934506,37.2243392053861,38.0972345691731));
#22471=CARTESIAN_POINT('Ctrl Pts',(-41.7611095506402,37.2255700552863,38.0986279642712));
#22472=CARTESIAN_POINT('Ctrl Pts',(-41.761824199355,37.2268018275256,38.1000208045815));
#22473=CARTESIAN_POINT('Ctrl Pts',(-41.7625388480698,37.2280335997649,38.1014136448918));
#22474=CARTESIAN_POINT('Ctrl Pts',(-41.7632529883098,37.2292662943431,38.1028059304144));
#22475=CARTESIAN_POINT('Ctrl Pts',(-41.763966619565,37.2304999103799,38.1041976601548));
#22476=CARTESIAN_POINT('Ctrl Pts',(-41.7646802508202,37.2317335264167,38.1055893898952));
#22477=CARTESIAN_POINT('Ctrl Pts',(-41.7653933730906,37.232968063912,38.1069805638536));
#22478=CARTESIAN_POINT('Ctrl Pts',(-41.7661059858668,37.2342035219841,38.108371181036));
#22479=CARTESIAN_POINT('Ctrl Pts',(-41.766818598643,37.2354389800562,38.1097617982186));
#22480=CARTESIAN_POINT('Ctrl Pts',(-41.767530701925,37.2366753587051,38.1111518586253));
#22481=CARTESIAN_POINT('Ctrl Pts',(-41.7682422952044,37.2379126570476,38.1125413612635));
#22482=CARTESIAN_POINT('Ctrl Pts',(-41.7689538884836,37.2391499553902,38.1139308639016));
#22483=CARTESIAN_POINT('Ctrl Pts',(-41.7696649717601,37.2403881734266,38.1153198087711));
#22484=CARTESIAN_POINT('Ctrl Pts',(-41.7703755445259,37.2416273102722,38.11670819488));
#22485=CARTESIAN_POINT('Ctrl Pts',(-41.7710861172917,37.2428664471179,38.1180965809888));
#22486=CARTESIAN_POINT('Ctrl Pts',(-41.7717961795469,37.2441065027729,38.119484408337));
#22487=CARTESIAN_POINT('Ctrl Pts',(-41.7725057307843,37.2453474763514,38.1208716759333));
#22488=CARTESIAN_POINT('Ctrl Pts',(-41.7732152820216,37.24658844993,38.1222589435297));
#22489=CARTESIAN_POINT('Ctrl Pts',(-41.7739243222412,37.2478303414323,38.1236456513741));
#22490=CARTESIAN_POINT('Ctrl Pts',(-41.7746328509364,37.2490731499712,38.1250317984762));
#22491=CARTESIAN_POINT('Ctrl Pts',(-41.7753413796317,37.2503159585101,38.1264179455783));
#22492=CARTESIAN_POINT('Ctrl Pts',(-41.7760493968028,37.2515596840855,38.1278035319381));
#22493=CARTESIAN_POINT('Ctrl Pts',(-41.7767569019439,37.2528043258094,38.1291885565659));
#22494=CARTESIAN_POINT('Ctrl Pts',(-41.7774644070851,37.2540489675332,38.1305735811937));
#22495=CARTESIAN_POINT('Ctrl Pts',(-41.7781714001963,37.2552945254054,38.1319580440895));
#22496=CARTESIAN_POINT('Ctrl Pts',(-41.7788778807726,37.2565409985362,38.1333419442646));
#22497=CARTESIAN_POINT('Ctrl Pts',(-41.7795843613489,37.257787471667,38.1347258444396));
#22498=CARTESIAN_POINT('Ctrl Pts',(-41.7802903293903,37.2590348600565,38.1361091818938));
#22499=CARTESIAN_POINT('Ctrl Pts',(-41.7809957843926,37.2602831628138,38.1374919556392));
#22500=CARTESIAN_POINT('Ctrl Pts',(-41.7284556368598,37.1796898657602,38.0513058194986));
#22501=CARTESIAN_POINT('Ctrl Pts',(-41.72944530003,37.1813261852412,38.0531959552349));
#22502=CARTESIAN_POINT('Ctrl Pts',(-41.7304341078028,37.1829640881581,38.0550851651249));
#22503=CARTESIAN_POINT('Ctrl Pts',(-41.7314220591106,37.1846035727302,38.0569734471179));
#22504=CARTESIAN_POINT('Ctrl Pts',(-41.7324091331635,37.186241601516,38.0588600524042));
#22505=CARTESIAN_POINT('Ctrl Pts',(-41.7333953522717,37.1878812091493,38.0607457314407));
#22506=CARTESIAN_POINT('Ctrl Pts',(-41.7343807153722,37.1895223938508,38.0626304821839));
#22507=CARTESIAN_POINT('Ctrl Pts',(-41.7353660784728,37.1911635785522,38.0645152329272));
#22508=CARTESIAN_POINT('Ctrl Pts',(-41.7363505855657,37.1928063403217,38.0663990553772));
#22509=CARTESIAN_POINT('Ctrl Pts',(-41.7373342355896,37.1944506773768,38.0682819474925));
#22510=CARTESIAN_POINT('Ctrl Pts',(-41.7383178856135,37.1960950144319,38.0701648396078));
#22511=CARTESIAN_POINT('Ctrl Pts',(-41.7393006785684,37.1977409267727,38.0720468013883));
#22512=CARTESIAN_POINT('Ctrl Pts',(-41.7402826133948,37.1993884126133,38.0739278307945));
#22513=CARTESIAN_POINT('Ctrl Pts',(-41.7412645482211,37.201035898454,38.0758088602006));
#22514=CARTESIAN_POINT('Ctrl Pts',(-41.7422456249189,37.2026849577945,38.0776889572324));
#22515=CARTESIAN_POINT('Ctrl Pts',(-41.7432258424304,37.204335588846,38.0795681198521));
#22516=CARTESIAN_POINT('Ctrl Pts',(-41.7442060599419,37.2059862198976,38.0814472824717));
#22517=CARTESIAN_POINT('Ctrl Pts',(-41.7451854182669,37.2076384226602,38.0833255106791));
#22518=CARTESIAN_POINT('Ctrl Pts',(-41.7461639163495,37.2092921953418,38.0852028024386));
#22519=CARTESIAN_POINT('Ctrl Pts',(-41.7471424144321,37.2109459680234,38.0870800941981));
#22520=CARTESIAN_POINT('Ctrl Pts',(-41.7481200522723,37.2126013106239,38.0889564495096));
#22521=CARTESIAN_POINT('Ctrl Pts',(-41.7490968288155,37.2142582213483,38.090831866339));
#22522=CARTESIAN_POINT('Ctrl Pts',(-41.7500736053588,37.2159151320727,38.0927072831685));
#22523=CARTESIAN_POINT('Ctrl Pts',(-41.7510495206052,37.2175736109209,38.0945817615159));
#22524=CARTESIAN_POINT('Ctrl Pts',(-41.7520245735021,37.2192336560945,38.0964552993493));
#22525=CARTESIAN_POINT('Ctrl Pts',(-41.752999626399,37.2208937012682,38.0983288371826));
#22526=CARTESIAN_POINT('Ctrl Pts',(-41.7539738169465,37.2225553127673,38.1002014345018));
#22527=CARTESIAN_POINT('Ctrl Pts',(-41.7549471440936,37.2242184887904,38.1020730892768));
#22528=CARTESIAN_POINT('Ctrl Pts',(-41.7559204712406,37.2258816648134,38.1039447440518));
#22529=CARTESIAN_POINT('Ctrl Pts',(-41.7568929349873,37.2275464053604,38.1058154562824));
#22530=CARTESIAN_POINT('Ctrl Pts',(-41.7578645342845,37.2292127086268,38.1076852239405));
#22531=CARTESIAN_POINT('Ctrl Pts',(-41.7588361335817,37.230879011893,38.1095549915986));
#22532=CARTESIAN_POINT('Ctrl Pts',(-41.7598068684293,37.2325468778786,38.1114238146841));
#22533=CARTESIAN_POINT('Ctrl Pts',(-41.76077673778,37.2342163047757,38.1132916911706));
#22534=CARTESIAN_POINT('Ctrl Pts',(-41.7617466071307,37.2358857316728,38.1151595676571));
#22535=CARTESIAN_POINT('Ctrl Pts',(-41.7627156109845,37.2375567194813,38.1170264975447));
#22536=CARTESIAN_POINT('Ctrl Pts',(-41.7636837482957,37.2392292663904,38.1188924788088));
#22537=CARTESIAN_POINT('Ctrl Pts',(-41.7646518856068,37.2409018132995,38.1207584600729));
#22538=CARTESIAN_POINT('Ctrl Pts',(-41.7656191563754,37.2425759193091,38.1226234927135));
#22539=CARTESIAN_POINT('Ctrl Pts',(-41.7665855595574,37.2442515826052,38.1244875747081));
#22540=CARTESIAN_POINT('Ctrl Pts',(-41.7675519627395,37.2459272459012,38.1263516567027));
#22541=CARTESIAN_POINT('Ctrl Pts',(-41.768517498335,37.2476044664838,38.1282147880512));
#22542=CARTESIAN_POINT('Ctrl Pts',(-41.7694821653018,37.2492832425355,38.1300769667331));
#22543=CARTESIAN_POINT('Ctrl Pts',(-41.7704468322687,37.2509620185871,38.131939145415));
#22544=CARTESIAN_POINT('Ctrl Pts',(-41.7714106306068,37.2526423501081,38.1338003714302));
#22545=CARTESIAN_POINT('Ctrl Pts',(-41.7723735592759,37.2543242352779,38.1356606427601));
#22546=CARTESIAN_POINT('Ctrl Pts',(-41.7733364879449,37.2560061204476,38.1375209140899));
#22547=CARTESIAN_POINT('Ctrl Pts',(-41.7742985469448,37.2576895592663,38.1393802307343));
#22548=CARTESIAN_POINT('Ctrl Pts',(-41.775259735237,37.2593745499102,38.1412385906764));
#22549=CARTESIAN_POINT('Ctrl Pts',(-41.7091602750971,37.1578460913556,38.0313362231075));
#22550=CARTESIAN_POINT('Ctrl Pts',(-41.7104420238158,37.1599035150217,38.0337310951134));
#22551=CARTESIAN_POINT('Ctrl Pts',(-41.7117223763588,37.1619635480723,38.0361244614683));
#22552=CARTESIAN_POINT('Ctrl Pts',(-41.7130013305215,37.1640261868666,38.0385163179722));
#22553=CARTESIAN_POINT('Ctrl Pts',(-41.7142791490322,37.1660869941335,38.0409060506185));
#22554=CARTESIAN_POINT('Ctrl Pts',(-41.7155555716447,37.1681504025185,38.0432942760941));
#22555=CARTESIAN_POINT('Ctrl Pts',(-41.7168305961639,37.1702164083836,38.0456809902143));
#22556=CARTESIAN_POINT('Ctrl Pts',(-41.7181056206831,37.1722824142486,38.0480677043346));
#22557=CARTESIAN_POINT('Ctrl Pts',(-41.719379247109,37.1743510175936,38.0504529070995));
#22558=CARTESIAN_POINT('Ctrl Pts',(-41.7206514732504,37.1764222147733,38.0528365943289));
#22559=CARTESIAN_POINT('Ctrl Pts',(-41.7219236993918,37.178493411953,38.0552202815582));
#22560=CARTESIAN_POINT('Ctrl Pts',(-41.7231945252486,37.1805672029672,38.0576024532521));
#22561=CARTESIAN_POINT('Ctrl Pts',(-41.7244639486337,37.1826435841636,38.0599831052344));
#22562=CARTESIAN_POINT('Ctrl Pts',(-41.7257333720188,37.18471996536,38.0623637572168));
#22563=CARTESIAN_POINT('Ctrl Pts',(-41.727001392932,37.1867989367385,38.0647428894876));
#22564=CARTESIAN_POINT('Ctrl Pts',(-41.7282680091901,37.1888804946396,38.0671204978753));
#22565=CARTESIAN_POINT('Ctrl Pts',(-41.7295346254482,37.1909620525406,38.069498106263));
#22566=CARTESIAN_POINT('Ctrl Pts',(-41.7307998370511,37.1930461969642,38.0718741907675));
#22567=CARTESIAN_POINT('Ctrl Pts',(-41.7320636418194,37.1951329242436,38.0742487472214));
#22568=CARTESIAN_POINT('Ctrl Pts',(-41.7333274465877,37.1972196515231,38.0766233036752));
#22569=CARTESIAN_POINT('Ctrl Pts',(-41.7345898445214,37.1993089616584,38.0789963320785));
#22570=CARTESIAN_POINT('Ctrl Pts',(-41.7358508334449,37.2014008509757,38.081367828268));
#22571=CARTESIAN_POINT('Ctrl Pts',(-41.7371118223684,37.203492740293,38.0837393244575));
#22572=CARTESIAN_POINT('Ctrl Pts',(-41.7383714022818,37.2055872087923,38.0861092884332));
#22573=CARTESIAN_POINT('Ctrl Pts',(-41.7396295710134,37.2076842527928,38.0884777160364));
#22574=CARTESIAN_POINT('Ctrl Pts',(-41.740887739745,37.2097812967933,38.0908461436395));
#22575=CARTESIAN_POINT('Ctrl Pts',(-41.7421444972949,37.211880916295,38.09321303487));
#22576=CARTESIAN_POINT('Ctrl Pts',(-41.7433998414954,37.2139831076097,38.0955783855734));
#22577=CARTESIAN_POINT('Ctrl Pts',(-41.7446551856959,37.2160852989245,38.0979437362768));
#22578=CARTESIAN_POINT('Ctrl Pts',(-41.745909116547,37.2181900620525,38.100307546453));
#22579=CARTESIAN_POINT('Ctrl Pts',(-41.7471616318849,37.2202973932986,38.1026698119518));
#22580=CARTESIAN_POINT('Ctrl Pts',(-41.7484141472228,37.2224047245446,38.1050320774506));
#22581=CARTESIAN_POINT('Ctrl Pts',(-41.7496652470475,37.2245146239088,38.1073927982719));
#22582=CARTESIAN_POINT('Ctrl Pts',(-41.7509149291994,37.2266270876888,38.1097519702699));
#22583=CARTESIAN_POINT('Ctrl Pts',(-41.7521646113512,37.2287395514689,38.112111142268));
#22584=CARTESIAN_POINT('Ctrl Pts',(-41.7534128758301,37.230854579665,38.1144687654425));
#22585=CARTESIAN_POINT('Ctrl Pts',(-41.7546597204802,37.2329721685677,38.1168248356522));
#22586=CARTESIAN_POINT('Ctrl Pts',(-41.7559065651303,37.2350897574705,38.1191809058618));
#22587=CARTESIAN_POINT('Ctrl Pts',(-41.7571519899515,37.23720990708,38.1215354231064));
#22588=CARTESIAN_POINT('Ctrl Pts',(-41.7583959927921,37.23933261368,38.1238883832486));
#22589=CARTESIAN_POINT('Ctrl Pts',(-41.7596399956326,37.2414553202799,38.1262413433909));
#22590=CARTESIAN_POINT('Ctrl Pts',(-41.7608825764924,37.2435805838703,38.1285927464307));
#22591=CARTESIAN_POINT('Ctrl Pts',(-41.7621237332236,37.2457084007279,38.1309425882353));
#22592=CARTESIAN_POINT('Ctrl Pts',(-41.7633648899547,37.2478362175854,38.1332924300399));
#22593=CARTESIAN_POINT('Ctrl Pts',(-41.7646046225571,37.24996658771,38.1356407106091));
#22594=CARTESIAN_POINT('Ctrl Pts',(-41.7658429288868,37.2520995073713,38.1379874258143));
#22595=CARTESIAN_POINT('Ctrl Pts',(-41.7670812352165,37.2542324270326,38.1403341410195));
#22596=CARTESIAN_POINT('Ctrl Pts',(-41.7683181152735,37.2563678962306,38.1426792908607));
#22597=CARTESIAN_POINT('Ctrl Pts',(-41.7695535669177,37.2585059112279,38.1450228712136));
#22598=CARTESIAN_POINT('Ctrl Pts',(-41.6889393053371,37.1357612177105,38.0109524721443));
#22599=CARTESIAN_POINT('Ctrl Pts',(-41.6905364576388,37.1382386034432,38.0138650725638));
#22600=CARTESIAN_POINT('Ctrl Pts',(-41.6921314669563,37.1407200717346,38.0167753755858));
#22601=CARTESIAN_POINT('Ctrl Pts',(-41.6937243283598,37.1432056149149,38.019683372215));
#22602=CARTESIAN_POINT('Ctrl Pts',(-41.6953157753764,37.1456889510481,38.0225887866781));
#22603=CARTESIAN_POINT('Ctrl Pts',(-41.6969050782917,37.1481763548368,38.0254918988425));
#22604=CARTESIAN_POINT('Ctrl Pts',(-41.6984922322021,37.1506678186063,38.0283926997509));
#22605=CARTESIAN_POINT('Ctrl Pts',(-41.7000793861125,37.1531592823757,38.0312935006593));
#22606=CARTESIAN_POINT('Ctrl Pts',(-41.701664391018,37.1556548061259,38.0341919903117));
#22607=CARTESIAN_POINT('Ctrl Pts',(-41.7032472420284,37.1581543821572,38.0370881597651));
#22608=CARTESIAN_POINT('Ctrl Pts',(-41.7048300930387,37.1606539581885,38.0399843292186));
#22609=CARTESIAN_POINT('Ctrl Pts',(-41.7064107901537,37.1631575865009,38.042878178473));
#22610=CARTESIAN_POINT('Ctrl Pts',(-41.7079893284965,37.1656652593697,38.0457696985998));
#22611=CARTESIAN_POINT('Ctrl Pts',(-41.7095678668393,37.1681729322385,38.0486612187265));
#22612=CARTESIAN_POINT('Ctrl Pts',(-41.7111442464097,37.1706846496637,38.0515504097256));
#22613=CARTESIAN_POINT('Ctrl Pts',(-41.7127184623441,37.1732004038957,38.0544372626828));
#22614=CARTESIAN_POINT('Ctrl Pts',(-41.7142926782785,37.1757161581277,38.0573241156399));
#22615=CARTESIAN_POINT('Ctrl Pts',(-41.7158647305767,37.1782359491665,38.0602086305551));
#22616=CARTESIAN_POINT('Ctrl Pts',(-41.7174346143886,37.1807597692374,38.0630907985285));
#22617=CARTESIAN_POINT('Ctrl Pts',(-41.7190044982004,37.1832835893083,38.0659729665019));
#22618=CARTESIAN_POINT('Ctrl Pts',(-41.7205722135258,37.1858114384115,38.0688527875335));
#22619=CARTESIAN_POINT('Ctrl Pts',(-41.7221377555276,37.1883433087475,38.0717302527378));
#22620=CARTESIAN_POINT('Ctrl Pts',(-41.7237032975295,37.1908751790835,38.0746077179421));
#22621=CARTESIAN_POINT('Ctrl Pts',(-41.7252666662079,37.1934110706522,38.0774828273193));
#22622=CARTESIAN_POINT('Ctrl Pts',(-41.7268278567391,37.1959509756296,38.0803555719983));
#22623=CARTESIAN_POINT('Ctrl Pts',(-41.7283890472704,37.198490880607,38.0832283166774));
#22624=CARTESIAN_POINT('Ctrl Pts',(-41.7299480596546,37.2010347989929,38.0860986966584));
#22625=CARTESIAN_POINT('Ctrl Pts',(-41.7315048890814,37.2035827229384,38.0889667030851));
#22626=CARTESIAN_POINT('Ctrl Pts',(-41.7330617185083,37.2061306468839,38.0918347095118));
#22627=CARTESIAN_POINT('Ctrl Pts',(-41.7346163649779,37.208682576389,38.0947003423842));
#22628=CARTESIAN_POINT('Ctrl Pts',(-41.7361688236936,37.2112385035799,38.0975635928606));
#22629=CARTESIAN_POINT('Ctrl Pts',(-41.7377212824092,37.2137944307708,38.1004268433371));
#22630=CARTESIAN_POINT('Ctrl Pts',(-41.7392715533709,37.2163543556476,38.1032877114176));
#22631=CARTESIAN_POINT('Ctrl Pts',(-41.7408196317953,37.2189182703119,38.1061461882752));
#22632=CARTESIAN_POINT('Ctrl Pts',(-41.7423677102199,37.2214821849762,38.1090046651329));
#22633=CARTESIAN_POINT('Ctrl Pts',(-41.7439135961072,37.224050089428,38.1118607507677));
#22634=CARTESIAN_POINT('Ctrl Pts',(-41.7454572846877,37.2266219757442,38.1147144363676));
#22635=CARTESIAN_POINT('Ctrl Pts',(-41.7470009732681,37.2291938620605,38.1175681219675));
#22636=CARTESIAN_POINT('Ctrl Pts',(-41.7485424645417,37.2317697302412,38.1204194075323));
#22637=CARTESIAN_POINT('Ctrl Pts',(-41.7500817537524,37.2343495723389,38.1232682842648));
#22638=CARTESIAN_POINT('Ctrl Pts',(-41.7516210429631,37.2369294144365,38.1261171609973));
#22639=CARTESIAN_POINT('Ctrl Pts',(-41.7531581301108,37.2395132304511,38.1289636288975));
#22640=CARTESIAN_POINT('Ctrl Pts',(-41.7546930104531,37.2421010124104,38.1318076791829));
#22641=CARTESIAN_POINT('Ctrl Pts',(-41.7562278907953,37.2446887943699,38.1346517294682));
#22642=CARTESIAN_POINT('Ctrl Pts',(-41.7577605643321,37.247280542274,38.1374933621388));
#22643=CARTESIAN_POINT('Ctrl Pts',(-41.7592910263345,37.2498762481265,38.140332568427));
#22644=CARTESIAN_POINT('Ctrl Pts',(-41.7608214883369,37.2524719539789,38.1431717747151));
#22645=CARTESIAN_POINT('Ctrl Pts',(-41.7623497388049,37.2550716177796,38.1460085546209));
#22646=CARTESIAN_POINT('Ctrl Pts',(-41.7638757730233,37.2576752315076,38.1488428993918));
#22647=CARTESIAN_POINT('Ctrl Pts',(-41.6687183355772,37.1136763440655,37.9905687211811));
#22648=CARTESIAN_POINT('Ctrl Pts',(-41.6706308914618,37.1165736918647,37.9939990500142));
#22649=CARTESIAN_POINT('Ctrl Pts',(-41.6725405575538,37.119476595397,37.9974262897033));
#22650=CARTESIAN_POINT('Ctrl Pts',(-41.6744473261982,37.1223850429631,38.0008504264578));
#22651=CARTESIAN_POINT('Ctrl Pts',(-41.6763524017206,37.1252909079628,38.0042715227377));
#22652=CARTESIAN_POINT('Ctrl Pts',(-41.6782545849386,37.1282023071551,38.007689521591));
#22653=CARTESIAN_POINT('Ctrl Pts',(-41.6801538682403,37.1311192288289,38.0111044092876));
#22654=CARTESIAN_POINT('Ctrl Pts',(-41.6820531515419,37.1340361505028,38.0145192969841));
#22655=CARTESIAN_POINT('Ctrl Pts',(-41.6839495349271,37.1369585946581,38.017931073524));
#22656=CARTESIAN_POINT('Ctrl Pts',(-41.6858430108064,37.1398865495411,38.0213397252014));
#22657=CARTESIAN_POINT('Ctrl Pts',(-41.6877364866856,37.1428145044241,38.0247483768789));
#22658=CARTESIAN_POINT('Ctrl Pts',(-41.6896270550588,37.1457479700346,38.0281539036939));
#22659=CARTESIAN_POINT('Ctrl Pts',(-41.6915147083593,37.1486869345758,38.0315562919651));
#22660=CARTESIAN_POINT('Ctrl Pts',(-41.6934023616597,37.1516258991171,38.0349586802362));
#22661=CARTESIAN_POINT('Ctrl Pts',(-41.6952870998874,37.154570362589,38.0383579299636));
#22662=CARTESIAN_POINT('Ctrl Pts',(-41.697168915498,37.1575203131519,38.0417540274902));
#22663=CARTESIAN_POINT('Ctrl Pts',(-41.6990507311087,37.1604702637148,38.0451501250169));
#22664=CARTESIAN_POINT('Ctrl Pts',(-41.7009296241024,37.1634257013687,38.0485430703428));
#22665=CARTESIAN_POINT('Ctrl Pts',(-41.7028055869577,37.1663866142312,38.0519328498357));
#22666=CARTESIAN_POINT('Ctrl Pts',(-41.7046815498131,37.1693475270936,38.0553226293286));
#22667=CARTESIAN_POINT('Ctrl Pts',(-41.7065545825302,37.1723139151648,38.0587092429884));
#22668=CARTESIAN_POINT('Ctrl Pts',(-41.7084246776104,37.1752857665193,38.0620926772076));
#22669=CARTESIAN_POINT('Ctrl Pts',(-41.7102947726906,37.178257617874,38.0654761114268));
#22670=CARTESIAN_POINT('Ctrl Pts',(-41.712161930134,37.1812349325122,38.0688563662053));
#22671=CARTESIAN_POINT('Ctrl Pts',(-41.7140261424648,37.1842176984664,38.0722334279603));
#22672=CARTESIAN_POINT('Ctrl Pts',(-41.7158903547957,37.1872004644206,38.0756104897153));
#22673=CARTESIAN_POINT('Ctrl Pts',(-41.7177516220142,37.1901886816908,38.0789843584468));
#22674=CARTESIAN_POINT('Ctrl Pts',(-41.7196099366675,37.193182338267,38.0823550205968));
#22675=CARTESIAN_POINT('Ctrl Pts',(-41.7214682513208,37.1961759948432,38.0857256827468));
#22676=CARTESIAN_POINT('Ctrl Pts',(-41.7233236134089,37.1991750907254,38.0890931383153));
#22677=CARTESIAN_POINT('Ctrl Pts',(-41.7251760155023,37.2021796138613,38.0924573737694));
#22678=CARTESIAN_POINT('Ctrl Pts',(-41.7270284175957,37.205184136997,38.0958216092235));
#22679=CARTESIAN_POINT('Ctrl Pts',(-41.7288778596942,37.2081940873865,38.0991826245632));
#22680=CARTESIAN_POINT('Ctrl Pts',(-41.7307243343914,37.211209452935,38.1025404062805));
#22681=CARTESIAN_POINT('Ctrl Pts',(-41.7325708090885,37.2142248184835,38.1058981879979));
#22682=CARTESIAN_POINT('Ctrl Pts',(-41.7344143163842,37.217245599191,38.1092527360929));
#22683=CARTESIAN_POINT('Ctrl Pts',(-41.7362548488951,37.2202717829207,38.112604037083));
#22684=CARTESIAN_POINT('Ctrl Pts',(-41.738095381406,37.2232979666505,38.1159553380731));
#22685=CARTESIAN_POINT('Ctrl Pts',(-41.739932939132,37.2263295534024,38.1193033919582));
#22686=CARTESIAN_POINT('Ctrl Pts',(-41.7417675147128,37.2293665309978,38.122648185281));
#22687=CARTESIAN_POINT('Ctrl Pts',(-41.7436020902936,37.2324035085931,38.1259929786038));
#22688=CARTESIAN_POINT('Ctrl Pts',(-41.7454336837292,37.2354458770318,38.1293345113643));
#22689=CARTESIAN_POINT('Ctrl Pts',(-41.7472622876826,37.2384936240931,38.1326727701304));
#22690=CARTESIAN_POINT('Ctrl Pts',(-41.749090891636,37.2415413711543,38.1360110288966));
#22691=CARTESIAN_POINT('Ctrl Pts',(-41.7509165061071,37.2445944968381,38.1393460136685));
#22692=CARTESIAN_POINT('Ctrl Pts',(-41.7527391237821,37.2476529888817,38.1426777110396));
#22693=CARTESIAN_POINT('Ctrl Pts',(-41.7545617414572,37.2507114809253,38.1460094084107));
#22694=CARTESIAN_POINT('Ctrl Pts',(-41.7563813623363,37.2537753393287,38.1493378183811));
#22695=CARTESIAN_POINT('Ctrl Pts',(-41.7581979791288,37.2568445517873,38.1526629275699));
#22696=CARTESIAN_POINT('Ctrl Pts',(-41.6475728892226,37.0913544340564,37.969773861755));
#22697=CARTESIAN_POINT('Ctrl Pts',(-41.6498241513043,37.0946704940769,37.9737348553367));
#22698=CARTESIAN_POINT('Ctrl Pts',(-41.6520715703113,37.0979940317792,37.9776917557169));
#22699=CARTESIAN_POINT('Ctrl Pts',(-41.6543151342611,37.1013250292433,37.9816445416399));
#22700=CARTESIAN_POINT('Ctrl Pts',(-41.6565567060304,37.1046530689362,37.9855938176725));
#22701=CARTESIAN_POINT('Ctrl Pts',(-41.6587944295858,37.1079885551487,37.9895389865515));
#22702=CARTESIAN_POINT('Ctrl Pts',(-41.6610282930162,37.1113314699335,37.9934800271196));
#22703=CARTESIAN_POINT('Ctrl Pts',(-41.6632621564465,37.1146743847181,37.9974210676877));
#22704=CARTESIAN_POINT('Ctrl Pts',(-41.6654921597517,37.1180247280751,38.0013579799447));
#22705=CARTESIAN_POINT('Ctrl Pts',(-41.6677182910599,37.1213824819817,38.0052907427754));
#22706=CARTESIAN_POINT('Ctrl Pts',(-41.6699444223679,37.1247402358884,38.009223505606));
#22707=CARTESIAN_POINT('Ctrl Pts',(-41.6721666816788,37.128105400345,38.01315211901));
#22708=CARTESIAN_POINT('Ctrl Pts',(-41.6743850571597,37.1314779572543,38.0170765619143));
#22709=CARTESIAN_POINT('Ctrl Pts',(-41.6766034326405,37.1348505141636,38.0210010048186));
#22710=CARTESIAN_POINT('Ctrl Pts',(-41.6788179242914,37.1382304635258,38.024921277223));
#22711=CARTESIAN_POINT('Ctrl Pts',(-41.6810285203188,37.1416177871692,38.0288373580966));
#22712=CARTESIAN_POINT('Ctrl Pts',(-41.6832391163462,37.1450051108127,38.0327534389702));
#22713=CARTESIAN_POINT('Ctrl Pts',(-41.68544581675,37.1483998087376,38.0366653283129));
#22714=CARTESIAN_POINT('Ctrl Pts',(-41.6876486097765,37.1518018626979,38.0405730051363));
#22715=CARTESIAN_POINT('Ctrl Pts',(-41.6898514028029,37.1552039166582,38.0444806819597));
#22716=CARTESIAN_POINT('Ctrl Pts',(-41.6920502884518,37.1586133266541,38.0483841462638));
#22717=CARTESIAN_POINT('Ctrl Pts',(-41.6942452550088,37.1620300743655,38.0522833771027));
#22718=CARTESIAN_POINT('Ctrl Pts',(-41.6964402215659,37.165446822077,38.0561826079417));
#22719=CARTESIAN_POINT('Ctrl Pts',(-41.6986312690311,37.168870907504,38.0600776053155));
#22720=CARTESIAN_POINT('Ctrl Pts',(-41.7008183857296,37.1723023122527,38.0639683483214));
#22721=CARTESIAN_POINT('Ctrl Pts',(-41.7030055024282,37.1757337170013,38.0678590913274));
#22722=CARTESIAN_POINT('Ctrl Pts',(-41.7051886883601,37.1791724410717,38.0717455799653));
#22723=CARTESIAN_POINT('Ctrl Pts',(-41.7073679318905,37.1826184659959,38.0756277933756));
#22724=CARTESIAN_POINT('Ctrl Pts',(-41.7095471754209,37.1860644909201,38.0795100067858));
#22725=CARTESIAN_POINT('Ctrl Pts',(-41.7117224765497,37.1895178166982,38.0833879449684));
#22726=CARTESIAN_POINT('Ctrl Pts',(-41.713893823682,37.1929784247889,38.0872615871069));
#22727=CARTESIAN_POINT('Ctrl Pts',(-41.7160651708142,37.1964390328797,38.0911352292454));
#22728=CARTESIAN_POINT('Ctrl Pts',(-41.7182325639499,37.1999069232829,38.0950045753397));
#22729=CARTESIAN_POINT('Ctrl Pts',(-41.720395991534,37.2033820773839,38.098869604617));
#22730=CARTESIAN_POINT('Ctrl Pts',(-41.7225594191181,37.2068572314848,38.1027346338944));
#22731=CARTESIAN_POINT('Ctrl Pts',(-41.7247188811506,37.2103396492834,38.1065953463546));
#22732=CARTESIAN_POINT('Ctrl Pts',(-41.7268743661166,37.2138293120917,38.1104517212686));
#22733=CARTESIAN_POINT('Ctrl Pts',(-41.7290298510826,37.2173189748999,38.1143080961826));
#22734=CARTESIAN_POINT('Ctrl Pts',(-41.7311813589821,37.2208158827178,38.1181601335503));
#22735=CARTESIAN_POINT('Ctrl Pts',(-41.7333288783403,37.224320016784,38.1220078126863));
#22736=CARTESIAN_POINT('Ctrl Pts',(-41.7354763976986,37.2278241508502,38.1258554918223));
#22737=CARTESIAN_POINT('Ctrl Pts',(-41.7376199285156,37.2313355111647,38.1296988127267));
#22738=CARTESIAN_POINT('Ctrl Pts',(-41.7397594593571,37.2348540788934,38.1335377547582));
#22739=CARTESIAN_POINT('Ctrl Pts',(-41.7418989901986,37.238372646622,38.1373766967897));
#22740=CARTESIAN_POINT('Ctrl Pts',(-41.7440345210644,37.2418984217649,38.1412112599481));
#22741=CARTESIAN_POINT('Ctrl Pts',(-41.7461660405608,37.2454313854149,38.1450414236367));
#22742=CARTESIAN_POINT('Ctrl Pts',(-41.7482975600572,37.2489643490649,38.1488715873253));
#22743=CARTESIAN_POINT('Ctrl Pts',(-41.750425068184,37.2525045012221,38.1526973515439));
#22744=CARTESIAN_POINT('Ctrl Pts',(-41.7525485535879,37.256051822907,38.15651869574));
#22745=CARTESIAN_POINT('Ctrl Pts',(-41.6257141900876,37.0691011556449,37.9488313498428));
#22746=CARTESIAN_POINT('Ctrl Pts',(-41.6283229847769,37.0728276862717,37.9533303089943));
#22747=CARTESIAN_POINT('Ctrl Pts',(-41.6309267846842,37.0765641067473,37.9578239725956));
#22748=CARTESIAN_POINT('Ctrl Pts',(-41.6335255706247,37.0803103895415,37.9623123075375));
#22749=CARTESIAN_POINT('Ctrl Pts',(-41.636122048964,37.0840533458105,37.9667966570464));
#22750=CARTESIAN_POINT('Ctrl Pts',(-41.6387135222368,37.0878061468915,37.9712756873548));
#22751=CARTESIAN_POINT('Ctrl Pts',(-41.6412999713831,37.0915687651826,37.9757493655199));
#22752=CARTESIAN_POINT('Ctrl Pts',(-41.6438864205294,37.0953313834738,37.9802230436849));
#22753=CARTESIAN_POINT('Ctrl Pts',(-41.6464678455491,37.0991038189753,37.9846913697065));
#22754=CARTESIAN_POINT('Ctrl Pts',(-41.6490442274561,37.1028860439409,37.9891543107205));
#22755=CARTESIAN_POINT('Ctrl Pts',(-41.6516206093631,37.1066682689066,37.9936172517345));
#22756=CARTESIAN_POINT('Ctrl Pts',(-41.6541919481574,37.1104602833365,37.9980748077408));
#22757=CARTESIAN_POINT('Ctrl Pts',(-41.6567582249268,37.1142620593407,38.0025269459543));
#22758=CARTESIAN_POINT('Ctrl Pts',(-41.6593245016963,37.1180638353448,38.006979084168));
#22759=CARTESIAN_POINT('Ctrl Pts',(-41.6618857164409,37.1218753729231,38.0114258045888));
#22760=CARTESIAN_POINT('Ctrl Pts',(-41.6644418503232,37.1256966440421,38.0158670745116));
#22761=CARTESIAN_POINT('Ctrl Pts',(-41.6669979842055,37.1295179151611,38.0203083444344));
#22762=CARTESIAN_POINT('Ctrl Pts',(-41.6695490372254,37.1333489198205,38.0247441638592));
#22763=CARTESIAN_POINT('Ctrl Pts',(-41.6720949906201,37.1371896298438,38.0291745001607));
#22764=CARTESIAN_POINT('Ctrl Pts',(-41.6746409440149,37.1410303398672,38.0336048364622));
#22765=CARTESIAN_POINT('Ctrl Pts',(-41.6771817977843,37.1448807552543,38.0380296896405));
#22766=CARTESIAN_POINT('Ctrl Pts',(-41.6797175332409,37.1487408476856,38.042449027151));
#22767=CARTESIAN_POINT('Ctrl Pts',(-41.6822532686974,37.152600940117,38.0468683646616));
#22768=CARTESIAN_POINT('Ctrl Pts',(-41.6847838858408,37.1564707095926,38.0512821865043));
#22769=CARTESIAN_POINT('Ctrl Pts',(-41.6873093660587,37.1603501276504,38.055690460216));
#22770=CARTESIAN_POINT('Ctrl Pts',(-41.6898348462767,37.1642295457083,38.0600987339277));
#22771=CARTESIAN_POINT('Ctrl Pts',(-41.6923551895691,37.1681186123485,38.0645014595082));
#22772=CARTESIAN_POINT('Ctrl Pts',(-41.6948703773989,37.1720172989672,38.0688986045758));
#22773=CARTESIAN_POINT('Ctrl Pts',(-41.6973855652288,37.1759159855859,38.0732957496434));
#22774=CARTESIAN_POINT('Ctrl Pts',(-41.6998955975961,37.179824292183,38.0776873141981));
#22775=CARTESIAN_POINT('Ctrl Pts',(-41.7024004560398,37.1837421900134,38.0820732659402));
#22776=CARTESIAN_POINT('Ctrl Pts',(-41.7049053144835,37.1876600878437,38.0864592176823));
#22777=CARTESIAN_POINT('Ctrl Pts',(-41.7074049990036,37.1915875769071,38.0908395566119));
#22778=CARTESIAN_POINT('Ctrl Pts',(-41.7098994912149,37.1955246283172,38.0952142505117));
#22779=CARTESIAN_POINT('Ctrl Pts',(-41.7123939834263,37.1994616797273,38.0995889444116));
#22780=CARTESIAN_POINT('Ctrl Pts',(-41.714883283329,37.2034082934841,38.1039579932818));
#22781=CARTESIAN_POINT('Ctrl Pts',(-41.7173673726144,37.2073644405605,38.1083213649881));
#22782=CARTESIAN_POINT('Ctrl Pts',(-41.7198514618998,37.2113205876369,38.1126847366945));
#22783=CARTESIAN_POINT('Ctrl Pts',(-41.7223303405679,37.2152862680329,38.1170424312371));
#22784=CARTESIAN_POINT('Ctrl Pts',(-41.7248039903866,37.2192614525812,38.1213944165653));
#22785=CARTESIAN_POINT('Ctrl Pts',(-41.7272776402054,37.2232366371295,38.1257464018935));
#22786=CARTESIAN_POINT('Ctrl Pts',(-41.7297460611749,37.22722132583,38.1300926780074));
#22787=CARTESIAN_POINT('Ctrl Pts',(-41.7322092351399,37.2312154893756,38.1344332129404));
#22788=CARTESIAN_POINT('Ctrl Pts',(-41.734672409105,37.2352096529214,38.1387737478733));
#22789=CARTESIAN_POINT('Ctrl Pts',(-41.7371303360657,37.2392132913121,38.1431085416253));
#22790=CARTESIAN_POINT('Ctrl Pts',(-41.7395829979441,37.2432263751015,38.1474375623142));
#22791=CARTESIAN_POINT('Ctrl Pts',(-41.7420356598224,37.247239458891,38.1517665830032));
#22792=CARTESIAN_POINT('Ctrl Pts',(-41.7444830566185,37.251261988079,38.156089830629));
#22793=CARTESIAN_POINT('Ctrl Pts',(-41.7469251703319,37.2552939330803,38.1604072733946));
#22794=CARTESIAN_POINT('Ctrl Pts',(-41.6038554909526,37.0468478772333,37.9278888379305));
#22795=CARTESIAN_POINT('Ctrl Pts',(-41.6068218182495,37.0509848784665,37.9329257626518));
#22796=CARTESIAN_POINT('Ctrl Pts',(-41.6097819990572,37.0551341817153,37.9379561894743));
#22797=CARTESIAN_POINT('Ctrl Pts',(-41.6127360069883,37.0592957498397,37.9429800734352));
#22798=CARTESIAN_POINT('Ctrl Pts',(-41.6156873918975,37.063453622685,37.9479994964203));
#22799=CARTESIAN_POINT('Ctrl Pts',(-41.6186326148878,37.0676237386342,37.9530123881581));
#22800=CARTESIAN_POINT('Ctrl Pts',(-41.62157164975,37.0718060604318,37.9580187039201));
#22801=CARTESIAN_POINT('Ctrl Pts',(-41.6245106846123,37.0759883822295,37.9630250196822));
#22802=CARTESIAN_POINT('Ctrl Pts',(-41.6274435313465,37.0801829098755,37.9680247594683));
#22803=CARTESIAN_POINT('Ctrl Pts',(-41.6303701638525,37.0843896059001,37.9730178786657));
#22804=CARTESIAN_POINT('Ctrl Pts',(-41.6332967963584,37.0885963019248,37.978010997863));
#22805=CARTESIAN_POINT('Ctrl Pts',(-41.6362172146359,37.0928151663281,37.9829974964715));
#22806=CARTESIAN_POINT('Ctrl Pts',(-41.639131392694,37.0970461614271,37.9879773299944));
#22807=CARTESIAN_POINT('Ctrl Pts',(-41.642045570752,37.1012771565259,37.9929571635173));
#22808=CARTESIAN_POINT('Ctrl Pts',(-41.6449535085904,37.1055202823205,37.9979303319545));
#22809=CARTESIAN_POINT('Ctrl Pts',(-41.6478551803277,37.1097755009149,38.0028967909266));
#22810=CARTESIAN_POINT('Ctrl Pts',(-41.6507568520649,37.1140307195093,38.0078632498987));
#22811=CARTESIAN_POINT('Ctrl Pts',(-41.6536522577008,37.1182980309035,38.0128229994054));
#22812=CARTESIAN_POINT('Ctrl Pts',(-41.6565413714638,37.1225773969899,38.017775995185));
#22813=CARTESIAN_POINT('Ctrl Pts',(-41.6594304852268,37.1268567630762,38.0227289909647));
#22814=CARTESIAN_POINT('Ctrl Pts',(-41.6623133071169,37.1311481838545,38.0276752330172));
#22815=CARTESIAN_POINT('Ctrl Pts',(-41.6651898114729,37.1354516210057,38.0326146771993));
#22816=CARTESIAN_POINT('Ctrl Pts',(-41.6680663158288,37.139755058157,38.0375541213814));
#22817=CARTESIAN_POINT('Ctrl Pts',(-41.6709365026506,37.1440705116811,38.0424867676931));
#22818=CARTESIAN_POINT('Ctrl Pts',(-41.6738003463879,37.1483979430482,38.0474125721105));
#22819=CARTESIAN_POINT('Ctrl Pts',(-41.6766641901252,37.1527253744153,38.0523383765279));
#22820=CARTESIAN_POINT('Ctrl Pts',(-41.679521690778,37.1570647836254,38.057257339051));
#22821=CARTESIAN_POINT('Ctrl Pts',(-41.6823728229074,37.1614161319385,38.062169415776));
#22822=CARTESIAN_POINT('Ctrl Pts',(-41.6852239550367,37.1657674802517,38.0670814925009));
#22823=CARTESIAN_POINT('Ctrl Pts',(-41.6880687186425,37.1701307676679,38.0719866834278));
#22824=CARTESIAN_POINT('Ctrl Pts',(-41.6909070883976,37.1745059552378,38.0768849447736));
#22825=CARTESIAN_POINT('Ctrl Pts',(-41.6937454581527,37.1788811428077,38.0817832061194));
#22826=CARTESIAN_POINT('Ctrl Pts',(-41.6965774340572,37.1832682305312,38.0866745378841));
#22827=CARTESIAN_POINT('Ctrl Pts',(-41.6994029908958,37.1876671792505,38.0915588964065));
#22828=CARTESIAN_POINT('Ctrl Pts',(-41.7022285477345,37.1920661279698,38.0964432549289));
#22829=CARTESIAN_POINT('Ctrl Pts',(-41.7050476855074,37.1964769376847,38.1013206402089));
#22830=CARTESIAN_POINT('Ctrl Pts',(-41.7078603791122,37.2008995690293,38.1061910087076));
#22831=CARTESIAN_POINT('Ctrl Pts',(-41.710673072717,37.2053222003739,38.1110613772063));
#22832=CARTESIAN_POINT('Ctrl Pts',(-41.7134793221537,37.209756653348,38.1159247289238));
#22833=CARTESIAN_POINT('Ctrl Pts',(-41.716279102433,37.2142028883784,38.1207810204443));
#22834=CARTESIAN_POINT('Ctrl Pts',(-41.7190788827123,37.2186491234088,38.1256373119647));
#22835=CARTESIAN_POINT('Ctrl Pts',(-41.7218721938341,37.2231071404953,38.1304865432881));
#22836=CARTESIAN_POINT('Ctrl Pts',(-41.7246590109227,37.227576899858,38.1353286711225));
#22837=CARTESIAN_POINT('Ctrl Pts',(-41.7274458280114,37.2320466592206,38.1401707989569));
#22838=CARTESIAN_POINT('Ctrl Pts',(-41.7302261510669,37.2365281608594,38.1450058233024));
#22839=CARTESIAN_POINT('Ctrl Pts',(-41.7329999553273,37.2410213647883,38.1498337009917));
#22840=CARTESIAN_POINT('Ctrl Pts',(-41.7357737595877,37.2455145687171,38.154661578681));
#22841=CARTESIAN_POINT('Ctrl Pts',(-41.7385410450531,37.2500194749359,38.1594823097141));
#22842=CARTESIAN_POINT('Ctrl Pts',(-41.7413017870759,37.2545360432535,38.1642958510492));
#22843=CARTESIAN_POINT('Ctrl Pts',(-41.5812887586841,37.0246695558006,37.9068043561179));
#22844=CARTESIAN_POINT('Ctrl Pts',(-41.5846313316133,37.029208650787,37.9123864232581));
#22845=CARTESIAN_POINT('Ctrl Pts',(-41.5879664082902,37.0337629504581,37.9179605923033));
#22846=CARTESIAN_POINT('Ctrl Pts',(-41.5912939522271,37.0383324046554,37.923526802022));
#22847=CARTESIAN_POINT('Ctrl Pts',(-41.5946185414596,37.0428978013895,37.9290880692049));
#22848=CARTESIAN_POINT('Ctrl Pts',(-41.5979356113237,37.0474783257485,37.93464139119));
#22849=CARTESIAN_POINT('Ctrl Pts',(-41.6012451255902,37.0520739273846,37.940186707079));
#22850=CARTESIAN_POINT('Ctrl Pts',(-41.6045546398567,37.0566695290208,37.945732022968));
#22851=CARTESIAN_POINT('Ctrl Pts',(-41.6078565985256,37.0612802079339,37.9512693327608));
#22852=CARTESIAN_POINT('Ctrl Pts',(-41.6111509655294,37.0659059134548,37.9567985757307));
#22853=CARTESIAN_POINT('Ctrl Pts',(-41.6144453325332,37.0705316189757,37.9623278187007));
#22854=CARTESIAN_POINT('Ctrl Pts',(-41.6177321078719,37.0751723511041,37.9678489948478));
#22855=CARTESIAN_POINT('Ctrl Pts',(-41.6210112556406,37.0798280588501,37.9733620436181));
#22856=CARTESIAN_POINT('Ctrl Pts',(-41.6242904034094,37.084483766596,37.9788750923885));
#22857=CARTESIAN_POINT('Ctrl Pts',(-41.6275619236081,37.0891544499595,37.9843800137821));
#22858=CARTESIAN_POINT('Ctrl Pts',(-41.6308257804953,37.0938400576309,37.9898767474193));
#22859=CARTESIAN_POINT('Ctrl Pts',(-41.6340896373825,37.0985256653023,37.9953734810565));
#22860=CARTESIAN_POINT('Ctrl Pts',(-41.6373458309581,37.1032261972816,38.0008620269372));
#22861=CARTESIAN_POINT('Ctrl Pts',(-41.6405943256446,37.1079416019407,38.0063423248572));
#22862=CARTESIAN_POINT('Ctrl Pts',(-41.6438428203311,37.1126570065999,38.0118226227772));
#22863=CARTESIAN_POINT('Ctrl Pts',(-41.6470836161284,37.1173872839388,38.0172946727364));
#22864=CARTESIAN_POINT('Ctrl Pts',(-41.6503166776239,37.1221323820122,38.0227584147072));
#22865=CARTESIAN_POINT('Ctrl Pts',(-41.6535497391193,37.1268774800855,38.0282221566779));
#22866=CARTESIAN_POINT('Ctrl Pts',(-41.6567750663129,37.1316373988932,38.0336775906601));
#22867=CARTESIAN_POINT('Ctrl Pts',(-41.6599926239573,37.1364120861736,38.0391246568041));
#22868=CARTESIAN_POINT('Ctrl Pts',(-41.6632101816016,37.141186773454,38.044571722948));
#22869=CARTESIAN_POINT('Ctrl Pts',(-41.6664199696968,37.1459762292069,38.0500104212536));
#22870=CARTESIAN_POINT('Ctrl Pts',(-41.6696219531617,37.1507804008554,38.0554406920501));
#22871=CARTESIAN_POINT('Ctrl Pts',(-41.6728239366267,37.155584572504,38.0608709628466));
#22872=CARTESIAN_POINT('Ctrl Pts',(-41.6760181154612,37.1604034600481,38.066292806134));
#22873=CARTESIAN_POINT('Ctrl Pts',(-41.6792044547515,37.1652370105968,38.0717061624219));
#22874=CARTESIAN_POINT('Ctrl Pts',(-41.6823907940418,37.1700705611453,38.0771195187099));
#22875=CARTESIAN_POINT('Ctrl Pts',(-41.6855692937877,37.1749187746984,38.0825243879982));
#22876=CARTESIAN_POINT('Ctrl Pts',(-41.6887399192427,37.1797815980517,38.0879207109784));
#22877=CARTESIAN_POINT('Ctrl Pts',(-41.6919105446977,37.184644421405,38.0933170339585));
#22878=CARTESIAN_POINT('Ctrl Pts',(-41.6950732958619,37.1895218545586,38.0987048106302));
#22879=CARTESIAN_POINT('Ctrl Pts',(-41.6982281381571,37.1944138439962,38.1040839818675));
#22880=CARTESIAN_POINT('Ctrl Pts',(-41.7013829804523,37.1993058334339,38.1094631531049));
#22881=CARTESIAN_POINT('Ctrl Pts',(-41.7045299138786,37.2042123791556,38.1148337189078));
#22882=CARTESIAN_POINT('Ctrl Pts',(-41.7076689040269,37.2091334273345,38.1201956203343));
#22883=CARTESIAN_POINT('Ctrl Pts',(-41.7108078941752,37.2140544755134,38.1255575217609));
#22884=CARTESIAN_POINT('Ctrl Pts',(-41.7139389410454,37.2189900261494,38.1309107588109));
#22885=CARTESIAN_POINT('Ctrl Pts',(-41.7170620103986,37.2239400251058,38.1362552727277));
#22886=CARTESIAN_POINT('Ctrl Pts',(-41.7201850797517,37.2288900240622,38.1415997866445));
#22887=CARTESIAN_POINT('Ctrl Pts',(-41.7233001715877,37.2338544713389,38.1469355774281));
#22888=CARTESIAN_POINT('Ctrl Pts',(-41.7264072518377,37.2388333124907,38.152262586508));
#22889=CARTESIAN_POINT('Ctrl Pts',(-41.7295143320877,37.2438121536425,38.157589595588));
#22890=CARTESIAN_POINT('Ctrl Pts',(-41.7326134007518,37.2488053886693,38.1629078229643));
#22891=CARTESIAN_POINT('Ctrl Pts',(-41.7357044239324,37.2538129628184,38.1682172102543));
#22892=CARTESIAN_POINT('Ctrl Pts',(-41.5583014337907,37.0028702244532,37.8858609795071));
#22893=CARTESIAN_POINT('Ctrl Pts',(-41.5620325071846,37.0077967995883,37.8919889217062));
#22894=CARTESIAN_POINT('Ctrl Pts',(-41.565754568211,37.012741966141,37.8981074045777));
#22895=CARTESIAN_POINT('Ctrl Pts',(-41.5694675661243,37.0177056566895,37.9042163447035));
#22896=CARTESIAN_POINT('Ctrl Pts',(-41.5731772670678,37.0226649397112,37.9103198603741));
#22897=CARTESIAN_POINT('Ctrl Pts',(-41.5768779209862,37.0276427138463,37.9164138502385));
#22898=CARTESIAN_POINT('Ctrl Pts',(-41.580569477515,37.0326389113493,37.9224982313596));
#22899=CARTESIAN_POINT('Ctrl Pts',(-41.5842610340438,37.0376351088523,37.9285826124808));
#22900=CARTESIAN_POINT('Ctrl Pts',(-41.5879434931829,37.042649729723,37.9346573848587));
#22901=CARTESIAN_POINT('Ctrl Pts',(-41.5916168048155,37.0476827057143,37.9407224658179));
#22902=CARTESIAN_POINT('Ctrl Pts',(-41.595290116448,37.0527156817056,37.9467875467772));
#22903=CARTESIAN_POINT('Ctrl Pts',(-41.5989542805739,37.0577670128175,37.9528429363176));
#22904=CARTESIAN_POINT('Ctrl Pts',(-41.6026092473254,37.0628366303032,37.9588885520279));
#22905=CARTESIAN_POINT('Ctrl Pts',(-41.6062642140768,37.067906247789,37.9649341677381));
#22906=CARTESIAN_POINT('Ctrl Pts',(-41.6099099834537,37.0729941516485,37.9709700096178));
#22907=CARTESIAN_POINT('Ctrl Pts',(-41.6135465058385,37.0781002726373,37.9769959955217));
#22908=CARTESIAN_POINT('Ctrl Pts',(-41.6171830282233,37.0832063936262,37.9830219814256));
#22909=CARTESIAN_POINT('Ctrl Pts',(-41.6208103036159,37.0883307317442,37.9890381113535));
#22910=CARTESIAN_POINT('Ctrl Pts',(-41.6244282826505,37.0934732172512,37.9950443034281));
#22911=CARTESIAN_POINT('Ctrl Pts',(-41.6280462616851,37.0986157027582,38.0010504955027));
#22912=CARTESIAN_POINT('Ctrl Pts',(-41.6316549443616,37.103776335654,38.0070467497239));
#22913=CARTESIAN_POINT('Ctrl Pts',(-41.6352542815672,37.1089550457045,38.013032984485));
#22914=CARTESIAN_POINT('Ctrl Pts',(-41.6388536187729,37.1141337557549,38.0190192192461));
#22915=CARTESIAN_POINT('Ctrl Pts',(-41.6424436105076,37.1193305429598,38.0249954345469));
#22916=CARTESIAN_POINT('Ctrl Pts',(-41.646024207913,37.1245453365929,38.0309615490536));
#22917=CARTESIAN_POINT('Ctrl Pts',(-41.6496048053184,37.129760130226,38.0369276635602));
#22918=CARTESIAN_POINT('Ctrl Pts',(-41.6531760083943,37.1349929302873,38.0428836772724));
#22919=CARTESIAN_POINT('Ctrl Pts',(-41.656737768538,37.1402436655602,38.0488295091312));
#22920=CARTESIAN_POINT('Ctrl Pts',(-41.6602995286818,37.1454944008331,38.0547753409901));
#22921=CARTESIAN_POINT('Ctrl Pts',(-41.6638518458934,37.1507630713176,38.0607109909953));
#22922=CARTESIAN_POINT('Ctrl Pts',(-41.6673946718271,37.1560496053091,38.0666363783651));
#22923=CARTESIAN_POINT('Ctrl Pts',(-41.6709374977608,37.1613361393005,38.0725617657349));
#22924=CARTESIAN_POINT('Ctrl Pts',(-41.6744708324165,37.1666405367989,38.0784768904691));
#22925=CARTESIAN_POINT('Ctrl Pts',(-41.6779946277069,37.1719627256134,38.084381672065));
#22926=CARTESIAN_POINT('Ctrl Pts',(-41.6815184229973,37.1772849144277,38.0902864536611));
#22927=CARTESIAN_POINT('Ctrl Pts',(-41.6850326789224,37.1826248945581,38.0961808921187));
#22928=CARTESIAN_POINT('Ctrl Pts',(-41.6885373476544,37.1879825933294,38.102064907217));
#22929=CARTESIAN_POINT('Ctrl Pts',(-41.6920420163864,37.1933402921006,38.1079489223154));
#22930=CARTESIAN_POINT('Ctrl Pts',(-41.6955370979252,37.1987157095126,38.1138225140541));
#22931=CARTESIAN_POINT('Ctrl Pts',(-41.6990225447042,37.2041087724079,38.1196856024962));
#22932=CARTESIAN_POINT('Ctrl Pts',(-41.7025079914833,37.2095018353033,38.1255486909382));
#22933=CARTESIAN_POINT('Ctrl Pts',(-41.7059838035024,37.2149125436819,38.1314012760832));
#22934=CARTESIAN_POINT('Ctrl Pts',(-41.7094499334571,37.2203408239061,38.1372432782799));
#22935=CARTESIAN_POINT('Ctrl Pts',(-41.7129160634118,37.2257691041303,38.1430852804766));
#22936=CARTESIAN_POINT('Ctrl Pts',(-41.7163725113021,37.2312149562,38.1489166997247));
#22937=CARTESIAN_POINT('Ctrl Pts',(-41.7198192300869,37.2366783059992,38.154737456661));
#22938=CARTESIAN_POINT('Ctrl Pts',(-41.7232659488718,37.2421416557985,38.1605582135972));
#22939=CARTESIAN_POINT('Ctrl Pts',(-41.7267029385512,37.2476225033271,38.1663683082215));
#22940=CARTESIAN_POINT('Ctrl Pts',(-41.730130152349,37.2531207739928,38.1721676614605));
#22941=CARTESIAN_POINT('Ctrl Pts',(-41.5353141088974,36.9810708931059,37.8649176028963));
#22942=CARTESIAN_POINT('Ctrl Pts',(-41.5394336827557,36.9863849483897,37.8715914201543));
#22943=CARTESIAN_POINT('Ctrl Pts',(-41.5435427281318,36.9917209818238,37.878254216852));
#22944=CARTESIAN_POINT('Ctrl Pts',(-41.5476411800214,36.9970789087236,37.884905887385));
#22945=CARTESIAN_POINT('Ctrl Pts',(-41.551735992676,37.002432078033,37.8915516515433));
#22946=CARTESIAN_POINT('Ctrl Pts',(-41.5558202306487,37.0078071019442,37.8981863092869));
#22947=CARTESIAN_POINT('Ctrl Pts',(-41.5598938294398,37.013203895314,37.9048097556403));
#22948=CARTESIAN_POINT('Ctrl Pts',(-41.5639674282308,37.0186006886838,37.9114332019936));
#22949=CARTESIAN_POINT('Ctrl Pts',(-41.5680303878402,37.0240192515119,37.9180454369566));
#22950=CARTESIAN_POINT('Ctrl Pts',(-41.5720826441015,37.0294594979738,37.9246463559051));
#22951=CARTESIAN_POINT('Ctrl Pts',(-41.5761349003628,37.0348997444356,37.9312472748536));
#22952=CARTESIAN_POINT('Ctrl Pts',(-41.580176453276,37.0403616745309,37.9378368777876));
#22953=CARTESIAN_POINT('Ctrl Pts',(-41.5842072390102,37.0458452017564,37.9444150604376));
#22954=CARTESIAN_POINT('Ctrl Pts',(-41.5882380247443,37.0513287289819,37.9509932430877));
#22955=CARTESIAN_POINT('Ctrl Pts',(-41.5922580432993,37.0568338533374,37.9575600054536));
#22956=CARTESIAN_POINT('Ctrl Pts',(-41.5962672311817,37.0623604876437,37.9641152436242));
#22957=CARTESIAN_POINT('Ctrl Pts',(-41.6002764190641,37.06788712195,37.9706704817948));
#22958=CARTESIAN_POINT('Ctrl Pts',(-41.6042747762737,37.0734352662068,37.9772141957697));
#22959=CARTESIAN_POINT('Ctrl Pts',(-41.6082622396564,37.0790048325617,37.9837462819989));
#22960=CARTESIAN_POINT('Ctrl Pts',(-41.6122497030391,37.0845743989165,37.9902783682281));
#22961=CARTESIAN_POINT('Ctrl Pts',(-41.6162262725948,37.0901653873693,37.9967988267113));
#22962=CARTESIAN_POINT('Ctrl Pts',(-41.6201918855106,37.0957777093968,38.0033075542628));
#22963=CARTESIAN_POINT('Ctrl Pts',(-41.6241574984265,37.1013900314243,38.0098162818142));
#22964=CARTESIAN_POINT('Ctrl Pts',(-41.6281121547024,37.1070236870264,38.0163132784337));
#22965=CARTESIAN_POINT('Ctrl Pts',(-41.6320557918687,37.1126785870122,38.0227984413031));
#22966=CARTESIAN_POINT('Ctrl Pts',(-41.6359994290351,37.1183334869982,38.0292836041724));
#22967=CARTESIAN_POINT('Ctrl Pts',(-41.6399320470917,37.1240096313677,38.0357569332913));
#22968=CARTESIAN_POINT('Ctrl Pts',(-41.6438535839144,37.1297069302649,38.0422183262124));
#22969=CARTESIAN_POINT('Ctrl Pts',(-41.647775120737,37.1354042291623,38.0486797191335));
#22970=CARTESIAN_POINT('Ctrl Pts',(-41.6516855763256,37.141122682587,38.0551291758567));
#22971=CARTESIAN_POINT('Ctrl Pts',(-41.6555848889026,37.1468622000214,38.0615665943083));
#22972=CARTESIAN_POINT('Ctrl Pts',(-41.6594842014798,37.1526017174557,38.06800401276));
#22973=CARTESIAN_POINT('Ctrl Pts',(-41.6633723710453,37.1583622988995,38.0744293929399));
#22974=CARTESIAN_POINT('Ctrl Pts',(-41.6672493361711,37.164143853175,38.0808426331518));
#22975=CARTESIAN_POINT('Ctrl Pts',(-41.6711263012969,37.1699254074505,38.0872558733636));
#22976=CARTESIAN_POINT('Ctrl Pts',(-41.6749920619829,37.1757279345577,38.0936569736073));
#22977=CARTESIAN_POINT('Ctrl Pts',(-41.6788465571516,37.1815513426625,38.1000458325666));
#22978=CARTESIAN_POINT('Ctrl Pts',(-41.6827010523204,37.1873747507672,38.1064346915258));
#22979=CARTESIAN_POINT('Ctrl Pts',(-41.6865442819719,37.1932190398695,38.1128113092005));
#22980=CARTESIAN_POINT('Ctrl Pts',(-41.6903761853817,37.1990841174813,38.119175584658));
#22981=CARTESIAN_POINT('Ctrl Pts',(-41.6942080887914,37.2049491950931,38.1255398601155));
#22982=CARTESIAN_POINT('Ctrl Pts',(-41.6980286659593,37.2108350612144,38.1318917933555));
#22983=CARTESIAN_POINT('Ctrl Pts',(-41.7018378565156,37.2167416227065,38.1382312838321));
#22984=CARTESIAN_POINT('Ctrl Pts',(-41.7056470470719,37.2226481841985,38.1445707743086));
#22985=CARTESIAN_POINT('Ctrl Pts',(-41.7094448510165,37.2285754410611,38.1508978220214));
#22986=CARTESIAN_POINT('Ctrl Pts',(-41.7132312083362,37.2345232995077,38.1572123268139));
#22987=CARTESIAN_POINT('Ctrl Pts',(-41.7170175656559,37.2404711579544,38.1635268316065));
#22988=CARTESIAN_POINT('Ctrl Pts',(-41.7207924763506,37.2464396179848,38.1698287934786));
#22989=CARTESIAN_POINT('Ctrl Pts',(-41.7245558807656,37.2524285851673,38.1761181126667));
#22990=CARTESIAN_POINT('Ctrl Pts',(-41.5119116205319,36.9596544812705,37.8441194560785));
#22991=CARTESIAN_POINT('Ctrl Pts',(-41.5164318225131,36.9653413393433,37.8513397802637));
#22992=CARTESIAN_POINT('Ctrl Pts',(-41.5209398144549,36.9710540452047,37.8585473625558));
#22993=CARTESIAN_POINT('Ctrl Pts',(-41.5254355129223,36.9767924926594,37.8657420692341));
#22994=CARTESIAN_POINT('Ctrl Pts',(-41.5299272194183,36.9825258446392,37.8729303873468));
#22995=CARTESIAN_POINT('Ctrl Pts',(-41.534406654262,36.9882848925176,37.8801058527013));
#22996=CARTESIAN_POINT('Ctrl Pts',(-41.5388737346897,36.9940695294441,37.8872683324032));
#22997=CARTESIAN_POINT('Ctrl Pts',(-41.5433408151174,36.9998541663706,37.8944308121051));
#22998=CARTESIAN_POINT('Ctrl Pts',(-41.5477955411289,37.0056643923449,37.9015803061543));
#22999=CARTESIAN_POINT('Ctrl Pts',(-41.5522378304123,37.0115000995826,37.908716682132));
#23000=CARTESIAN_POINT('Ctrl Pts',(-41.5566801196957,37.0173358068204,37.9158530581097));
#23001=CARTESIAN_POINT('Ctrl Pts',(-41.561109972251,37.0231969953212,37.9229763160157));
#23002=CARTESIAN_POINT('Ctrl Pts',(-41.5655273062213,37.029083556371,37.9300863239114));
#23003=CARTESIAN_POINT('Ctrl Pts',(-41.5699446401916,37.0349701174208,37.9371963318071));
#23004=CARTESIAN_POINT('Ctrl Pts',(-41.5743494555768,37.0408820510191,37.9442930896923));
#23005=CARTESIAN_POINT('Ctrl Pts',(-41.5787416709781,37.0468192475256,37.9513764661133));
#23006=CARTESIAN_POINT('Ctrl Pts',(-41.5831338863793,37.0527564440322,37.9584598425344));
#23007=CARTESIAN_POINT('Ctrl Pts',(-41.5875135017965,37.0587189034466,37.965529837491));
#23008=CARTESIAN_POINT('Ctrl Pts',(-41.5918804362916,37.0647065152065,37.9725863200193));
#23009=CARTESIAN_POINT('Ctrl Pts',(-41.5962473707868,37.0706941269664,37.9796428025476));
#23010=CARTESIAN_POINT('Ctrl Pts',(-41.6006016243598,37.0767068910715,37.9866857726473));
#23011=CARTESIAN_POINT('Ctrl Pts',(-41.6049431165364,37.082744696041,37.9937150998487));
#23012=CARTESIAN_POINT('Ctrl Pts',(-41.609284608713,37.0887825010107,38.0007444270501));
#23013=CARTESIAN_POINT('Ctrl Pts',(-41.6136133394932,37.0948453468446,38.007760111353));
#23014=CARTESIAN_POINT('Ctrl Pts',(-41.6179292288694,37.1009331211479,38.0147620227869));
#23015=CARTESIAN_POINT('Ctrl Pts',(-41.6222451182455,37.1070208954514,38.0217639342208));
#23016=CARTESIAN_POINT('Ctrl Pts',(-41.6265481662175,37.1131335982241,38.0287520727853));
#23017=CARTESIAN_POINT('Ctrl Pts',(-41.6308382932475,37.1192711161612,38.0357263090137));
#23018=CARTESIAN_POINT('Ctrl Pts',(-41.6351284202774,37.1254086340983,38.042700545242));
#23019=CARTESIAN_POINT('Ctrl Pts',(-41.639405626365,37.1315709671997,38.0496608791339));
#23020=CARTESIAN_POINT('Ctrl Pts',(-41.6436698324448,37.1377580012544,38.0566071817309));
#23021=CARTESIAN_POINT('Ctrl Pts',(-41.6479340385245,37.1439450353091,38.0635534843278));
#23022=CARTESIAN_POINT('Ctrl Pts',(-41.6521852445963,37.1501567703169,38.0704857556296));
#23023=CARTESIAN_POINT('Ctrl Pts',(-41.6564233720695,37.1563930911652,38.0774038671906));
#23024=CARTESIAN_POINT('Ctrl Pts',(-41.6606614995428,37.1626294120135,38.0843219787517));
#23025=CARTESIAN_POINT('Ctrl Pts',(-41.6648865484175,37.1688903187019,38.0912259305717));
#23026=CARTESIAN_POINT('Ctrl Pts',(-41.6690984405812,37.17517569522,38.0981155947229));
#23027=CARTESIAN_POINT('Ctrl Pts',(-41.673310332745,37.1814610717381,38.1050052588741));
#23028=CARTESIAN_POINT('Ctrl Pts',(-41.6775090681976,37.1877709180856,38.1118806353562));
#23029=CARTESIAN_POINT('Ctrl Pts',(-41.6816945693075,37.1941051173586,38.1187415967635));
#23030=CARTESIAN_POINT('Ctrl Pts',(-41.6858800704174,37.2004393166314,38.1256025581708));
#23031=CARTESIAN_POINT('Ctrl Pts',(-41.6900523371845,37.2067978688295,38.132449104503));
#23032=CARTESIAN_POINT('Ctrl Pts',(-41.6942112924608,37.2131806561592,38.1392811088814));
#23033=CARTESIAN_POINT('Ctrl Pts',(-41.6983702477371,37.2195634434889,38.1461131132597));
#23034=CARTESIAN_POINT('Ctrl Pts',(-41.7025158915224,37.22597046595,38.1529305756838));
#23035=CARTESIAN_POINT('Ctrl Pts',(-41.7066481471553,37.2324016048639,38.1597333698063));
#23036=CARTESIAN_POINT('Ctrl Pts',(-41.7107804027881,37.2388327437779,38.1665361639287));
#23037=CARTESIAN_POINT('Ctrl Pts',(-41.7148992702682,37.2452879991444,38.1733242897491));
#23038=CARTESIAN_POINT('Ctrl Pts',(-41.7190046734231,37.2517672514041,38.1800976214559));
#23039=CARTESIAN_POINT('Ctrl Pts',(-41.4883731457974,36.9388425395209,37.8236917716039));
#23040=CARTESIAN_POINT('Ctrl Pts',(-41.4932995733036,36.944883604912,37.8314537588732));
#23041=CARTESIAN_POINT('Ctrl Pts',(-41.4982119888981,36.950954823534,37.8392011713985));
#23042=CARTESIAN_POINT('Ctrl Pts',(-41.5031102855784,36.9570560631423,37.8469338404252));
#23043=CARTESIAN_POINT('Ctrl Pts',(-41.5080042327986,36.9631518851332,37.8546596432006));
#23044=CARTESIAN_POINT('Ctrl Pts',(-41.5128840861671,36.9692776748191,37.8623707286484));
#23045=CARTESIAN_POINT('Ctrl Pts',(-41.5177497395788,36.9754332990042,37.8700669291027));
#23046=CARTESIAN_POINT('Ctrl Pts',(-41.5226153929905,36.9815889231893,37.877763129557));
#23047=CARTESIAN_POINT('Ctrl Pts',(-41.5274668464452,36.9877743818732,37.8854444450174));
#23048=CARTESIAN_POINT('Ctrl Pts',(-41.5323039944555,36.9939895405628,37.8931107084654));
#23049=CARTESIAN_POINT('Ctrl Pts',(-41.5371411424658,37.0002046992523,37.9007769719134));
#23050=CARTESIAN_POINT('Ctrl Pts',(-41.5419639850314,37.0064495579469,37.9084281833486));
#23051=CARTESIAN_POINT('Ctrl Pts',(-41.546772417287,37.0127239808619,37.9160641764072));
#23052=CARTESIAN_POINT('Ctrl Pts',(-41.5515808495426,37.0189984037769,37.9237001694659));
#23053=CARTESIAN_POINT('Ctrl Pts',(-41.5563748714879,37.0253023909118,37.9313209441474));
#23054=CARTESIAN_POINT('Ctrl Pts',(-41.5611543788843,37.0316358051961,37.9389263347498));
#23055=CARTESIAN_POINT('Ctrl Pts',(-41.5659338862806,37.0379692194805,37.9465317253522));
#23056=CARTESIAN_POINT('Ctrl Pts',(-41.5706988791277,37.0443320609139,37.954121731875));
#23057=CARTESIAN_POINT('Ctrl Pts',(-41.5754492538182,37.050724191146,37.9616961892852));
#23058=CARTESIAN_POINT('Ctrl Pts',(-41.5801996285086,37.0571163213783,37.9692706466953));
#23059=CARTESIAN_POINT('Ctrl Pts',(-41.5849353850422,37.0635377404088,37.9768295549925));
#23060=CARTESIAN_POINT('Ctrl Pts',(-41.5896564204469,37.0699883086141,37.9843727498196));
#23061=CARTESIAN_POINT('Ctrl Pts',(-41.5943774558517,37.0764388768193,37.9919159446468));
#23062=CARTESIAN_POINT('Ctrl Pts',(-41.5990837701275,37.0829185941986,37.9994434260036));
#23063=CARTESIAN_POINT('Ctrl Pts',(-41.6037752609427,37.0894273198606,38.0069550302165));
#23064=CARTESIAN_POINT('Ctrl Pts',(-41.6084667517579,37.0959360455226,38.0144666344295));
#23065=CARTESIAN_POINT('Ctrl Pts',(-41.6131434191123,37.1024737794668,38.021962361498));
#23066=CARTESIAN_POINT('Ctrl Pts',(-41.6178051613189,37.1090403795404,38.0294420484391));
#23067=CARTESIAN_POINT('Ctrl Pts',(-41.6224669035254,37.115606979614,38.0369217353803));
#23068=CARTESIAN_POINT('Ctrl Pts',(-41.6271137205839,37.1222024458164,38.0443853821936));
#23069=CARTESIAN_POINT('Ctrl Pts',(-41.6317455114564,37.1288266347395,38.0518328265934));
#23070=CARTESIAN_POINT('Ctrl Pts',(-41.6363773023289,37.1354508236625,38.0592802709933));
#23071=CARTESIAN_POINT('Ctrl Pts',(-41.6409940670151,37.1421037353058,38.0667115129793));
#23072=CARTESIAN_POINT('Ctrl Pts',(-41.6455957051307,37.1487852250119,38.0741263909705));
#23073=CARTESIAN_POINT('Ctrl Pts',(-41.6501973432462,37.155466714718,38.0815412689617));
#23074=CARTESIAN_POINT('Ctrl Pts',(-41.6547838547908,37.1621767824866,38.0889397829577));
#23075=CARTESIAN_POINT('Ctrl Pts',(-41.6593551400376,37.1689152824175,38.0963217720891));
#23076=CARTESIAN_POINT('Ctrl Pts',(-41.6639264252845,37.1756537823485,38.1037037612205));
#23077=CARTESIAN_POINT('Ctrl Pts',(-41.6684824842335,37.1824207144413,38.1110692254869));
#23078=CARTESIAN_POINT('Ctrl Pts',(-41.6730232178201,37.1892159315596,38.1184180047376));
#23079=CARTESIAN_POINT('Ctrl Pts',(-41.6775639514066,37.1960111486779,38.1257667839883));
#23080=CARTESIAN_POINT('Ctrl Pts',(-41.6820893596305,37.2028346508212,38.1330988782228));
#23081=CARTESIAN_POINT('Ctrl Pts',(-41.6865993440937,37.2096862896228,38.140414128016));
#23082=CARTESIAN_POINT('Ctrl Pts',(-41.6911093285568,37.2165379284245,38.1477293778093));
#23083=CARTESIAN_POINT('Ctrl Pts',(-41.6956038892589,37.2234177038842,38.1550277831608));
#23084=CARTESIAN_POINT('Ctrl Pts',(-41.7000829284727,37.2303254664117,38.162309185378));
#23085=CARTESIAN_POINT('Ctrl Pts',(-41.7045619676864,37.2372332289392,38.1695905875952));
#23086=CARTESIAN_POINT('Ctrl Pts',(-41.7090254854116,37.2441689785342,38.1768549866776));
#23087=CARTESIAN_POINT('Ctrl Pts',(-41.7134733845959,37.2511325643894,38.184102224672));
#23088=CARTESIAN_POINT('Ctrl Pts',(-41.4648346710629,36.9180305977713,37.8032640871294));
#23089=CARTESIAN_POINT('Ctrl Pts',(-41.4701673240942,36.9244258704808,37.8115677374827));
#23090=CARTESIAN_POINT('Ctrl Pts',(-41.4754841633414,36.9308556018634,37.8198549802413));
#23091=CARTESIAN_POINT('Ctrl Pts',(-41.4807850582345,36.9373196336253,37.8281256116162));
#23092=CARTESIAN_POINT('Ctrl Pts',(-41.486081246179,36.9437779256271,37.8363888990545));
#23093=CARTESIAN_POINT('Ctrl Pts',(-41.4913615180722,36.9502704571205,37.8446356045956));
#23094=CARTESIAN_POINT('Ctrl Pts',(-41.4966257444679,36.9567970685643,37.8528655258022));
#23095=CARTESIAN_POINT('Ctrl Pts',(-41.5018899708636,36.963323680008,37.8610954470088));
#23096=CARTESIAN_POINT('Ctrl Pts',(-41.5071381517616,36.9698843714016,37.8693085838804));
#23097=CARTESIAN_POINT('Ctrl Pts',(-41.5123701584987,36.9764789815429,37.8775047347988));
#23098=CARTESIAN_POINT('Ctrl Pts',(-41.5176021652359,36.9830735916842,37.8857008857171));
#23099=CARTESIAN_POINT('Ctrl Pts',(-41.5228179978118,36.9897021205725,37.8938800506816));
#23100=CARTESIAN_POINT('Ctrl Pts',(-41.5280175283527,36.9963644053527,37.9020420289031));
#23101=CARTESIAN_POINT('Ctrl Pts',(-41.5332170588936,37.003026690133,37.9102040071246));
#23102=CARTESIAN_POINT('Ctrl Pts',(-41.538400287399,37.0097227308045,37.9183487986025));
#23103=CARTESIAN_POINT('Ctrl Pts',(-41.5435670867904,37.0164523628666,37.9264762033862));
#23104=CARTESIAN_POINT('Ctrl Pts',(-41.5487338861819,37.0231819949288,37.93460360817));
#23105=CARTESIAN_POINT('Ctrl Pts',(-41.553884256459,37.029945218381,37.9427136262589));
#23106=CARTESIAN_POINT('Ctrl Pts',(-41.5590180713448,37.0367418670856,37.950806058551));
#23107=CARTESIAN_POINT('Ctrl Pts',(-41.5641518862305,37.0435385157901,37.9588984908431));
#23108=CARTESIAN_POINT('Ctrl Pts',(-41.5692691457245,37.0503685897463,37.9669733373377));
#23109=CARTESIAN_POINT('Ctrl Pts',(-41.5743697243575,37.0572319211871,37.9750303997906));
#23110=CARTESIAN_POINT('Ctrl Pts',(-41.5794703029904,37.0640952526279,37.9830874622435));
#23111=CARTESIAN_POINT('Ctrl Pts',(-41.5845542007618,37.0709918415526,37.9911267406543));
#23112=CARTESIAN_POINT('Ctrl Pts',(-41.5896212930161,37.0779215185733,37.9991480376462));
#23113=CARTESIAN_POINT('Ctrl Pts',(-41.5946883852703,37.0848511955938,38.0071693346381));
#23114=CARTESIAN_POINT('Ctrl Pts',(-41.599738672007,37.0918139607097,38.0151726502107));
#23115=CARTESIAN_POINT('Ctrl Pts',(-41.6047720293902,37.0988096429197,38.0231577878646));
#23116=CARTESIAN_POINT('Ctrl Pts',(-41.6098053867735,37.1058053251296,38.0311429255186));
#23117=CARTESIAN_POINT('Ctrl Pts',(-41.6148218148028,37.1128339244332,38.0391098852532));
#23118=CARTESIAN_POINT('Ctrl Pts',(-41.619821190468,37.1198952682246,38.047058471456));
#23119=CARTESIAN_POINT('Ctrl Pts',(-41.6248205661333,37.1269566120159,38.0550070576587));
#23120=CARTESIAN_POINT('Ctrl Pts',(-41.629802889434,37.1340507002946,38.062937270329));
#23121=CARTESIAN_POINT('Ctrl Pts',(-41.6347680381918,37.1411773588585,38.0708489147504));
#23122=CARTESIAN_POINT('Ctrl Pts',(-41.6397331869496,37.1483040174226,38.0787605591718));
#23123=CARTESIAN_POINT('Ctrl Pts',(-41.644681161164,37.1554632462713,38.0866536353436));
#23124=CARTESIAN_POINT('Ctrl Pts',(-41.649611839494,37.1626548696151,38.0945279494552));
#23125=CARTESIAN_POINT('Ctrl Pts',(-41.6545425178241,37.1698464929588,38.1024022635669));
#23126=CARTESIAN_POINT('Ctrl Pts',(-41.6594559002695,37.177070510797,38.1102578156176));
#23127=CARTESIAN_POINT('Ctrl Pts',(-41.6643518663326,37.1843267457607,38.1180944127116));
#23128=CARTESIAN_POINT('Ctrl Pts',(-41.6692478323959,37.1915829807243,38.1259310098057));
#23129=CARTESIAN_POINT('Ctrl Pts',(-41.6741263820765,37.1988714328129,38.1337486519425));
#23130=CARTESIAN_POINT('Ctrl Pts',(-41.6789873957265,37.2061919230865,38.1415471471507));
#23131=CARTESIAN_POINT('Ctrl Pts',(-41.6838484093764,37.2135124133602,38.1493456423588));
#23132=CARTESIAN_POINT('Ctrl Pts',(-41.6886918869953,37.2208649418183,38.1571249906378));
#23133=CARTESIAN_POINT('Ctrl Pts',(-41.69351770979,37.2282493279595,38.1648850009497));
#23134=CARTESIAN_POINT('Ctrl Pts',(-41.6983435325848,37.2356337141006,38.1726450112617));
#23135=CARTESIAN_POINT('Ctrl Pts',(-41.703151700555,37.243049957924,38.180385683606));
#23136=CARTESIAN_POINT('Ctrl Pts',(-41.7079420957686,37.2504978773748,38.1881068278881));
#23137=CARTESIAN_POINT('Ctrl Pts',(-41.4411625260449,36.8978229684399,37.7832073884005));
#23138=CARTESIAN_POINT('Ctrl Pts',(-41.4469069412086,36.9045538788403,37.7920478342999));
#23139=CARTESIAN_POINT('Ctrl Pts',(-41.4526336212004,36.9113239876996,37.8008699290073));
#23140=CARTESIAN_POINT('Ctrl Pts',(-41.4583424066575,36.9181331060726,37.8096734267128));
#23141=CARTESIAN_POINT('Ctrl Pts',(-41.464046122978,36.9249361782645,37.8184691073211));
#23142=CARTESIAN_POINT('Ctrl Pts',(-41.4697319765726,36.9317781907605,37.8272462239758));
#23143=CARTESIAN_POINT('Ctrl Pts',(-41.4753998095769,36.9386589530465,37.8360045326208));
#23144=CARTESIAN_POINT('Ctrl Pts',(-41.4810676425811,36.9455397153324,37.8447628412659));
#23145=CARTESIAN_POINT('Ctrl Pts',(-41.4867174549946,36.9524592274075,37.8535023419004));
#23146=CARTESIAN_POINT('Ctrl Pts',(-41.4923490899483,36.9594172966217,37.8622227915074));
#23147=CARTESIAN_POINT('Ctrl Pts',(-41.4979807249019,36.9663753658359,37.8709432411143));
#23148=CARTESIAN_POINT('Ctrl Pts',(-41.5035941823952,36.9733719921884,37.8796446396928));
#23149=CARTESIAN_POINT('Ctrl Pts',(-41.5091893065629,36.9804069809039,37.8883267452782));
#23150=CARTESIAN_POINT('Ctrl Pts',(-41.5147844307306,36.9874419696193,37.8970088508636));
#23151=CARTESIAN_POINT('Ctrl Pts',(-41.5203612215722,36.9945153206969,37.905671663455));
#23152=CARTESIAN_POINT('Ctrl Pts',(-41.5259195242348,37.0016268372465,37.9143149421534));
#23153=CARTESIAN_POINT('Ctrl Pts',(-41.5314778268974,37.0087383537961,37.9229582208518));
#23154=CARTESIAN_POINT('Ctrl Pts',(-41.5370176413805,37.0158880358169,37.9315819656562));
#23155=CARTESIAN_POINT('Ctrl Pts',(-41.542538813852,37.0230756843147,37.9401859367464));
#23156=CARTESIAN_POINT('Ctrl Pts',(-41.5480599863234,37.0302633328126,37.9487899078366));
#23157=CARTESIAN_POINT('Ctrl Pts',(-41.5535625167827,37.0374889477867,37.9573741052116));
#23158=CARTESIAN_POINT('Ctrl Pts',(-41.5590462524268,37.0447523281498,37.9659382901431));
#23159=CARTESIAN_POINT('Ctrl Pts',(-41.5645299880708,37.052015708513,37.9745024750745));
#23160=CARTESIAN_POINT('Ctrl Pts',(-41.5699949288992,37.0593168542644,37.9830466475614));
#23161=CARTESIAN_POINT('Ctrl Pts',(-41.5754409231463,37.0666555622348,37.9915705699802));
#23162=CARTESIAN_POINT('Ctrl Pts',(-41.5808869173934,37.0739942702052,38.000094492399));
#23163=CARTESIAN_POINT('Ctrl Pts',(-41.5863139650587,37.0813705403938,38.0085981647488));
#23164=CARTESIAN_POINT('Ctrl Pts',(-41.5917219154225,37.0887841675603,38.017081350524));
#23165=CARTESIAN_POINT('Ctrl Pts',(-41.5971298657864,37.0961977947268,38.0255645362992));
#23166=CARTESIAN_POINT('Ctrl Pts',(-41.6025187188481,37.1036487788704,38.0340272354987));
#23167=CARTESIAN_POINT('Ctrl Pts',(-41.607888324942,37.111136912691,38.0424692127479));
#23168=CARTESIAN_POINT('Ctrl Pts',(-41.613257931036,37.1186250465116,38.050911189997));
#23169=CARTESIAN_POINT('Ctrl Pts',(-41.6186082901615,37.1261503300086,38.0593324452947));
#23170=CARTESIAN_POINT('Ctrl Pts',(-41.623939253715,37.1337125538333,38.0677327444099));
#23171=CARTESIAN_POINT('Ctrl Pts',(-41.6292702172685,37.1412747776581,38.0761330435249));
#23172=CARTESIAN_POINT('Ctrl Pts',(-41.6345817852494,37.1488739418099,38.0845123864566));
#23173=CARTESIAN_POINT('Ctrl Pts',(-41.6398738101244,37.1565098349032,38.09287054013));
#23174=CARTESIAN_POINT('Ctrl Pts',(-41.6451658349994,37.1641457279966,38.1012286938033));
#23175=CARTESIAN_POINT('Ctrl Pts',(-41.6504383167679,37.1718183500307,38.1095656582175));
#23176=CARTESIAN_POINT('Ctrl Pts',(-41.6556911089748,37.1795274875948,38.1178812014669));
#23177=CARTESIAN_POINT('Ctrl Pts',(-41.6609439011816,37.1872366251589,38.1261967447164));
#23178=CARTESIAN_POINT('Ctrl Pts',(-41.6661770038263,37.1949822782522,38.1344908668002));
#23179=CARTESIAN_POINT('Ctrl Pts',(-41.6713902715401,37.2027642314499,38.1427633369947));
#23180=CARTESIAN_POINT('Ctrl Pts',(-41.6766035392538,37.2105461846477,38.1510358071891));
#23181=CARTESIAN_POINT('Ctrl Pts',(-41.6817969720361,37.2183644379491,38.1592866254934));
#23182=CARTESIAN_POINT('Ctrl Pts',(-41.6869704256122,37.2262187739276,38.1675155623782));
#23183=CARTESIAN_POINT('Ctrl Pts',(-41.6921438791884,37.2340731099062,38.175744499263));
#23184=CARTESIAN_POINT('Ctrl Pts',(-41.6972973535554,37.241963528558,38.1839515547247));
#23185=CARTESIAN_POINT('Ctrl Pts',(-41.7024307055465,37.2498898104733,38.1921365004474));
#23186=CARTESIAN_POINT('Ctrl Pts',(-41.4175681781877,36.8783311375915,37.7636543125594));
#23187=CARTESIAN_POINT('Ctrl Pts',(-41.4237247372187,36.8853777678676,37.7730231199949));
#23188=CARTESIAN_POINT('Ctrl Pts',(-41.4298615655738,36.8924687040171,37.7823715691034));
#23189=CARTESIAN_POINT('Ctrl Pts',(-41.4359784694956,36.8996037221832,37.7916993647842));
#23190=CARTESIAN_POINT('Ctrl Pts',(-41.4420899418905,36.9067324047845,37.8010188778155));
#23191=CARTESIAN_POINT('Ctrl Pts',(-41.448181525261,36.913905091185,37.8103177741145));
#23192=CARTESIAN_POINT('Ctrl Pts',(-41.4542530277002,36.9211215554196,37.8195957607326));
#23193=CARTESIAN_POINT('Ctrl Pts',(-41.4603245301395,36.9283380196542,37.8288737473507));
#23194=CARTESIAN_POINT('Ctrl Pts',(-41.4663759516467,36.9355982617217,37.8381308242868));
#23195=CARTESIAN_POINT('Ctrl Pts',(-41.4724071015805,36.9429020528988,37.8473666999098));
#23196=CARTESIAN_POINT('Ctrl Pts',(-41.4784382515143,36.9502058440759,37.8566025755327));
#23197=CARTESIAN_POINT('Ctrl Pts',(-41.4844491298738,36.9575531843614,37.8658172498414));
#23198=CARTESIAN_POINT('Ctrl Pts',(-41.4904395472949,36.9649438422879,37.8750104325405));
#23199=CARTESIAN_POINT('Ctrl Pts',(-41.496429964716,36.9723345002145,37.8842036152396));
#23200=CARTESIAN_POINT('Ctrl Pts',(-41.5023999211979,36.9797684757809,37.8933753063279));
#23201=CARTESIAN_POINT('Ctrl Pts',(-41.5083492286656,36.9872455347906,37.9025252168644));
#23202=CARTESIAN_POINT('Ctrl Pts',(-41.5142985361333,36.9947225938003,37.9116751274009));
#23203=CARTESIAN_POINT('Ctrl Pts',(-41.520227194586,37.0022427362521,37.9208032573843));
#23204=CARTESIAN_POINT('Ctrl Pts',(-41.5261350172497,37.0098057252348,37.9299093192459));
#23205=CARTESIAN_POINT('Ctrl Pts',(-41.5320428399134,37.0173687142174,37.9390153811075));
#23206=CARTESIAN_POINT('Ctrl Pts',(-41.5379298267874,37.0249745497298,37.9480993748461));
#23207=CARTESIAN_POINT('Ctrl Pts',(-41.5437957924105,37.0326229921609,37.9571610142833));
#23208=CARTESIAN_POINT('Ctrl Pts',(-41.5496617580337,37.0402714345921,37.9662226537206));
#23209=CARTESIAN_POINT('Ctrl Pts',(-41.5555067024051,37.0479624839409,37.9752619388553));
#23210=CARTESIAN_POINT('Ctrl Pts',(-41.5613304413883,37.055695897912,37.9842785849177));
#23211=CARTESIAN_POINT('Ctrl Pts',(-41.5671541803714,37.063429311883,37.99329523098));
#23212=CARTESIAN_POINT('Ctrl Pts',(-41.5729567139654,37.0712050904752,38.0022892379688));
#23213=CARTESIAN_POINT('Ctrl Pts',(-41.5787378593698,37.0790229887236,38.0112603225407));
#23214=CARTESIAN_POINT('Ctrl Pts',(-41.5845190047742,37.086840886972,38.0202314071125));
#23215=CARTESIAN_POINT('Ctrl Pts',(-41.5902787619881,37.0947009048757,38.0291795692662));
#23216=CARTESIAN_POINT('Ctrl Pts',(-41.5960169495586,37.102602794816,38.0381045271027));
#23217=CARTESIAN_POINT('Ctrl Pts',(-41.6017551371292,37.1105046847562,38.0470294849391));
#23218=CARTESIAN_POINT('Ctrl Pts',(-41.6074717550556,37.1184484467319,38.0559312384571));
#23219=CARTESIAN_POINT('Ctrl Pts',(-41.6131666232439,37.1264338304863,38.0648095072195));
#23220=CARTESIAN_POINT('Ctrl Pts',(-41.6188614914322,37.1344192142406,38.073687775982));
#23221=CARTESIAN_POINT('Ctrl Pts',(-41.6245346098817,37.1424462197725,38.0825425599877));
#23222=CARTESIAN_POINT('Ctrl Pts',(-41.6301857998689,37.1505145942025,38.0913735802794));
#23223=CARTESIAN_POINT('Ctrl Pts',(-41.635836989856,37.1585829686325,38.100204600571));
#23224=CARTESIAN_POINT('Ctrl Pts',(-41.64146625138,37.1666927119596,38.1090118571474));
#23225=CARTESIAN_POINT('Ctrl Pts',(-41.6470734070991,37.1748435686977,38.1177950725484));
#23226=CARTESIAN_POINT('Ctrl Pts',(-41.6526805628181,37.1829944254359,38.1265782879495));
#23227=CARTESIAN_POINT('Ctrl Pts',(-41.6582656127314,37.1911863955842,38.1353374621739));
#23228=CARTESIAN_POINT('Ctrl Pts',(-41.66382838089,37.1994192210661,38.1440723192766));
#23229=CARTESIAN_POINT('Ctrl Pts',(-41.6693911490485,37.207652046548,38.1528071763792));
#23230=CARTESIAN_POINT('Ctrl Pts',(-41.6749316354515,37.2159257273625,38.1615177163588));
#23231=CARTESIAN_POINT('Ctrl Pts',(-41.6804496655538,37.2242400028591,38.1702036648023));
#23232=CARTESIAN_POINT('Ctrl Pts',(-41.6859676956561,37.2325542783556,38.1788896132457));
#23233=CARTESIAN_POINT('Ctrl Pts',(-41.6914632694547,37.2409091485302,38.1875509701493));
#23234=CARTESIAN_POINT('Ctrl Pts',(-41.6969362138248,37.2493043501811,38.1961874626549));
#23235=CARTESIAN_POINT('Ctrl Pts',(-41.3939738303305,36.8588393067431,37.7441012367184));
#23236=CARTESIAN_POINT('Ctrl Pts',(-41.4005425332289,36.8662016568948,37.7539984056898));
#23237=CARTESIAN_POINT('Ctrl Pts',(-41.4070895099472,36.8736134203346,37.7638732091995));
#23238=CARTESIAN_POINT('Ctrl Pts',(-41.4136145323336,36.8810743382939,37.7737253028556));
#23239=CARTESIAN_POINT('Ctrl Pts',(-41.4201337608031,36.8885286313044,37.78356864831));
#23240=CARTESIAN_POINT('Ctrl Pts',(-41.4266310739494,36.8960319916095,37.7933893242532));
#23241=CARTESIAN_POINT('Ctrl Pts',(-41.4331062458236,36.9035841577927,37.8031869888444));
#23242=CARTESIAN_POINT('Ctrl Pts',(-41.4395814176978,36.9111363239759,37.8129846534356));
#23243=CARTESIAN_POINT('Ctrl Pts',(-41.4460344482988,36.918737296036,37.8227593066733));
#23244=CARTESIAN_POINT('Ctrl Pts',(-41.4524651132127,36.926386809176,37.8325106083122));
#23245=CARTESIAN_POINT('Ctrl Pts',(-41.4588957781266,36.9340363223159,37.8422619099512));
#23246=CARTESIAN_POINT('Ctrl Pts',(-41.4653040773524,36.9417343765344,37.85198985999));
#23247=CARTESIAN_POINT('Ctrl Pts',(-41.4716897880269,36.949480703672,37.8616941198028));
#23248=CARTESIAN_POINT('Ctrl Pts',(-41.4780754987014,36.9572270308095,37.8713983796156));
#23249=CARTESIAN_POINT('Ctrl Pts',(-41.4844386208236,36.9650216308649,37.8810789492008));
#23250=CARTESIAN_POINT('Ctrl Pts',(-41.4907789330963,36.9728642323347,37.8907354915754));
#23251=CARTESIAN_POINT('Ctrl Pts',(-41.4971192453691,36.9807068338045,37.90039203395));
#23252=CARTESIAN_POINT('Ctrl Pts',(-41.5034367477914,36.9885974366874,37.9100245491124));
#23253=CARTESIAN_POINT('Ctrl Pts',(-41.5097312206474,36.9965357661548,37.9196327017454));
#23254=CARTESIAN_POINT('Ctrl Pts',(-41.5160256935034,37.0044740956222,37.9292408543784));
#23255=CARTESIAN_POINT('Ctrl Pts',(-41.5222971367922,37.0124601516729,37.9388246444805));
#23256=CARTESIAN_POINT('Ctrl Pts',(-41.5285453323944,37.020493656172,37.9483837384236));
#23257=CARTESIAN_POINT('Ctrl Pts',(-41.5347935279965,37.0285271606712,37.9579428323667));
#23258=CARTESIAN_POINT('Ctrl Pts',(-41.5410184759111,37.0366081136174,37.9674772301492));
#23259=CARTESIAN_POINT('Ctrl Pts',(-41.5472199596302,37.0447362335891,37.9769865998551));
#23260=CARTESIAN_POINT('Ctrl Pts',(-41.5534214433494,37.0528643535608,37.986495969561));
#23261=CARTESIAN_POINT('Ctrl Pts',(-41.5595994628721,37.0610396405565,37.9959803111888));
#23262=CARTESIAN_POINT('Ctrl Pts',(-41.565753803317,37.0692618098869,38.0054392945573));
#23263=CARTESIAN_POINT('Ctrl Pts',(-41.5719081437619,37.0774839792173,38.0148982779259));
#23264=CARTESIAN_POINT('Ctrl Pts',(-41.5780388051281,37.0857530308811,38.0243319030337));
#23265=CARTESIAN_POINT('Ctrl Pts',(-41.5841455741753,37.0940686769409,38.0337398414575));
#23266=CARTESIAN_POINT('Ctrl Pts',(-41.5902523432224,37.1023843230008,38.0431477798813));
#23267=CARTESIAN_POINT('Ctrl Pts',(-41.5963352199497,37.1107465634554,38.0525300316195));
#23268=CARTESIAN_POINT('Ctrl Pts',(-41.6023939927728,37.1191551071392,38.0618862700293));
#23269=CARTESIAN_POINT('Ctrl Pts',(-41.608452765596,37.1275636508232,38.071242508439));
#23270=CARTESIAN_POINT('Ctrl Pts',(-41.614487434514,37.1360184977352,38.0805727335188));
#23271=CARTESIAN_POINT('Ctrl Pts',(-41.6204977896133,37.1445193535017,38.0898766204288));
#23272=CARTESIAN_POINT('Ctrl Pts',(-41.6265081447126,37.1530202092684,38.0991805073388));
#23273=CARTESIAN_POINT('Ctrl Pts',(-41.6324941859922,37.1615670738884,38.1084580560773));
#23274=CARTESIAN_POINT('Ctrl Pts',(-41.6384557052234,37.1701596498007,38.1177089436299));
#23275=CARTESIAN_POINT('Ctrl Pts',(-41.6444172244546,37.1787522257129,38.1269598311826));
#23276=CARTESIAN_POINT('Ctrl Pts',(-41.6503542216365,37.1873905129162,38.1361840575477));
#23277=CARTESIAN_POINT('Ctrl Pts',(-41.6562664902398,37.1960742106822,38.1453813015585));
#23278=CARTESIAN_POINT('Ctrl Pts',(-41.6621787588431,37.2047579084483,38.1545785455694));
#23279=CARTESIAN_POINT('Ctrl Pts',(-41.6680662988668,37.2134870167759,38.1637488072244));
#23280=CARTESIAN_POINT('Ctrl Pts',(-41.6739289054954,37.2222612317904,38.1728917672265));
#23281=CARTESIAN_POINT('Ctrl Pts',(-41.6797915121239,37.231035446805,38.1820347272285));
#23282=CARTESIAN_POINT('Ctrl Pts',(-41.6856291853541,37.2398547685024,38.1911503855738));
#23283=CARTESIAN_POINT('Ctrl Pts',(-41.6914417221031,37.2487188898889,38.2002384248625));
#23284=CARTESIAN_POINT('Ctrl Pts',(-41.3704568141619,36.8400609999701,37.7250501241905));
#23285=CARTESIAN_POINT('Ctrl Pts',(-41.3774380466235,36.8477192136434,37.7354672496683));
#23286=CARTESIAN_POINT('Ctrl Pts',(-41.3843954836192,36.8554323147081,37.7458599393064));
#23287=CARTESIAN_POINT('Ctrl Pts',(-41.3913288569572,36.8632000051908,37.7562277921192));
#23288=CARTESIAN_POINT('Ctrl Pts',(-41.3982560737816,36.8709607983251,37.7665864387599));
#23289=CARTESIAN_POINT('Ctrl Pts',(-41.4051592696763,36.8787760839841,37.7769202926724));
#23290=CARTESIAN_POINT('Ctrl Pts',(-41.4120381790331,36.8866455608354,37.7872289558619));
#23291=CARTESIAN_POINT('Ctrl Pts',(-41.4189170883898,36.8945150376866,37.7975376190515));
#23292=CARTESIAN_POINT('Ctrl Pts',(-41.4257717112071,36.9024387057288,37.8078210915159));
#23293=CARTESIAN_POINT('Ctrl Pts',(-41.4326017837395,36.9104162594787,37.8180789771934));
#23294=CARTESIAN_POINT('Ctrl Pts',(-41.4394318562719,36.9183938132286,37.8283368628709));
#23295=CARTESIAN_POINT('Ctrl Pts',(-41.4462373785179,36.9264252526848,37.8385691617593));
#23296=CARTESIAN_POINT('Ctrl Pts',(-41.453018088615,36.9345102682369,37.8487754797595));
#23297=CARTESIAN_POINT('Ctrl Pts',(-41.4597987987121,36.9425952837891,37.8589817977596));
#23298=CARTESIAN_POINT('Ctrl Pts',(-41.4665546966589,36.9507338754356,37.8691621348695));
#23299=CARTESIAN_POINT('Ctrl Pts',(-41.4732855224958,36.9589257294625,37.8793160989828));
#23300=CARTESIAN_POINT('Ctrl Pts',(-41.4800163483326,36.9671175834893,37.8894700630961));
#23301=CARTESIAN_POINT('Ctrl Pts',(-41.4867221020581,36.9753626998948,37.8995976542109));
#23302=CARTESIAN_POINT('Ctrl Pts',(-41.4934025256351,36.9836607608853,37.9096984822434));
#23303=CARTESIAN_POINT('Ctrl Pts',(-41.5000829492121,36.9919588218757,37.919799310276));
#23304=CARTESIAN_POINT('Ctrl Pts',(-41.5067380426394,37.0003098274494,37.9298733752245));
#23305=CARTESIAN_POINT('Ctrl Pts',(-41.5133675498222,37.0087134557569,37.9399202890576));
#23306=CARTESIAN_POINT('Ctrl Pts',(-41.5199970570049,37.0171170840643,37.9499672028907));
#23307=CARTESIAN_POINT('Ctrl Pts',(-41.5266009779418,37.025573335104,37.9599869656065));
#23308=CARTESIAN_POINT('Ctrl Pts',(-41.5331790584998,37.0340818829953,37.9699791912559));
#23309=CARTESIAN_POINT('Ctrl Pts',(-41.5397571390579,37.0425904308867,37.9799714169054));
#23310=CARTESIAN_POINT('Ctrl Pts',(-41.5463093792357,37.0511512756281,37.9899361054864));
#23311=CARTESIAN_POINT('Ctrl Pts',(-41.5528355268815,37.0597640873328,37.9998728731613));
#23312=CARTESIAN_POINT('Ctrl Pts',(-41.5593616745273,37.0683768990375,38.0098096408362));
#23313=CARTESIAN_POINT('Ctrl Pts',(-41.5658617296397,37.077041677704,38.0197184876031));
#23314=CARTESIAN_POINT('Ctrl Pts',(-41.5723354420671,37.0857580894643,38.0295990317648));
#23315=CARTESIAN_POINT('Ctrl Pts',(-41.5788091544946,37.0944745012246,38.0394795759265));
#23316=CARTESIAN_POINT('Ctrl Pts',(-41.5852565242357,37.1032425460772,38.0493318174811));
#23317=CARTESIAN_POINT('Ctrl Pts',(-41.5916773031583,37.1120618861987,38.0591553769012));
#23318=CARTESIAN_POINT('Ctrl Pts',(-41.598098082081,37.1208812263202,38.0689789363214));
#23319=CARTESIAN_POINT('Ctrl Pts',(-41.6044922701839,37.1297518617088,38.0787738136053));
#23320=CARTESIAN_POINT('Ctrl Pts',(-41.6108596213729,37.1386734506113,38.088539631424));
#23321=CARTESIAN_POINT('Ctrl Pts',(-41.6172269725618,37.147595039514,38.0983054492427));
#23322=CARTESIAN_POINT('Ctrl Pts',(-41.6235674868357,37.1565675819287,38.1080422075945));
#23323=CARTESIAN_POINT('Ctrl Pts',(-41.6298809201574,37.1655907321986,38.1177495313779));
#23324=CARTESIAN_POINT('Ctrl Pts',(-41.6361943534791,37.1746138824685,38.1274568551614));
#23325=CARTESIAN_POINT('Ctrl Pts',(-41.6424807058473,37.1836876405919,38.1371347443747));
#23326=CARTESIAN_POINT('Ctrl Pts',(-41.6487397353004,37.1928116570341,38.1467828261724));
#23327=CARTESIAN_POINT('Ctrl Pts',(-41.6549987647536,37.2019356734762,38.1564309079702));
#23328=CARTESIAN_POINT('Ctrl Pts',(-41.6612304712904,37.2111099482355,38.1660491823505));
#23329=CARTESIAN_POINT('Ctrl Pts',(-41.6674346150433,37.2203341279265,38.1756372787524));
#23330=CARTESIAN_POINT('Ctrl Pts',(-41.6736387587962,37.2295583076174,38.1852253751544));
#23331=CARTESIAN_POINT('Ctrl Pts',(-41.6798153397637,37.2388323922379,38.1947832935759));
#23332=CARTESIAN_POINT('Ctrl Pts',(-41.6859641201911,37.2481560245796,38.2043106657693));
#23333=CARTESIAN_POINT('Ctrl Pts',(-41.3471485981035,36.8220184082047,37.7065516748432));
#23334=CARTESIAN_POINT('Ctrl Pts',(-41.3545393602976,36.8299531375333,37.7174786109716));
#23335=CARTESIAN_POINT('Ctrl Pts',(-41.3619042218529,36.8379485277722,37.7283790161319));
#23336=CARTESIAN_POINT('Ctrl Pts',(-41.3692428685891,36.8460042378472,37.7392524253368));
#23337=CARTESIAN_POINT('Ctrl Pts',(-41.3765749989477,36.8540527948257,37.7501161794591));
#23338=CARTESIAN_POINT('Ctrl Pts',(-41.3838809610326,36.8621615645735,37.7609529855544));
#23339=CARTESIAN_POINT('Ctrl Pts',(-41.3911604437533,36.8703302018164,37.7717623821877));
#23340=CARTESIAN_POINT('Ctrl Pts',(-41.3984399264739,36.8784988390592,37.782571778821));
#23341=CARTESIAN_POINT('Ctrl Pts',(-41.4056929298286,36.8867273437952,37.7933537659895));
#23342=CARTESIAN_POINT('Ctrl Pts',(-41.4129191449819,36.8950153656514,37.8041078845926));
#23343=CARTESIAN_POINT('Ctrl Pts',(-41.4201453601353,36.9033033875077,37.8148620031957));
#23344=CARTESIAN_POINT('Ctrl Pts',(-41.4273447870854,36.9116509264823,37.8255882532307));
#23345=CARTESIAN_POINT('Ctrl Pts',(-41.4345171192782,36.9200576271341,37.8362861779701));
#23346=CARTESIAN_POINT('Ctrl Pts',(-41.441689451471,36.928464327786,37.8469841027093));
#23347=CARTESIAN_POINT('Ctrl Pts',(-41.4488346889047,36.9369301901129,37.8576537021504));
#23348=CARTESIAN_POINT('Ctrl Pts',(-41.4559525273326,36.9454548536356,37.8682945219779));
#23349=CARTESIAN_POINT('Ctrl Pts',(-41.4630703657605,36.9539795171584,37.8789353418053));
#23350=CARTESIAN_POINT('Ctrl Pts',(-41.4701608051808,36.9625629818748,37.8895473820166));
#23351=CARTESIAN_POINT('Ctrl Pts',(-41.4772235436802,36.9712048822978,37.9001301907472));
#23352=CARTESIAN_POINT('Ctrl Pts',(-41.4842862821795,36.9798467827208,37.9107129994779));
#23353=CARTESIAN_POINT('Ctrl Pts',(-41.4913213197562,36.9885471188485,37.9212665767253));
#23354=CARTESIAN_POINT('Ctrl Pts',(-41.4983283568557,36.9973055202173,37.9317904731145));
#23355=CARTESIAN_POINT('Ctrl Pts',(-41.5053353939552,37.0060639215861,37.9423143695036));
#23356=CARTESIAN_POINT('Ctrl Pts',(-41.512314430576,37.0148803881939,37.952808585032));
#23357=CARTESIAN_POINT('Ctrl Pts',(-41.5192651695481,37.0237545446324,37.9632726728521));
#23358=CARTESIAN_POINT('Ctrl Pts',(-41.5262159085202,37.0326287010711,37.9737367606722));
#23359=CARTESIAN_POINT('Ctrl Pts',(-41.5331383498419,37.0415605473383,37.9841707207815));
#23360=CARTESIAN_POINT('Ctrl Pts',(-41.5400321987533,37.0505497031129,37.9945741088983));
#23361=CARTESIAN_POINT('Ctrl Pts',(-41.5469260476646,37.0595388588875,38.0049774970151));
#23362=CARTESIAN_POINT('Ctrl Pts',(-41.553791304164,37.0685853241673,38.0153503131368));
#23363=CARTESIAN_POINT('Ctrl Pts',(-41.5606276759261,37.0776887137508,38.0256921155853));
#23364=CARTESIAN_POINT('Ctrl Pts',(-41.5674640476884,37.0867921033341,38.0360339180337));
#23365=CARTESIAN_POINT('Ctrl Pts',(-41.5742715347118,37.0959524172188,38.0463447068064));
#23366=CARTESIAN_POINT('Ctrl Pts',(-41.5810498471313,37.1051692653554,38.0566240428664));
#23367=CARTESIAN_POINT('Ctrl Pts',(-41.5878281595508,37.114386113492,38.0669033789262));
#23368=CARTESIAN_POINT('Ctrl Pts',(-41.5945772973647,37.1236594958782,38.0771512622708));
#23369=CARTESIAN_POINT('Ctrl Pts',(-41.6012969731922,37.1329890176503,38.0873672565416));
#23370=CARTESIAN_POINT('Ctrl Pts',(-41.6080166490197,37.1423185394222,38.0975832508123));
#23371=CARTESIAN_POINT('Ctrl Pts',(-41.6147068628593,37.1517042005777,38.1077673560068));
#23372=CARTESIAN_POINT('Ctrl Pts',(-41.6213673298393,37.1611456014718,38.1179191384821));
#23373=CARTESIAN_POINT('Ctrl Pts',(-41.6280277968192,37.1705870023659,38.1280709209575));
#23374=CARTESIAN_POINT('Ctrl Pts',(-41.6346585169379,37.1800841429965,38.1381903807112));
#23375=CARTESIAN_POINT('Ctrl Pts',(-41.641259207857,37.1896366189718,38.1482770868531));
#23376=CARTESIAN_POINT('Ctrl Pts',(-41.647859898776,37.199189094947,38.1583637929951));
#23377=CARTESIAN_POINT('Ctrl Pts',(-41.6544305604938,37.2087969062648,38.1684177455228));
#23378=CARTESIAN_POINT('Ctrl Pts',(-41.6609709132292,37.218459643821,38.1784385163354));
#23379=CARTESIAN_POINT('Ctrl Pts',(-41.6675112659646,37.2281223813771,38.1884592871481));
#23380=CARTESIAN_POINT('Ctrl Pts',(-41.6740213097158,37.2378400451691,38.1984468762429));
#23381=CARTESIAN_POINT('Ctrl Pts',(-41.6805007672835,37.247612221416,38.2084008583455));
#23382=CARTESIAN_POINT('Ctrl Pts',(-41.323840382045,36.8039758164394,37.688053225496));
#23383=CARTESIAN_POINT('Ctrl Pts',(-41.3316406739716,36.8121870614232,37.6994899722748));
#23384=CARTESIAN_POINT('Ctrl Pts',(-41.3394129600866,36.8204647408363,37.7108980929574));
#23385=CARTESIAN_POINT('Ctrl Pts',(-41.347156880221,36.8288084705036,37.7222770585544));
#23386=CARTESIAN_POINT('Ctrl Pts',(-41.3548939241138,36.8371447913263,37.7336459201582));
#23387=CARTESIAN_POINT('Ctrl Pts',(-41.3626026523888,36.845547045163,37.7449856784364));
#23388=CARTESIAN_POINT('Ctrl Pts',(-41.3702827084734,36.8540148427975,37.7562958085134));
#23389=CARTESIAN_POINT('Ctrl Pts',(-41.377962764558,36.8624826404318,37.7676059385904));
#23390=CARTESIAN_POINT('Ctrl Pts',(-41.3856141484502,36.8710159818614,37.7788864404632));
#23391=CARTESIAN_POINT('Ctrl Pts',(-41.3932365062244,36.8796144718241,37.7901367919919));
#23392=CARTESIAN_POINT('Ctrl Pts',(-41.4008588639986,36.8882129617867,37.8013871435206));
#23393=CARTESIAN_POINT('Ctrl Pts',(-41.4084521956528,36.8968766002798,37.8126073447022));
#23394=CARTESIAN_POINT('Ctrl Pts',(-41.4160161499413,36.9056049860313,37.8237968761807));
#23395=CARTESIAN_POINT('Ctrl Pts',(-41.4235801042298,36.9143333717828,37.8349864076591));
#23396=CARTESIAN_POINT('Ctrl Pts',(-41.4311146811504,36.9231265047903,37.8461452694313));
#23397=CARTESIAN_POINT('Ctrl Pts',(-41.4386195321694,36.9319839778089,37.8572729449729));
#23398=CARTESIAN_POINT('Ctrl Pts',(-41.4461243831884,36.9408414508275,37.8684006205145));
#23399=CARTESIAN_POINT('Ctrl Pts',(-41.4535995083036,36.9497632638546,37.8794971098223));
#23400=CARTESIAN_POINT('Ctrl Pts',(-41.4610445617253,36.9587490037103,37.890561899251));
#23401=CARTESIAN_POINT('Ctrl Pts',(-41.4684896151469,36.967734743566,37.9016266886797));
#23402=CARTESIAN_POINT('Ctrl Pts',(-41.475904596873,36.9767844102475,37.9126597782262));
#23403=CARTESIAN_POINT('Ctrl Pts',(-41.4832891638893,36.9858975846777,37.9236606571714));
#23404=CARTESIAN_POINT('Ctrl Pts',(-41.4906737309056,36.9950107591077,37.9346615361166));
#23405=CARTESIAN_POINT('Ctrl Pts',(-41.4980278832102,37.0041874412838,37.9456302044575));
#23406=CARTESIAN_POINT('Ctrl Pts',(-41.5053512805964,37.0134272062696,37.9565661544483));
#23407=CARTESIAN_POINT('Ctrl Pts',(-41.5126746779825,37.0226669712554,37.9675021044391));
#23408=CARTESIAN_POINT('Ctrl Pts',(-41.5199673204481,37.0319698190485,37.9784053360766));
#23409=CARTESIAN_POINT('Ctrl Pts',(-41.527228870625,37.041335318893,37.9892753446353));
#23410=CARTESIAN_POINT('Ctrl Pts',(-41.534490420802,37.0507008187375,38.0001453531939));
#23411=CARTESIAN_POINT('Ctrl Pts',(-41.5417208786882,37.0601289706308,38.0109821386705));
#23412=CARTESIAN_POINT('Ctrl Pts',(-41.5489199097852,37.0696193380372,38.0217851994057));
#23413=CARTESIAN_POINT('Ctrl Pts',(-41.5561189408822,37.0791097054437,38.032588260141));
#23414=CARTESIAN_POINT('Ctrl Pts',(-41.5632865451879,37.0886622883605,38.0433575961318));
#23415=CARTESIAN_POINT('Ctrl Pts',(-41.5704223911043,37.0982766445122,38.0540927088314));
#23416=CARTESIAN_POINT('Ctrl Pts',(-41.5775582370206,37.1078910006639,38.064827821531));
#23417=CARTESIAN_POINT('Ctrl Pts',(-41.5846623245454,37.1175671300478,38.0755287109364));
#23418=CARTESIAN_POINT('Ctrl Pts',(-41.5917343250115,37.1273045846892,38.0861948816592));
#23419=CARTESIAN_POINT('Ctrl Pts',(-41.5988063254775,37.1370420393306,38.0968610523819));
#23420=CARTESIAN_POINT('Ctrl Pts',(-41.6058462388828,37.1468408192267,38.1074925044191));
#23421=CARTESIAN_POINT('Ctrl Pts',(-41.6128537395211,37.156700470745,38.1180887455863));
#23422=CARTESIAN_POINT('Ctrl Pts',(-41.6198612401594,37.1665601222634,38.1286849867535));
#23423=CARTESIAN_POINT('Ctrl Pts',(-41.6268363280286,37.1764806454011,38.1392460170477));
#23424=CARTESIAN_POINT('Ctrl Pts',(-41.6337786804136,37.1864615809095,38.1497713475339));
#23425=CARTESIAN_POINT('Ctrl Pts',(-41.6407210327985,37.1964425164179,38.16029667802));
#23426=CARTESIAN_POINT('Ctrl Pts',(-41.6476306496972,37.2064838642941,38.1707863086951));
#23427=CARTESIAN_POINT('Ctrl Pts',(-41.6545072114151,37.2165851597154,38.1812397539184));
#23428=CARTESIAN_POINT('Ctrl Pts',(-41.661383773133,37.2266864551368,38.1916931991416));
#23429=CARTESIAN_POINT('Ctrl Pts',(-41.6682272796678,37.2368476981002,38.2021104589099));
#23430=CARTESIAN_POINT('Ctrl Pts',(-41.6750374143759,37.2470684182525,38.2124910509217));
#23431=CARTESIAN_POINT('Ctrl Pts',(-41.300739486661,36.7866666524049,37.6701054954137));
#23432=CARTESIAN_POINT('Ctrl Pts',(-41.308946338799,36.7951351177238,37.6820419472366));
#23433=CARTESIAN_POINT('Ctrl Pts',(-41.3171230440224,36.8036760900231,37.6939476530182));
#23434=CARTESIAN_POINT('Ctrl Pts',(-41.325269190303,36.8122891381963,37.7058220124267));
#23435=CARTESIAN_POINT('Ctrl Pts',(-41.3334081031839,36.8208945383825,37.7176858279554));
#23436=CARTESIAN_POINT('Ctrl Pts',(-41.3415165113648,36.8295718864962,37.7295183527505));
#23437=CARTESIAN_POINT('Ctrl Pts',(-41.3495940069763,36.8383207453626,37.74131899122));
#23438=CARTESIAN_POINT('Ctrl Pts',(-41.3576715025878,36.847069604229,37.7531196296895));
#23439=CARTESIAN_POINT('Ctrl Pts',(-41.3657180856273,36.8558899738451,37.7648883818295));
#23440=CARTESIAN_POINT('Ctrl Pts',(-41.3737333513292,36.8647814098646,37.7766246552502));
#23441=CARTESIAN_POINT('Ctrl Pts',(-41.3817486170311,36.8736728458841,37.7883609286707));
#23442=CARTESIAN_POINT('Ctrl Pts',(-41.3897325653926,36.882635348304,37.800064723368));
#23443=CARTESIAN_POINT('Ctrl Pts',(-41.3976847947922,36.8916684656507,37.811735450213));
#23444=CARTESIAN_POINT('Ctrl Pts',(-41.4056370241918,36.9007015829975,37.823406177058));
#23445=CARTESIAN_POINT('Ctrl Pts',(-41.4135575346268,36.9098053152681,37.8350438360469));
#23446=CARTESIAN_POINT('Ctrl Pts',(-41.4214459276598,36.9189792039071,37.8466478413707));
#23447=CARTESIAN_POINT('Ctrl Pts',(-41.4293343206928,36.928153092546,37.8582518466945));
#23448=CARTESIAN_POINT('Ctrl Pts',(-41.4371905963211,36.9373971375502,37.8698221983494));
#23449=CARTESIAN_POINT('Ctrl Pts',(-41.4450143593312,36.9467108733282,37.8813583139049));
#23450=CARTESIAN_POINT('Ctrl Pts',(-41.4528381223413,36.9560246091062,37.8928944294605));
#23451=CARTESIAN_POINT('Ctrl Pts',(-41.4606293727305,36.9654080356548,37.9043963089128));
#23452=CARTESIAN_POINT('Ctrl Pts',(-41.4683877185487,36.9748606803929,37.9158633732683));
#23453=CARTESIAN_POINT('Ctrl Pts',(-41.476146064367,36.9843133251309,37.9273304376238));
#23454=CARTESIAN_POINT('Ctrl Pts',(-41.4838715055346,36.9938351879875,37.9387626868187));
#23455=CARTESIAN_POINT('Ctrl Pts',(-41.491563653561,37.0034257895769,37.9501595454759));
#23456=CARTESIAN_POINT('Ctrl Pts',(-41.4992558015874,37.0130163911663,37.9615564041331));
#23457=CARTESIAN_POINT('Ctrl Pts',(-41.5069146564582,37.0226757314765,37.9729178722397));
#23458=CARTESIAN_POINT('Ctrl Pts',(-41.5145398327278,37.0324033239651,37.9842433777404));
#23459=CARTESIAN_POINT('Ctrl Pts',(-41.5221650089974,37.0421309164538,37.9955688832409));
#23460=CARTESIAN_POINT('Ctrl Pts',(-41.5297565067344,37.0519267611811,38.006858426187));
#23461=CARTESIAN_POINT('Ctrl Pts',(-41.5373139440122,37.0617903648834,38.0181114382409));
#23462=CARTESIAN_POINT('Ctrl Pts',(-41.5448713812901,37.0716539685857,38.0293644502947));
#23463=CARTESIAN_POINT('Ctrl Pts',(-41.5523947581062,37.0815853312599,38.0405809314524));
#23464=CARTESIAN_POINT('Ctrl Pts',(-41.5598836959522,37.0915839528458,38.0517603170423));
#23465=CARTESIAN_POINT('Ctrl Pts',(-41.5673726337982,37.1015825744317,38.0629397026322));
#23466=CARTESIAN_POINT('Ctrl Pts',(-41.5748271326715,37.1116484549262,38.0740819926505));
#23467=CARTESIAN_POINT('Ctrl Pts',(-41.5822468175192,37.1217810875226,38.0851866261479));
#23468=CARTESIAN_POINT('Ctrl Pts',(-41.589666502367,37.1319137201192,38.0962912596452));
#23469=CARTESIAN_POINT('Ctrl Pts',(-41.5970513731868,37.1421131048144,38.107358236618));
#23470=CARTESIAN_POINT('Ctrl Pts',(-41.604401058419,37.1523787281061,38.1183869998953));
#23471=CARTESIAN_POINT('Ctrl Pts',(-41.6117507436512,37.1626443513978,38.1294157631727));
#23472=CARTESIAN_POINT('Ctrl Pts',(-41.6190652432934,37.1729762132827,38.1404063127509));
#23473=CARTESIAN_POINT('Ctrl Pts',(-41.6263441893162,37.1833737936141,38.1513580952935));
#23474=CARTESIAN_POINT('Ctrl Pts',(-41.6336231353391,37.1937713739454,38.1623098778361));
#23475=CARTESIAN_POINT('Ctrl Pts',(-41.6408665277401,37.2042346727198,38.1732228933392));
#23476=CARTESIAN_POINT('Ctrl Pts',(-41.6480740020571,37.2147631631981,38.184096592356));
#23477=CARTESIAN_POINT('Ctrl Pts',(-41.6552814763742,37.2252916536764,38.1949702913728));
#23478=CARTESIAN_POINT('Ctrl Pts',(-41.6624530326048,37.2358853358551,38.2058046738995));
#23479=CARTESIAN_POINT('Ctrl Pts',(-41.6695883098903,37.2465436764554,38.2165991944336));
#23480=CARTESIAN_POINT('Ctrl Pts',(-41.277913517507,36.7700593990031,37.6527056210249));
#23481=CARTESIAN_POINT('Ctrl Pts',(-41.2865220517812,36.7787672739902,37.665131206525));
#23482=CARTESIAN_POINT('Ctrl Pts',(-41.2950982902937,36.7875539692752,37.6775239293325));
#23483=CARTESIAN_POINT('Ctrl Pts',(-41.3036417632543,36.7964190035341,37.6898831105967));
#23484=CARTESIAN_POINT('Ctrl Pts',(-41.3121776500075,36.8052761660542,37.7022313174816));
#23485=CARTESIAN_POINT('Ctrl Pts',(-41.3206808293679,36.8142115284835,37.7145460423583));
#23486=CARTESIAN_POINT('Ctrl Pts',(-41.3291508363723,36.8232246022265,37.726826611844));
#23487=CARTESIAN_POINT('Ctrl Pts',(-41.3376208433767,36.8322376759696,37.7391071813297));
#23488=CARTESIAN_POINT('Ctrl Pts',(-41.3460576780217,36.8413284610227,37.7513535954195));
#23489=CARTESIAN_POINT('Ctrl Pts',(-41.3544608789718,36.8504964602918,37.7635651844659));
#23490=CARTESIAN_POINT('Ctrl Pts',(-41.3628640799219,36.8596644595609,37.7757767735122));
#23491=CARTESIAN_POINT('Ctrl Pts',(-41.3712336471738,36.8689096730424,37.7879535375104));
#23492=CARTESIAN_POINT('Ctrl Pts',(-41.3795691230703,36.8782315951976,37.8000948106213));
#23493=CARTESIAN_POINT('Ctrl Pts',(-41.3879045989668,36.8875535173528,37.8122360837323));
#23494=CARTESIAN_POINT('Ctrl Pts',(-41.3962059835046,36.8969521481781,37.8243418659513));
#23495=CARTESIAN_POINT('Ctrl Pts',(-41.4044728227548,36.906426973746,37.8364114953207));
#23496=CARTESIAN_POINT('Ctrl Pts',(-41.4127396620049,36.9159017993139,37.84848112469));
#23497=CARTESIAN_POINT('Ctrl Pts',(-41.4209719559642,36.9254528196206,37.8605146012051));
#23498=CARTESIAN_POINT('Ctrl Pts',(-41.4291692544817,36.9350795124057,37.8725112668619));
#23499=CARTESIAN_POINT('Ctrl Pts',(-41.4373665529991,36.9447062051908,37.8845079325187));
#23500=CARTESIAN_POINT('Ctrl Pts',(-41.4455288560714,36.9544085704505,37.8964677873126));
#23501=CARTESIAN_POINT('Ctrl Pts',(-41.4536557173749,36.9641860776488,37.9083901772654));
#23502=CARTESIAN_POINT('Ctrl Pts',(-41.4617825786783,36.973963584847,37.9203125672183));
#23503=CARTESIAN_POINT('Ctrl Pts',(-41.469873998137,36.9838162339168,37.9321974922695));
#23504=CARTESIAN_POINT('Ctrl Pts',(-41.4779295334512,36.9937434862326,37.9440443026519));
#23505=CARTESIAN_POINT('Ctrl Pts',(-41.4859850687655,37.0036707385483,37.9558911130344));
#23506=CARTESIAN_POINT('Ctrl Pts',(-41.494004719921,37.0136725940981,37.967699808735));
#23507=CARTESIAN_POINT('Ctrl Pts',(-41.5019880482629,37.0237485058532,37.9794697439402));
#23508=CARTESIAN_POINT('Ctrl Pts',(-41.5099713766048,37.0338244176084,37.9912396791453));
#23509=CARTESIAN_POINT('Ctrl Pts',(-41.5179183821971,37.0439743856239,38.0029708539018));
#23510=CARTESIAN_POINT('Ctrl Pts',(-41.5258286304887,37.0541978548883,38.0146626267361));
#23511=CARTESIAN_POINT('Ctrl Pts',(-41.5337388787803,37.0644213241527,38.0263543995704));
#23512=CARTESIAN_POINT('Ctrl Pts',(-41.5416123697679,37.0747182946621,38.0380067704779));
#23513=CARTESIAN_POINT('Ctrl Pts',(-41.5494486729206,37.0850882033665,38.0496191022939));
#23514=CARTESIAN_POINT('Ctrl Pts',(-41.5572849760732,37.0954581120709,38.06123143411));
#23515=CARTESIAN_POINT('Ctrl Pts',(-41.5650840913877,37.1059009589663,38.07280372683));
#23516=CARTESIAN_POINT('Ctrl Pts',(-41.5728455923997,37.1164161730263,38.0843353476683));
#23517=CARTESIAN_POINT('Ctrl Pts',(-41.5806070934118,37.1269313870862,38.0958669685066));
#23518=CARTESIAN_POINT('Ctrl Pts',(-41.5883309801183,37.1375189683066,38.1073579174584));
#23519=CARTESIAN_POINT('Ctrl Pts',(-41.5960168301686,37.1481783377467,38.1188075661862));
#23520=CARTESIAN_POINT('Ctrl Pts',(-41.6037026802189,37.1588377071868,38.1302572149139));
#23521=CARTESIAN_POINT('Ctrl Pts',(-41.61135049361,37.1695688648423,38.1416655634129));
#23522=CARTESIAN_POINT('Ctrl Pts',(-41.618959852151,37.1803712239218,38.1530319878621));
#23523=CARTESIAN_POINT('Ctrl Pts',(-41.6265692106919,37.1911735830013,38.1643984123112));
#23524=CARTESIAN_POINT('Ctrl Pts',(-41.6341401143796,37.2020471435004,38.1757229127059));
#23525=CARTESIAN_POINT('Ctrl Pts',(-41.6416721492288,37.2129913108407,38.1870048698101));
#23526=CARTESIAN_POINT('Ctrl Pts',(-41.649204184078,37.2239354781811,38.1982868269143));
#23527=CARTESIAN_POINT('Ctrl Pts',(-41.6566973500857,37.2349502523584,38.2095262407234));
#23528=CARTESIAN_POINT('Ctrl Pts',(-41.6641512375171,37.2460350310726,38.2207224966539));
#23529=CARTESIAN_POINT('Ctrl Pts',(-41.2322615791988,36.7368448921995,37.6179058722475));
#23530=CARTESIAN_POINT('Ctrl Pts',(-41.2416734777457,36.7460315865228,37.6313097251018));
#23531=CARTESIAN_POINT('Ctrl Pts',(-41.2510487828363,36.7553097277793,37.6446764819612));
#23532=CARTESIAN_POINT('Ctrl Pts',(-41.2603869091568,36.7646787342098,37.6580053069365));
#23533=CARTESIAN_POINT('Ctrl Pts',(-41.2697167436546,36.7740394213977,37.671322296534));
#23534=CARTESIAN_POINT('Ctrl Pts',(-41.2790094653743,36.7834908124581,37.6846014215741));
#23535=CARTESIAN_POINT('Ctrl Pts',(-41.2882644951643,36.7930323159545,37.6978418530921));
#23536=CARTESIAN_POINT('Ctrl Pts',(-41.2975195249545,36.8025738194508,37.7110822846101));
#23537=CARTESIAN_POINT('Ctrl Pts',(-41.3067368628103,36.812205435378,37.7242840225993));
#23538=CARTESIAN_POINT('Ctrl Pts',(-41.315915934257,36.8219265611464,37.7374462428973));
#23539=CARTESIAN_POINT('Ctrl Pts',(-41.3250950057036,36.8316476869147,37.7506084631952));
#23540=CARTESIAN_POINT('Ctrl Pts',(-41.3342358107362,36.8414583225193,37.7637311657951));
#23541=CARTESIAN_POINT('Ctrl Pts',(-41.3433377796266,36.8513578542914,37.776813531438));
#23542=CARTESIAN_POINT('Ctrl Pts',(-41.3524397485169,36.8612573860636,37.7898958970809));
#23543=CARTESIAN_POINT('Ctrl Pts',(-41.3615028812602,36.8712458139983,37.8029379257601));
#23544=CARTESIAN_POINT('Ctrl Pts',(-41.3705266129447,36.881322513424,37.8159388032206));
#23545=CARTESIAN_POINT('Ctrl Pts',(-41.3795503446293,36.8913992128497,37.8289396806812));
#23546=CARTESIAN_POINT('Ctrl Pts',(-41.3885346752505,36.9015641837612,37.8418994069165));
#23547=CARTESIAN_POINT('Ctrl Pts',(-41.3974790447827,36.9118167905605,37.8548171727759));
#23548=CARTESIAN_POINT('Ctrl Pts',(-41.4064234143148,36.9220693973599,37.8677349386352));
#23549=CARTESIAN_POINT('Ctrl Pts',(-41.4153278227533,36.9324096400418,37.8806107441121));
#23550=CARTESIAN_POINT('Ctrl Pts',(-41.4241917150271,36.9428368721605,37.8934437852596));
#23551=CARTESIAN_POINT('Ctrl Pts',(-41.433055607301,36.9532641042791,37.9062768264071));
#23552=CARTESIAN_POINT('Ctrl Pts',(-41.4418789833418,36.9637783257753,37.919067103171));
#23553=CARTESIAN_POINT('Ctrl Pts',(-41.4506612932317,36.9743788795439,37.931813817004));
#23554=CARTESIAN_POINT('Ctrl Pts',(-41.4594436031217,36.9849794333125,37.944560530837));
#23555=CARTESIAN_POINT('Ctrl Pts',(-41.4681848468466,36.9956663193414,37.9572636817256));
#23556=CARTESIAN_POINT('Ctrl Pts',(-41.4768844793332,37.0064388696294,37.9699224763397));
#23557=CARTESIAN_POINT('Ctrl Pts',(-41.4855841118197,37.0172114199174,37.9825812709539));
#23558=CARTESIAN_POINT('Ctrl Pts',(-41.4942421331226,37.0280696345095,37.9951957093312));
#23559=CARTESIAN_POINT('Ctrl Pts',(-41.5028580034416,37.0390128348981,38.0077650037266));
#23560=CARTESIAN_POINT('Ctrl Pts',(-41.5114738737606,37.0499560352868,38.0203342981219));
#23561=CARTESIAN_POINT('Ctrl Pts',(-41.5200475930913,37.0609842214665,38.0328584485288));
#23562=CARTESIAN_POINT('Ctrl Pts',(-41.5285786268573,37.0720967044079,38.0453366727972));
#23563=CARTESIAN_POINT('Ctrl Pts',(-41.5371096606233,37.0832091873492,38.0578148970656));
#23564=CARTESIAN_POINT('Ctrl Pts',(-41.5455980088201,37.0944059670466,38.0702471951892));
#23565=CARTESIAN_POINT('Ctrl Pts',(-41.5540431421607,37.1056863440336,38.0826327907092));
#23566=CARTESIAN_POINT('Ctrl Pts',(-41.5624882755012,37.1169667210205,38.0950183862292));
#23567=CARTESIAN_POINT('Ctrl Pts',(-41.5708901939812,37.1283306952912,38.1073572791394));
#23568=CARTESIAN_POINT('Ctrl Pts',(-41.5792483736678,37.1397775570278,38.1196486987679));
#23569=CARTESIAN_POINT('Ctrl Pts',(-41.5876065533543,37.1512244187646,38.1319401183963));
#23570=CARTESIAN_POINT('Ctrl Pts',(-41.5959209942432,37.1627541679616,38.1441840647368));
#23571=CARTESIAN_POINT('Ctrl Pts',(-41.6041911778204,37.1743660845373,38.1563797729991));
#23572=CARTESIAN_POINT('Ctrl Pts',(-41.6124613613976,37.185978001113,38.1685754812615));
#23573=CARTESIAN_POINT('Ctrl Pts',(-41.6206872876587,37.1976720850615,38.1807229514394));
#23574=CARTESIAN_POINT('Ctrl Pts',(-41.6288684435722,37.209447606126,38.1928214247184));
#23575=CARTESIAN_POINT('Ctrl Pts',(-41.6370495994857,37.2212231271905,38.2049198979974));
#23576=CARTESIAN_POINT('Ctrl Pts',(-41.6451859850473,37.233080085365,38.2169693743713));
#23577=CARTESIAN_POINT('Ctrl Pts',(-41.6532770927708,37.2450177403072,38.2289691010946));
#23578=CARTESIAN_POINT('Ctrl Pts',(-41.1877289817149,36.7064399824573,37.5853042020928));
#23579=CARTESIAN_POINT('Ctrl Pts',(-41.1979242219596,36.7160343690079,37.5996437919289));
#23580=CARTESIAN_POINT('Ctrl Pts',(-41.2080785460692,36.7257337815324,37.6139420716953));
#23581=CARTESIAN_POINT('Ctrl Pts',(-41.2181912296561,36.7355375248302,37.6281980198277));
#23582=CARTESIAN_POINT('Ctrl Pts',(-41.2282949336494,36.7453325628591,37.64244130934));
#23583=CARTESIAN_POINT('Ctrl Pts',(-41.2383570710302,36.755231746455,37.6566423423526));
#23584=CARTESIAN_POINT('Ctrl Pts',(-41.2483769252352,36.7652343675505,37.6708001060175));
#23585=CARTESIAN_POINT('Ctrl Pts',(-41.2583967794402,36.775236988646,37.6849578696824));
#23586=CARTESIAN_POINT('Ctrl Pts',(-41.2683743504628,36.7853430472343,37.6990723639902));
#23587=CARTESIAN_POINT('Ctrl Pts',(-41.2783089277365,36.7955518206302,37.7131425822324));
#23588=CARTESIAN_POINT('Ctrl Pts',(-41.2882435050103,36.8057605940261,37.7272128004746));
#23589=CARTESIAN_POINT('Ctrl Pts',(-41.2981350885286,36.8160720822226,37.7412387426419));
#23590=CARTESIAN_POINT('Ctrl Pts',(-41.307982973821,36.8264855480185,37.755219408306));
#23591=CARTESIAN_POINT('Ctrl Pts',(-41.3178308591135,36.8368990138144,37.7692000739701));
#23592=CARTESIAN_POINT('Ctrl Pts',(-41.3276350461735,36.8474144572026,37.7831354631218));
#23593=CARTESIAN_POINT('Ctrl Pts',(-41.3373948367249,36.8580311265692,37.7970245817532));
#23594=CARTESIAN_POINT('Ctrl Pts',(-41.3471546272764,36.8686477959358,37.8109137003846));
#23595=CARTESIAN_POINT('Ctrl Pts',(-41.3568700213129,36.8793656912737,37.8247565484865));
#23596=CARTESIAN_POINT('Ctrl Pts',(-41.3665403268503,36.8901840466619,37.8385521386106));
#23597=CARTESIAN_POINT('Ctrl Pts',(-41.3762106323877,36.90100240205,37.8523477287347));
#23598=CARTESIAN_POINT('Ctrl Pts',(-41.3858358494196,36.9119212174812,37.8660960608719));
#23599=CARTESIAN_POINT('Ctrl Pts',(-41.3954152923506,36.9229397128349,37.8797961542715));
#23600=CARTESIAN_POINT('Ctrl Pts',(-41.4049947352816,36.9339582081886,37.8934962476712));
#23601=CARTESIAN_POINT('Ctrl Pts',(-41.4145284041053,36.9450763834573,37.9071481023244));
#23602=CARTESIAN_POINT('Ctrl Pts',(-41.4240156197108,36.9562934444306,37.9207507443156));
#23603=CARTESIAN_POINT('Ctrl Pts',(-41.4335028353163,36.9675105054037,37.9343533863069));
#23604=CARTESIAN_POINT('Ctrl Pts',(-41.4429435976973,36.9788264520739,37.9479068156272));
#23605=CARTESIAN_POINT('Ctrl Pts',(-41.4523372343223,36.9902404762517,37.9614100653328));
#23606=CARTESIAN_POINT('Ctrl Pts',(-41.4617308709474,37.0016545004295,37.9749133150385));
#23607=CARTESIAN_POINT('Ctrl Pts',(-41.4710773818102,37.0131666021072,37.9883663851205));
#23608=CARTESIAN_POINT('Ctrl Pts',(-41.4803761010527,37.0247759592303,38.001768315742));
#23609=CARTESIAN_POINT('Ctrl Pts',(-41.4896748202951,37.0363853163534,38.0151702463634));
#23610=CARTESIAN_POINT('Ctrl Pts',(-41.4989257479112,37.048091928914,38.0285210375155));
#23611=CARTESIAN_POINT('Ctrl Pts',(-41.5081282248091,37.0598949611075,38.0418197366027));
#23612=CARTESIAN_POINT('Ctrl Pts',(-41.517330701707,37.071697993301,38.0551184356899));
#23613=CARTESIAN_POINT('Ctrl Pts',(-41.5264847278807,37.0835974451195,38.0683650427034));
#23614=CARTESIAN_POINT('Ctrl Pts',(-41.5355896510973,37.0955924671253,38.0815586124227));
#23615=CARTESIAN_POINT('Ctrl Pts',(-41.5446945743139,37.107587489131,38.0947521821419));
#23616=CARTESIAN_POINT('Ctrl Pts',(-41.5537503945673,37.1196780813162,38.107892714558));
#23617=CARTESIAN_POINT('Ctrl Pts',(-41.5627564665744,37.1318633807292,38.1209792719577));
#23618=CARTESIAN_POINT('Ctrl Pts',(-41.5717625385814,37.1440486801423,38.1340658293574));
#23619=CARTESIAN_POINT('Ctrl Pts',(-41.5807188623362,37.156328686775,38.147098411732));
#23620=CARTESIAN_POINT('Ctrl Pts',(-41.5896247995955,37.1687025242832,38.1600760890065));
#23621=CARTESIAN_POINT('Ctrl Pts',(-41.5985307368549,37.1810763617914,38.1730537662811));
#23622=CARTESIAN_POINT('Ctrl Pts',(-41.6073862876129,37.1935440301667,38.1859765384471));
#23623=CARTESIAN_POINT('Ctrl Pts',(-41.6161908207558,37.2061046397946,38.1988434831987));
#23624=CARTESIAN_POINT('Ctrl Pts',(-41.6249953538988,37.2186652494225,38.2117104279504));
#23625=CARTESIAN_POINT('Ctrl Pts',(-41.6337488694209,37.2313188002946,38.2245215452789));
#23626=CARTESIAN_POINT('Ctrl Pts',(-41.6424507434257,37.244064389651,38.2372759207768));
#23627=CARTESIAN_POINT('Ctrl Pts',(-41.1444195426625,36.6783597806106,37.5546020043376));
#23628=CARTESIAN_POINT('Ctrl Pts',(-41.1553734557036,36.6883054348728,37.5698384308781));
#23629=CARTESIAN_POINT('Ctrl Pts',(-41.166282235733,36.6983703147992,37.5850294796951));
#23630=CARTESIAN_POINT('Ctrl Pts',(-41.1771449970972,36.708553603238,37.6001739174679));
#23631=CARTESIAN_POINT('Ctrl Pts',(-41.1879981128335,36.7187278493895,37.615304907683));
#23632=CARTESIAN_POINT('Ctrl Pts',(-41.1988052915835,36.7290202938554,37.6303893695809));
#23633=CARTESIAN_POINT('Ctrl Pts',(-41.2095656574962,36.7394301025007,37.6454260806647));
#23634=CARTESIAN_POINT('Ctrl Pts',(-41.220326023409,36.749839911146,37.6604627917486));
#23635=CARTESIAN_POINT('Ctrl Pts',(-41.2310395764751,36.7603670839615,37.6754517520053));
#23636=CARTESIAN_POINT('Ctrl Pts',(-41.2417054484313,36.771010767789,37.690391746678));
#23637=CARTESIAN_POINT('Ctrl Pts',(-41.2523713203876,36.7816544516165,37.7053317413507));
#23638=CARTESIAN_POINT('Ctrl Pts',(-41.2629895112246,36.7924146464467,37.7202227704263));
#23639=CARTESIAN_POINT('Ctrl Pts',(-41.2735591604079,36.8032904802363,37.7350636270846));
#23640=CARTESIAN_POINT('Ctrl Pts',(-41.2841288095911,36.8141663140259,37.7499044837429));
#23641=CARTESIAN_POINT('Ctrl Pts',(-41.2946499171111,36.8251577867655,37.7646951679709));
#23642=CARTESIAN_POINT('Ctrl Pts',(-41.3051216303013,36.8362640076682,37.7794344810807));
#23643=CARTESIAN_POINT('Ctrl Pts',(-41.3155933434915,36.8473702285709,37.7941737941905));
#23644=CARTESIAN_POINT('Ctrl Pts',(-41.3260156623427,36.8585911976271,37.8088617361692));
#23645=CARTESIAN_POINT('Ctrl Pts',(-41.3363877421943,36.8699260054509,37.8234971166555));
#23646=CARTESIAN_POINT('Ctrl Pts',(-41.3467598220459,36.8812608132747,37.8381324971418));
#23647=CARTESIAN_POINT('Ctrl Pts',(-41.3570816628888,36.892709459856,37.8527153161229));
#23648=CARTESIAN_POINT('Ctrl Pts',(-41.3673524282056,36.9042710173573,37.8672443917569));
#23649=CARTESIAN_POINT('Ctrl Pts',(-41.3776231935224,36.9158325748587,37.8817734673908));
#23650=CARTESIAN_POINT('Ctrl Pts',(-41.387842883304,36.9275070432698,37.8962487996651));
#23651=CARTESIAN_POINT('Ctrl Pts',(-41.3980106693117,36.9392934764517,37.9106692154489));
#23652=CARTESIAN_POINT('Ctrl Pts',(-41.4081784553195,36.9510799096335,37.9250896312327));
#23653=CARTESIAN_POINT('Ctrl Pts',(-41.4182943375443,36.9629783075759,37.9394551305134));
#23654=CARTESIAN_POINT('Ctrl Pts',(-41.4283574961605,36.9749877059916,37.9537645490616));
#23655=CARTESIAN_POINT('Ctrl Pts',(-41.4384206547766,36.9869971044073,37.9680739676097));
#23656=CARTESIAN_POINT('Ctrl Pts',(-41.4484310897753,36.9991175032858,37.9823273054128));
#23657=CARTESIAN_POINT('Ctrl Pts',(-41.4583879898763,37.0113479203483,37.9965234073313));
#23658=CARTESIAN_POINT('Ctrl Pts',(-41.4683448899773,37.0235783374109,38.0107195092498));
#23659=CARTESIAN_POINT('Ctrl Pts',(-41.478248255172,37.0359187726468,38.0248583752714));
#23660=CARTESIAN_POINT('Ctrl Pts',(-41.4880972828577,37.0483682259447,38.0389388595335));
#23661=CARTESIAN_POINT('Ctrl Pts',(-41.4979463105433,37.0608176792426,38.0530193437957));
#23662=CARTESIAN_POINT('Ctrl Pts',(-41.5077410007112,37.0733761505917,38.0670414462863));
#23663=CARTESIAN_POINT('Ctrl Pts',(-41.5174805595661,37.0860426222101,38.0810040306058));
#23664=CARTESIAN_POINT('Ctrl Pts',(-41.5272201184209,37.0987090938285,38.0949666149253));
#23665=CARTESIAN_POINT('Ctrl Pts',(-41.5369045459541,37.1114835657054,38.1088696810615));
#23666=CARTESIAN_POINT('Ctrl Pts',(-41.5465330573064,37.1243650025534,38.1227121022621));
#23667=CARTESIAN_POINT('Ctrl Pts',(-41.5561615686588,37.1372464394014,38.1365545234628));
#23668=CARTESIAN_POINT('Ctrl Pts',(-41.5657341638218,37.1502348412093,38.1503362997158));
#23669=CARTESIAN_POINT('Ctrl Pts',(-41.5752500669993,37.1633291553525,38.1640563140985));
#23670=CARTESIAN_POINT('Ctrl Pts',(-41.584765970177,37.1764234694955,38.1777763284813));
#23671=CARTESIAN_POINT('Ctrl Pts',(-41.5942251813608,37.1896236959624,38.1914345809818));
#23672=CARTESIAN_POINT('Ctrl Pts',(-41.603626933944,37.2029287649612,38.2050299646883));
#23673=CARTESIAN_POINT('Ctrl Pts',(-41.6130286865272,37.21623383396,38.2186253483948));
#23674=CARTESIAN_POINT('Ctrl Pts',(-41.6223729805015,37.2296437454791,38.2321578632955));
#23675=CARTESIAN_POINT('Ctrl Pts',(-41.6316590585731,37.2431574127333,38.2456264126687));
#23676=CARTESIAN_POINT('Ctrl Pts',(-41.1011101036101,36.6502795787638,37.5238998065825));
#23677=CARTESIAN_POINT('Ctrl Pts',(-41.1128226894475,36.6605765007378,37.5400330698273));
#23678=CARTESIAN_POINT('Ctrl Pts',(-41.1244859253969,36.6710068480659,37.5561168876949));
#23679=CARTESIAN_POINT('Ctrl Pts',(-41.1360987645382,36.6815696816458,37.5721498151081));
#23680=CARTESIAN_POINT('Ctrl Pts',(-41.1477012920175,36.6921231359199,37.588168506026));
#23681=CARTESIAN_POINT('Ctrl Pts',(-41.1592535121368,36.7028088412558,37.6041363968091));
#23682=CARTESIAN_POINT('Ctrl Pts',(-41.1707543897573,36.7136258374508,37.620052055312));
#23683=CARTESIAN_POINT('Ctrl Pts',(-41.1822552673778,36.7244428336459,37.6359677138148));
#23684=CARTESIAN_POINT('Ctrl Pts',(-41.1937048024874,36.7353911206887,37.6518311400204));
#23685=CARTESIAN_POINT('Ctrl Pts',(-41.2051019691261,36.7464697149479,37.6676409111236));
#23686=CARTESIAN_POINT('Ctrl Pts',(-41.2164991357649,36.757548309207,37.6834506822268));
#23687=CARTESIAN_POINT('Ctrl Pts',(-41.2278439339207,36.7687572106707,37.6992067982107));
#23688=CARTESIAN_POINT('Ctrl Pts',(-41.2391353469947,36.7800954124541,37.7149078458632));
#23689=CARTESIAN_POINT('Ctrl Pts',(-41.2504267600686,36.7914336142374,37.7306088935157));
#23690=CARTESIAN_POINT('Ctrl Pts',(-41.2616647880488,36.8029011163283,37.74625487282));
#23691=CARTESIAN_POINT('Ctrl Pts',(-41.2728484238777,36.8144968887672,37.7618443804082));
#23692=CARTESIAN_POINT('Ctrl Pts',(-41.2840320597066,36.8260926612061,37.7774338879964));
#23693=CARTESIAN_POINT('Ctrl Pts',(-41.2951613033725,36.8378167039806,37.792966923852));
#23694=CARTESIAN_POINT('Ctrl Pts',(-41.3062351575383,36.8496679642399,37.8084420947004));
#23695=CARTESIAN_POINT('Ctrl Pts',(-41.3173090117041,36.8615192244992,37.8239172655489));
#23696=CARTESIAN_POINT('Ctrl Pts',(-41.328327476358,36.8734977022308,37.8393345713738));
#23697=CARTESIAN_POINT('Ctrl Pts',(-41.3392895640606,36.8856023218798,37.8546926292421));
#23698=CARTESIAN_POINT('Ctrl Pts',(-41.3502516517632,36.8977069415287,37.8700506871105));
#23699=CARTESIAN_POINT('Ctrl Pts',(-41.3611573625028,36.9099377030822,37.8853494970058));
#23700=CARTESIAN_POINT('Ctrl Pts',(-41.3720057189127,36.9222935084728,37.9005876865821));
#23701=CARTESIAN_POINT('Ctrl Pts',(-41.3828540753226,36.9346493138634,37.9158258761585));
#23702=CARTESIAN_POINT('Ctrl Pts',(-41.3936450773913,36.9471301630778,37.9310034453995));
#23703=CARTESIAN_POINT('Ctrl Pts',(-41.4043777579986,36.9597349357315,37.9461190327902));
#23704=CARTESIAN_POINT('Ctrl Pts',(-41.4151104386059,36.9723397083851,37.9612346201809));
#23705=CARTESIAN_POINT('Ctrl Pts',(-41.4257847977404,36.9850684044644,37.9762882257051));
#23706=CARTESIAN_POINT('Ctrl Pts',(-41.4363998786999,36.9979198814664,37.9912784989207));
#23707=CARTESIAN_POINT('Ctrl Pts',(-41.4470149596595,37.0107713584684,38.0062687721363));
#23708=CARTESIAN_POINT('Ctrl Pts',(-41.4575707624329,37.0237456163795,38.0211957130272));
#23709=CARTESIAN_POINT('Ctrl Pts',(-41.4680663409063,37.0368414907819,38.0360579824644));
#23710=CARTESIAN_POINT('Ctrl Pts',(-41.4785619193796,37.0499373651843,38.0509202519016));
#23711=CARTESIAN_POINT('Ctrl Pts',(-41.4889972735417,37.0631548560639,38.0657178498691));
#23712=CARTESIAN_POINT('Ctrl Pts',(-41.4993714680348,37.0764927772949,38.0804494487889));
#23713=CARTESIAN_POINT('Ctrl Pts',(-41.5097456625279,37.0898306985261,38.0951810477086));
#23714=CARTESIAN_POINT('Ctrl Pts',(-41.520058697341,37.1032890500945,38.109846647565));
#23715=CARTESIAN_POINT('Ctrl Pts',(-41.5303096480385,37.1168666243775,38.1244449325666));
#23716=CARTESIAN_POINT('Ctrl Pts',(-41.5405605987361,37.1304441986604,38.1390432175682));
#23717=CARTESIAN_POINT('Ctrl Pts',(-41.5507494653073,37.1441409956436,38.1535741876996));
#23718=CARTESIAN_POINT('Ctrl Pts',(-41.5608753344032,37.1579557864216,38.1680365391905));
#23719=CARTESIAN_POINT('Ctrl Pts',(-41.571001203499,37.1717705771997,38.1824988906814));
#23720=CARTESIAN_POINT('Ctrl Pts',(-41.5810640751088,37.1857033617581,38.1968926235164));
#23721=CARTESIAN_POINT('Ctrl Pts',(-41.5910630471322,37.1997528901279,38.2112164461778));
#23722=CARTESIAN_POINT('Ctrl Pts',(-41.6010620191556,37.2138024184976,38.2255402688393));
#23723=CARTESIAN_POINT('Ctrl Pts',(-41.6109970915822,37.2279686906637,38.2397941813121));
#23724=CARTESIAN_POINT('Ctrl Pts',(-41.6208673737205,37.2422504358157,38.2539769045607));
#23725=CARTESIAN_POINT('Ctrl Pts',(-41.0590044066045,36.6245107757466,37.4950828317286));
#23726=CARTESIAN_POINT('Ctrl Pts',(-41.0714514561137,36.6351027502924,37.5120743871615));
#23727=CARTESIAN_POINT('Ctrl Pts',(-41.0838450412698,36.6458429750105,37.529012572385));
#23728=CARTESIAN_POINT('Ctrl Pts',(-41.0961839313899,36.6567303801302,37.5458957042908));
#23729=CARTESIAN_POINT('Ctrl Pts',(-41.1085118651484,36.6676081177397,37.5627638447592));
#23730=CARTESIAN_POINT('Ctrl Pts',(-41.1207852011292,36.6786327745861,37.5795770297387));
#23731=CARTESIAN_POINT('Ctrl Pts',(-41.13300272309,36.6898032549803,37.5963335917226));
#23732=CARTESIAN_POINT('Ctrl Pts',(-41.1452202450508,36.7009737353744,37.6130901537065));
#23733=CARTESIAN_POINT('Ctrl Pts',(-41.1573819529757,36.7122900393016,37.6297900926729));
#23734=CARTESIAN_POINT('Ctrl Pts',(-41.1694866416616,36.7237510422997,37.6464317523176));
#23735=CARTESIAN_POINT('Ctrl Pts',(-41.1815913303475,36.7352120452978,37.6630734119624));
#23736=CARTESIAN_POINT('Ctrl Pts',(-41.1936389997787,36.7468177473517,37.6796567922638));
#23737=CARTESIAN_POINT('Ctrl Pts',(-41.2056284560277,36.7585669954476,37.6961802484455));
#23738=CARTESIAN_POINT('Ctrl Pts',(-41.2176179122767,36.7703162435434,37.7127037046271));
#23739=CARTESIAN_POINT('Ctrl Pts',(-41.2295491553279,36.7822090376658,37.7291672366675));
#23740=CARTESIAN_POINT('Ctrl Pts',(-41.2414210027637,36.7942441964755,37.7455692116409));
#23741=CARTESIAN_POINT('Ctrl Pts',(-41.2532928501995,36.8062793552852,37.7619711866143));
#23742=CARTESIAN_POINT('Ctrl Pts',(-41.2651053020044,36.8184568787666,37.7783116044994));
#23743=CARTESIAN_POINT('Ctrl Pts',(-41.2768571875023,36.830775557488,37.7945888445415));
#23744=CARTESIAN_POINT('Ctrl Pts',(-41.2886090730003,36.8430942362094,37.8108660845837));
#23745=CARTESIAN_POINT('Ctrl Pts',(-41.300300392176,36.8555540701548,37.8270801467617));
#23746=CARTESIAN_POINT('Ctrl Pts',(-41.3119299863247,36.8681538220374,37.8432294228106));
#23747=CARTESIAN_POINT('Ctrl Pts',(-41.3235595804735,36.8807535739201,37.8593786988595));
#23748=CARTESIAN_POINT('Ctrl Pts',(-41.3351274494821,36.8934932436479,37.8754631886912));
#23749=CARTESIAN_POINT('Ctrl Pts',(-41.3466324470441,36.9063715664765,37.8914812969822));
#23750=CARTESIAN_POINT('Ctrl Pts',(-41.3581374446061,36.9192498893049,37.9074994052732));
#23751=CARTESIAN_POINT('Ctrl Pts',(-41.3695795706916,36.9322668652086,37.9234511319931));
#23752=CARTESIAN_POINT('Ctrl Pts',(-41.3809576910404,36.9454212017859,37.9393348946783));
#23753=CARTESIAN_POINT('Ctrl Pts',(-41.3923358113892,36.9585755383631,37.9552186573635));
#23754=CARTESIAN_POINT('Ctrl Pts',(-41.4036499260769,36.9718672356681,37.9710344560556));
#23755=CARTESIAN_POINT('Ctrl Pts',(-41.4148989136667,36.9852949743307,37.9867807218423));
#23756=CARTESIAN_POINT('Ctrl Pts',(-41.4261479012565,36.9987227129934,38.0025269876289));
#23757=CARTESIAN_POINT('Ctrl Pts',(-41.4373317617337,37.0122864929962,38.0182037204896));
#23758=CARTESIAN_POINT('Ctrl Pts',(-41.4484493865271,37.0259849681195,38.0338093652491));
#23759=CARTESIAN_POINT('Ctrl Pts',(-41.4595670113204,37.0396834432429,38.0494150100086));
#23760=CARTESIAN_POINT('Ctrl Pts',(-41.4706184004156,37.0535166134687,38.0649495666467));
#23761=CARTESIAN_POINT('Ctrl Pts',(-41.4816024583245,37.0674831059924,38.0804114940307));
#23762=CARTESIAN_POINT('Ctrl Pts',(-41.4925865162334,37.081449598516,38.0958734214147));
#23763=CARTESIAN_POINT('Ctrl Pts',(-41.503503242942,37.0955494133191,38.1112627195244));
#23764=CARTESIAN_POINT('Ctrl Pts',(-41.5143515562604,37.1097811512812,38.1265778615725));
#23765=CARTESIAN_POINT('Ctrl Pts',(-41.5251998695787,37.1240128892433,38.1418930036207));
#23766=CARTESIAN_POINT('Ctrl Pts',(-41.5359797694928,37.1383765503461,38.1571339895872));
#23767=CARTESIAN_POINT('Ctrl Pts',(-41.5466901873235,37.1528707094282,38.1722993073297));
#23768=CARTESIAN_POINT('Ctrl Pts',(-41.5574006051541,37.1673648685103,38.1874646250722));
#23769=CARTESIAN_POINT('Ctrl Pts',(-41.5680415408875,37.181989525553,38.2025542745711));
#23770=CARTESIAN_POINT('Ctrl Pts',(-41.5786119395645,37.1967432296344,38.2175667586257));
#23771=CARTESIAN_POINT('Ctrl Pts',(-41.5891823382414,37.2114969337158,38.2325792426804));
#23772=CARTESIAN_POINT('Ctrl Pts',(-41.5996821998361,37.2263796848018,38.2475145612583));
#23773=CARTESIAN_POINT('Ctrl Pts',(-41.6101104833444,37.2413900065276,38.2623712324232));
#23774=CARTESIAN_POINT('Ctrl Pts',(-41.0179887248003,36.6005789209292,37.4678003654629));
#23775=CARTESIAN_POINT('Ctrl Pts',(-41.0311471669881,36.6114222484506,37.485617698704));
#23776=CARTESIAN_POINT('Ctrl Pts',(-41.0442481894302,36.6224290791273,37.503377932541));
#23777=CARTESIAN_POINT('Ctrl Pts',(-41.0572903576435,36.6335982078395,37.5210791225655));
#23778=CARTESIAN_POINT('Ctrl Pts',(-41.0703209450169,36.6447574188839,37.538764594755));
#23779=CARTESIAN_POINT('Ctrl Pts',(-41.0832927827835,36.656078639948,37.5563911280262));
#23780=CARTESIAN_POINT('Ctrl Pts',(-41.096204453453,36.6675606339116,37.5739567962497));
#23781=CARTESIAN_POINT('Ctrl Pts',(-41.1091161241225,36.6790426278752,37.5915224644731));
#23782=CARTESIAN_POINT('Ctrl Pts',(-41.1219676276744,36.6906853947201,37.6090272676208));
#23783=CARTESIAN_POINT('Ctrl Pts',(-41.1347575597677,36.7024876621894,37.6264692928652));
#23784=CARTESIAN_POINT('Ctrl Pts',(-41.147547491861,36.7142899296587,37.6439113181096));
#23785=CARTESIAN_POINT('Ctrl Pts',(-41.1602758524755,36.7262516977336,37.6612905654229));
#23786=CARTESIAN_POINT('Ctrl Pts',(-41.1729412507266,36.7383716592988,37.6786051356975));
#23787=CARTESIAN_POINT('Ctrl Pts',(-41.1856066489777,36.7504916208638,37.6959197059722));
#23788=CARTESIAN_POINT('Ctrl Pts',(-41.1982090848453,36.7627697758997,37.7131695991807));
#23789=CARTESIAN_POINT('Ctrl Pts',(-41.2107471812052,36.775204782718,37.7303529303506));
#23790=CARTESIAN_POINT('Ctrl Pts',(-41.2232852775651,36.7876397895362,37.7475362615205));
#23791=CARTESIAN_POINT('Ctrl Pts',(-41.2357590343974,36.800231648117,37.7646530306244));
#23792=CARTESIAN_POINT('Ctrl Pts',(-41.2481670886393,36.8129789824919,37.781701367237));
#23793=CARTESIAN_POINT('Ctrl Pts',(-41.2605751428813,36.8257263168669,37.7987497038497));
#23794=CARTESIAN_POINT('Ctrl Pts',(-41.272917494513,36.8386291270158,37.8157296079438));
#23795=CARTESIAN_POINT('Ctrl Pts',(-41.285192794831,36.8516860029913,37.8326392240499));
#23796=CARTESIAN_POINT('Ctrl Pts',(-41.2974680951491,36.8647428789668,37.8495488401561));
#23797=CARTESIAN_POINT('Ctrl Pts',(-41.3096763440434,36.8779538206795,37.8663881681866));
#23798=CARTESIAN_POINT('Ctrl Pts',(-41.3218162076488,36.8913173846502,37.883155368157));
#23799=CARTESIAN_POINT('Ctrl Pts',(-41.3339560712541,36.9046809486209,37.8999225681274));
#23800=CARTESIAN_POINT('Ctrl Pts',(-41.3460275495374,36.9181971348206,37.9166176400022));
#23801=CARTESIAN_POINT('Ctrl Pts',(-41.358029323231,36.9318644661482,37.9332387593263));
#23802=CARTESIAN_POINT('Ctrl Pts',(-41.3700310969245,36.9455317974758,37.9498598786504));
#23803=CARTESIAN_POINT('Ctrl Pts',(-41.3819631660927,36.9593502739742,37.9664070454536));
#23804=CARTESIAN_POINT('Ctrl Pts',(-41.3938242268655,36.9733183856371,37.9828784515537));
#23805=CARTESIAN_POINT('Ctrl Pts',(-41.4056852876383,36.9872864973001,37.9993498576536));
#23806=CARTESIAN_POINT('Ctrl Pts',(-41.4174753399967,37.0014042441052,38.0157455030242));
#23807=CARTESIAN_POINT('Ctrl Pts',(-41.4291930955894,37.0156700833438,38.0320635960404));
#23808=CARTESIAN_POINT('Ctrl Pts',(-41.440910851182,37.0299359225824,38.0483816890565));
#23809=CARTESIAN_POINT('Ctrl Pts',(-41.4525563099903,37.0443498542317,38.0646222296922));
#23810=CARTESIAN_POINT('Ctrl Pts',(-41.4641281994632,37.0589103032173,38.0807834432716));
#23811=CARTESIAN_POINT('Ctrl Pts',(-41.4757000889362,37.073470752203,38.096944656851));
#23812=CARTESIAN_POINT('Ctrl Pts',(-41.4871984090552,37.0881777185019,38.1130265433482));
#23813=CARTESIAN_POINT('Ctrl Pts',(-41.498621903348,37.1030295950185,38.1290273454241));
#23814=CARTESIAN_POINT('Ctrl Pts',(-41.5100453976408,37.117881471535,38.1450281475001));
#23815=CARTESIAN_POINT('Ctrl Pts',(-41.5213940660891,37.1328782582455,38.1609478651294));
#23816=CARTESIAN_POINT('Ctrl Pts',(-41.5326666685735,37.1480183163847,38.1767847586936));
#23817=CARTESIAN_POINT('Ctrl Pts',(-41.5439392710579,37.1631583745239,38.1926216522579));
#23818=CARTESIAN_POINT('Ctrl Pts',(-41.5551358075605,37.1784417040676,38.2083757217319));
#23819=CARTESIAN_POINT('Ctrl Pts',(-41.566255054586,37.1938666349384,38.2240452455987));
#23820=CARTESIAN_POINT('Ctrl Pts',(-41.5773743016115,37.2092915658092,38.2397147694655));
#23821=CARTESIAN_POINT('Ctrl Pts',(-41.5884162591307,37.2248580979685,38.2552997476876));
#23822=CARTESIAN_POINT('Ctrl Pts',(-41.5993797205659,37.2405645304232,38.2707984772518));
#23823=CARTESIAN_POINT('Ctrl Pts',(-40.9769730429962,36.5766470661117,37.4405178991973));
#23824=CARTESIAN_POINT('Ctrl Pts',(-40.9908428778625,36.5877417466088,37.4591610102465));
#23825=CARTESIAN_POINT('Ctrl Pts',(-41.0046513375907,36.5990151832441,37.4777432926971));
#23826=CARTESIAN_POINT('Ctrl Pts',(-41.0183967838972,36.6104660355487,37.4962625408402));
#23827=CARTESIAN_POINT('Ctrl Pts',(-41.0321300248855,36.6219067200281,37.5147653447508));
#23828=CARTESIAN_POINT('Ctrl Pts',(-41.0458003644378,36.6335245053098,37.5332052263138));
#23829=CARTESIAN_POINT('Ctrl Pts',(-41.0594061838161,36.645318012843,37.5515800007768));
#23830=CARTESIAN_POINT('Ctrl Pts',(-41.0730120031943,36.6571115203761,37.5699547752398));
#23831=CARTESIAN_POINT('Ctrl Pts',(-41.0865533023731,36.6690807501385,37.5882644425688));
#23832=CARTESIAN_POINT('Ctrl Pts',(-41.1000284778738,36.6812242820791,37.6065068334128));
#23833=CARTESIAN_POINT('Ctrl Pts',(-41.1135036533746,36.6933678140196,37.6247492242568));
#23834=CARTESIAN_POINT('Ctrl Pts',(-41.1269127051723,36.7056856481155,37.6429243385819));
#23835=CARTESIAN_POINT('Ctrl Pts',(-41.1402540454255,36.7181763231499,37.6610300229497));
#23836=CARTESIAN_POINT('Ctrl Pts',(-41.1535953856787,36.7306669981843,37.6791357073173));
#23837=CARTESIAN_POINT('Ctrl Pts',(-41.1668690143625,36.7433305141338,37.6971719616938));
#23838=CARTESIAN_POINT('Ctrl Pts',(-41.1800733596466,36.7561653689606,37.7151366490602));
#23839=CARTESIAN_POINT('Ctrl Pts',(-41.1932777049307,36.7690002237873,37.7331013364267));
#23840=CARTESIAN_POINT('Ctrl Pts',(-41.2064127667905,36.7820064174673,37.7509944567495));
#23841=CARTESIAN_POINT('Ctrl Pts',(-41.2194769897764,36.7951824074959,37.7688138899326));
#23842=CARTESIAN_POINT('Ctrl Pts',(-41.2325412127622,36.8083583975245,37.7866333231157));
#23843=CARTESIAN_POINT('Ctrl Pts',(-41.24553459685,36.821704183877,37.8043790691258));
#23844=CARTESIAN_POINT('Ctrl Pts',(-41.2584556033373,36.8352181839453,37.8220490252892));
#23845=CARTESIAN_POINT('Ctrl Pts',(-41.2713766098246,36.8487321840136,37.8397189814527));
#23846=CARTESIAN_POINT('Ctrl Pts',(-41.2842252386047,36.8624143977111,37.857313147682));
#23847=CARTESIAN_POINT('Ctrl Pts',(-41.2969999682534,36.8762632028239,37.8748294393318));
#23848=CARTESIAN_POINT('Ctrl Pts',(-41.3097746979022,36.8901120079368,37.8923457309815));
#23849=CARTESIAN_POINT('Ctrl Pts',(-41.3224755283832,36.9041274044326,37.9097841480114));
#23850=CARTESIAN_POINT('Ctrl Pts',(-41.3351009554215,36.9183077305106,37.9271426239743));
#23851=CARTESIAN_POINT('Ctrl Pts',(-41.3477263824598,36.9324880565886,37.9445010999372));
#23852=CARTESIAN_POINT('Ctrl Pts',(-41.3602764061085,36.9468333122803,37.9617796348516));
#23853=CARTESIAN_POINT('Ctrl Pts',(-41.3727495400643,36.9613417969435,37.978976181265));
#23854=CARTESIAN_POINT('Ctrl Pts',(-41.3852226740201,36.9758502816067,37.9961727276784));
#23855=CARTESIAN_POINT('Ctrl Pts',(-41.3976189182597,36.9905219952142,38.0132872855588));
#23856=CARTESIAN_POINT('Ctrl Pts',(-41.4099368046517,37.0053551985681,38.0303178268316));
#23857=CARTESIAN_POINT('Ctrl Pts',(-41.4222546910436,37.0201884019219,38.0473483681044));
#23858=CARTESIAN_POINT('Ctrl Pts',(-41.4344942195651,37.0351830949946,38.0642948927377));
#23859=CARTESIAN_POINT('Ctrl Pts',(-41.4466539406019,37.0503375004424,38.0811553925125));
#23860=CARTESIAN_POINT('Ctrl Pts',(-41.4588136616388,37.0654919058901,38.0980158922873));
#23861=CARTESIAN_POINT('Ctrl Pts',(-41.4708935751684,37.0808060236847,38.1147903671719));
#23862=CARTESIAN_POINT('Ctrl Pts',(-41.4828922504357,37.0962780387556,38.1314768292758));
#23863=CARTESIAN_POINT('Ctrl Pts',(-41.4948909257029,37.1117500538266,38.1481632913796));
#23864=CARTESIAN_POINT('Ctrl Pts',(-41.5068083626853,37.1273799661451,38.1647617406715));
#23865=CARTESIAN_POINT('Ctrl Pts',(-41.5186431498235,37.1431659233413,38.1812702100575));
#23866=CARTESIAN_POINT('Ctrl Pts',(-41.5304779369617,37.1589518805375,38.1977786794435));
#23867=CARTESIAN_POINT('Ctrl Pts',(-41.5422300742335,37.1748938825821,38.2141971688928));
#23868=CARTESIAN_POINT('Ctrl Pts',(-41.5538981696076,37.1909900402423,38.2305237325717));
#23869=CARTESIAN_POINT('Ctrl Pts',(-41.5655662649816,37.2070861979025,38.2468502962505));
#23870=CARTESIAN_POINT('Ctrl Pts',(-41.5771503184253,37.2233365111352,38.2630849341168));
#23871=CARTESIAN_POINT('Ctrl Pts',(-41.5886489577874,37.2397390543188,38.2792257220803));
#23872=CARTESIAN_POINT('Ctrl Pts',(-40.9370413012329,36.5545511456659,37.4147676065073));
#23873=CARTESIAN_POINT('Ctrl Pts',(-40.9515996140237,36.5658534553905,37.434204060764));
#23874=CARTESIAN_POINT('Ctrl Pts',(-40.9660927536195,36.5773502054972,37.4535761511003));
#23875=CARTESIAN_POINT('Ctrl Pts',(-40.9805188577964,36.5890399153777,37.4728813871476));
#23876=CARTESIAN_POINT('Ctrl Pts',(-40.9949321522625,36.6007192453386,37.4921694810415));
#23877=CARTESIAN_POINT('Ctrl Pts',(-41.0092785302739,36.612591192521,37.5113908392785));
#23878=CARTESIAN_POINT('Ctrl Pts',(-41.0235561517129,36.6246542309846,37.530542995226));
#23879=CARTESIAN_POINT('Ctrl Pts',(-41.0378337731518,36.6367172694482,37.5496951511735));
#23880=CARTESIAN_POINT('Ctrl Pts',(-41.0520426379871,36.6489713991667,37.5687781047898));
#23881=CARTESIAN_POINT('Ctrl Pts',(-41.0661809237201,36.6614150453174,37.5877894071794));
#23882=CARTESIAN_POINT('Ctrl Pts',(-41.080319209453,36.6738586914682,37.6068007095689));
#23883=CARTESIAN_POINT('Ctrl Pts',(-41.094386916053,36.6864918540241,37.6257403606905));
#23884=CARTESIAN_POINT('Ctrl Pts',(-41.1083822391043,36.6993129096823,37.6446059300101));
#23885=CARTESIAN_POINT('Ctrl Pts',(-41.1223775621556,36.7121339653404,37.6634714993296));
#23886=CARTESIAN_POINT('Ctrl Pts',(-41.1363005016279,36.7251429140727,37.6822629868061));
#23887=CARTESIAN_POINT('Ctrl Pts',(-41.1501492716497,36.7383380845113,37.7009779808874));
#23888=CARTESIAN_POINT('Ctrl Pts',(-41.1639980416715,36.7515332549499,37.7196929749687));
#23889=CARTESIAN_POINT('Ctrl Pts',(-41.1777726422125,36.7649146470659,37.7383314756139));
#23890=CARTESIAN_POINT('Ctrl Pts',(-41.1914713063994,36.7784805418522,37.7568910908672));
#23891=CARTESIAN_POINT('Ctrl Pts',(-41.2051699705863,36.7920464366385,37.7754507061205));
#23892=CARTESIAN_POINT('Ctrl Pts',(-41.2187926983892,36.8057968340656,37.7939314359414));
#23893=CARTESIAN_POINT('Ctrl Pts',(-41.2323377423839,36.8197299679269,37.8123309085804));
#23894=CARTESIAN_POINT('Ctrl Pts',(-41.2458827863786,36.8336631017881,37.8307303812194));
#23895=CARTESIAN_POINT('Ctrl Pts',(-41.2593501465357,36.847778972053,37.8490485966365));
#23896=CARTESIAN_POINT('Ctrl Pts',(-41.2727380953247,36.8620757657659,37.8672832038934));
#23897=CARTESIAN_POINT('Ctrl Pts',(-41.2861260441138,36.8763725594786,37.8855178111503));
#23898=CARTESIAN_POINT('Ctrl Pts',(-41.2994345815056,36.8908502766081,37.9036688102071));
#23899=CARTESIAN_POINT('Ctrl Pts',(-41.312662000305,36.9055070579126,37.9217338715366));
#23900=CARTESIAN_POINT('Ctrl Pts',(-41.3258894191044,36.9201638392171,37.9397989328662));
#23901=CARTESIAN_POINT('Ctrl Pts',(-41.3390357192823,36.9349996846645,37.957778056429));
#23902=CARTESIAN_POINT('Ctrl Pts',(-41.3520992144129,36.9500126892013,37.9756689347026));
#23903=CARTESIAN_POINT('Ctrl Pts',(-41.3651627095435,36.965025693738,37.9935598129762));
#23904=CARTESIAN_POINT('Ctrl Pts',(-41.3781433995983,36.9802158573313,38.0113624459216));
#23905=CARTESIAN_POINT('Ctrl Pts',(-41.3910396193511,36.995581229602,38.0290745486096));
#23906=CARTESIAN_POINT('Ctrl Pts',(-41.4039358391038,37.0109466018728,38.0467866512976));
#23907=CARTESIAN_POINT('Ctrl Pts',(-41.4167475885263,37.0264871827876,38.0644082236895));
#23908=CARTESIAN_POINT('Ctrl Pts',(-41.4294732240162,37.0422009771393,38.0819370040326));
#23909=CARTESIAN_POINT('Ctrl Pts',(-41.4421988595062,37.0579147714911,38.0994657843757));
#23910=CARTESIAN_POINT('Ctrl Pts',(-41.4548383810359,37.0738017792454,38.1169017726317));
#23911=CARTESIAN_POINT('Ctrl Pts',(-41.4673901670459,37.0898599608768,38.1342427308005));
#23912=CARTESIAN_POINT('Ctrl Pts',(-41.479941953056,37.105918142508,38.1515836889694));
#23913=CARTESIAN_POINT('Ctrl Pts',(-41.492406003519,37.1221474979812,38.1688296170134));
#23914=CARTESIAN_POINT('Ctrl Pts',(-41.504780719332,37.1385459439719,38.1859783012565));
#23915=CARTESIAN_POINT('Ctrl Pts',(-41.517155435145,37.1549443899626,38.2031269854997));
#23916=CARTESIAN_POINT('Ctrl Pts',(-41.529440816281,37.171511926435,38.2201784259045));
#23917=CARTESIAN_POINT('Ctrl Pts',(-41.541635286501,37.1882464267978,38.2371304336835));
#23918=CARTESIAN_POINT('Ctrl Pts',(-41.553829756721,37.2049809271606,38.2540824414625));
#23919=CARTESIAN_POINT('Ctrl Pts',(-41.5659333159984,37.2218823913772,38.2709350165786));
#23920=CARTESIAN_POINT('Ctrl Pts',(-41.57794441136,37.2389486501317,38.2876859956913));
#23921=CARTESIAN_POINT('Ctrl Pts',(-40.898041328523,36.5339186748625,37.3902570496062));
#23922=CARTESIAN_POINT('Ctrl Pts',(-40.9132677638581,36.5453941770888,37.4104598746157));
#23923=CARTESIAN_POINT('Ctrl Pts',(-40.9284254085022,36.5570801166835,37.4305950141167));
#23924=CARTESIAN_POINT('Ctrl Pts',(-40.9435121571034,36.5689748704718,37.4506596713947));
#23925=CARTESIAN_POINT('Ctrl Pts',(-40.9585855093722,36.5808590622711,37.4707065121886));
#23926=CARTESIAN_POINT('Ctrl Pts',(-40.9735880914081,36.5929516975633,37.4906829958224));
#23927=CARTESIAN_POINT('Ctrl Pts',(-40.988517823087,36.6052510996916,37.5105863525352));
#23928=CARTESIAN_POINT('Ctrl Pts',(-41.0034475547659,36.61755050182,37.530489709248));
#23929=CARTESIAN_POINT('Ctrl Pts',(-41.0183044360495,36.630056670753,37.5503199389887));
#23930=CARTESIAN_POINT('Ctrl Pts',(-41.0330864070153,36.6427678724969,37.5700742922747));
#23931=CARTESIAN_POINT('Ctrl Pts',(-41.0478683779811,36.6554790742407,37.5898286455607));
#23932=CARTESIAN_POINT('Ctrl Pts',(-41.0625754385914,36.6683953087629,37.6095071223416));
#23933=CARTESIAN_POINT('Ctrl Pts',(-41.0772055496959,36.6815147852136,37.6291069941749));
#23934=CARTESIAN_POINT('Ctrl Pts',(-41.0918356608005,36.6946342616642,37.6487068660083));
#23935=CARTESIAN_POINT('Ctrl Pts',(-41.1063888223619,36.7079569800095,37.668228132844));
#23936=CARTESIAN_POINT('Ctrl Pts',(-41.120863016569,36.7214810930406,37.6876680880377));
#23937=CARTESIAN_POINT('Ctrl Pts',(-41.1353372107762,36.7350052060716,37.7071080432314));
#23938=CARTESIAN_POINT('Ctrl Pts',(-41.1497324375917,36.7487307137537,37.7264666867331));
#23939=CARTESIAN_POINT('Ctrl Pts',(-41.164046701102,36.7626557130303,37.7457413344461));
#23940=CARTESIAN_POINT('Ctrl Pts',(-41.1783609646123,36.7765807123069,37.7650159821591));
#23941=CARTESIAN_POINT('Ctrl Pts',(-41.1925942647807,36.7907052031424,37.7842066340339));
#23942=CARTESIAN_POINT('Ctrl Pts',(-41.2067446281447,36.805027227161,37.8033106292661));
#23943=CARTESIAN_POINT('Ctrl Pts',(-41.2208949915087,36.8193492511795,37.8224146244984));
#23944=CARTESIAN_POINT('Ctrl Pts',(-41.2349624180324,36.8338688083445,37.8414319630391));
#23945=CARTESIAN_POINT('Ctrl Pts',(-41.2489449572515,36.8485838855035,37.8603600081137));
#23946=CARTESIAN_POINT('Ctrl Pts',(-41.2629274964706,36.8632989626625,37.8792880531883));
#23947=CARTESIAN_POINT('Ctrl Pts',(-41.2768251483493,36.8782095597778,37.8981268047483));
#23948=CARTESIAN_POINT('Ctrl Pts',(-41.2906359859636,36.8933136094794,37.9168736507806));
#23949=CARTESIAN_POINT('Ctrl Pts',(-41.3044468235779,36.9084176591809,37.935620496813));
#23950=CARTESIAN_POINT('Ctrl Pts',(-41.3181708468922,36.9237151614297,37.9542754372696));
#23951=CARTESIAN_POINT('Ctrl Pts',(-41.3318061530559,36.939203995211,37.9728358856229));
#23952=CARTESIAN_POINT('Ctrl Pts',(-41.3454414592196,36.9546928289921,37.9913963339763));
#23953=CARTESIAN_POINT('Ctrl Pts',(-41.3589880481978,36.9703729942658,38.0098622901787));
#23954=CARTESIAN_POINT('Ctrl Pts',(-41.3724440417414,36.9862423169603,38.0282311939057));
#23955=CARTESIAN_POINT('Ctrl Pts',(-41.385900035285,37.0021116396548,38.0466000976326));
#23956=CARTESIAN_POINT('Ctrl Pts',(-41.3992654333594,37.0181701197294,38.0648719488369));
#23957=CARTESIAN_POINT('Ctrl Pts',(-41.4125383828378,37.0344155306586,38.0830442141068));
#23958=CARTESIAN_POINT('Ctrl Pts',(-41.4258113323163,37.0506609415878,38.1012164793766));
#23959=CARTESIAN_POINT('Ctrl Pts',(-41.4389918331648,37.0670932833299,38.1192891586655));
#23960=CARTESIAN_POINT('Ctrl Pts',(-41.4520780578928,37.0837102775231,38.137259746177));
#23961=CARTESIAN_POINT('Ctrl Pts',(-41.4651642826207,37.1003272717164,38.1552303336884));
#23962=CARTESIAN_POINT('Ctrl Pts',(-41.4781562311946,37.1171289183182,38.1730988293764));
#23963=CARTESIAN_POINT('Ctrl Pts',(-41.4910521022666,37.1341128877621,38.1908627557548));
#23964=CARTESIAN_POINT('Ctrl Pts',(-41.5039479733387,37.151096857206,38.2086266821332));
#23965=CARTESIAN_POINT('Ctrl Pts',(-41.516747766876,37.1682631494485,38.2262860391564));
#23966=CARTESIAN_POINT('Ctrl Pts',(-41.5294497081733,37.1856093843648,38.2438383783356));
#23967=CARTESIAN_POINT('Ctrl Pts',(-41.5421516494707,37.2029556192811,38.2613907175148));
#23968=CARTESIAN_POINT('Ctrl Pts',(-41.5547557384956,37.2204817968266,38.2788360388052));
#23969=CARTESIAN_POINT('Ctrl Pts',(-41.5672602276774,37.2381854869781,38.2961719233939));
#23970=CARTESIAN_POINT('Ctrl Pts',(-40.8590413558131,36.513286204059,37.3657464927051));
#23971=CARTESIAN_POINT('Ctrl Pts',(-40.8749359136926,36.5249348987871,37.3867156884675));
#23972=CARTESIAN_POINT('Ctrl Pts',(-40.8907580633849,36.5368100278699,37.407613877133));
#23973=CARTESIAN_POINT('Ctrl Pts',(-40.9065054564103,36.548909825566,37.4284379556418));
#23974=CARTESIAN_POINT('Ctrl Pts',(-40.9222388664818,36.5609988792036,37.4492435433357));
#23975=CARTESIAN_POINT('Ctrl Pts',(-40.9378976525422,36.5733122026056,37.4699751523663));
#23976=CARTESIAN_POINT('Ctrl Pts',(-40.9534794944611,36.5858479683988,37.4906297098443));
#23977=CARTESIAN_POINT('Ctrl Pts',(-40.9690613363799,36.5983837341919,37.5112842673223));
#23978=CARTESIAN_POINT('Ctrl Pts',(-40.9845662341119,36.6111419423394,37.5318617731876));
#23979=CARTESIAN_POINT('Ctrl Pts',(-40.9999918903106,36.6241206996763,37.5523591773701));
#23980=CARTESIAN_POINT('Ctrl Pts',(-41.0154175465092,36.6370994570133,37.5728565815525));
#23981=CARTESIAN_POINT('Ctrl Pts',(-41.0307639611298,36.6502987635018,37.5932738839926));
#23982=CARTESIAN_POINT('Ctrl Pts',(-41.0460288602876,36.6637166607449,37.6136080583398));
#23983=CARTESIAN_POINT('Ctrl Pts',(-41.0612937594454,36.677134557988,37.6339422326869));
#23984=CARTESIAN_POINT('Ctrl Pts',(-41.076477143096,36.6907710459463,37.654193278882));
#23985=CARTESIAN_POINT('Ctrl Pts',(-41.0915767614884,36.7046241015698,37.674358195188));
#23986=CARTESIAN_POINT('Ctrl Pts',(-41.1066763798808,36.7184771571934,37.6945231114941));
#23987=CARTESIAN_POINT('Ctrl Pts',(-41.121692232971,36.7325467804415,37.7146018978523));
#23988=CARTESIAN_POINT('Ctrl Pts',(-41.1366220958047,36.7468308842084,37.734591578025));
#23989=CARTESIAN_POINT('Ctrl Pts',(-41.1515519586384,36.7611149879753,37.7545812581977));
#23990=CARTESIAN_POINT('Ctrl Pts',(-41.1663958311721,36.7756135722191,37.7744818321265));
#23991=CARTESIAN_POINT('Ctrl Pts',(-41.1811515139055,36.7903244863951,37.7942903499519));
#23992=CARTESIAN_POINT('Ctrl Pts',(-41.1959071966389,36.8050354005709,37.8140988677773));
#23993=CARTESIAN_POINT('Ctrl Pts',(-41.210574689529,36.8199586446359,37.8338153294417));
#23994=CARTESIAN_POINT('Ctrl Pts',(-41.2251518191782,36.8350920052412,37.853436812334));
#23995=CARTESIAN_POINT('Ctrl Pts',(-41.2397289488273,36.8502253658463,37.8730582952263));
#23996=CARTESIAN_POINT('Ctrl Pts',(-41.254215715193,36.8655688429475,37.8925847992895));
#23997=CARTESIAN_POINT('Ctrl Pts',(-41.2686099716222,36.8811201610461,37.9120134300246));
#23998=CARTESIAN_POINT('Ctrl Pts',(-41.2830042280514,36.8966714791447,37.9314420607598));
#23999=CARTESIAN_POINT('Ctrl Pts',(-41.2973059745021,36.912430638195,37.9507728181102));
#24000=CARTESIAN_POINT('Ctrl Pts',(-41.3115130916989,36.9283953012207,37.9700028365432));
#24001=CARTESIAN_POINT('Ctrl Pts',(-41.3257202088957,36.9443599642462,37.9892328549763));
#24002=CARTESIAN_POINT('Ctrl Pts',(-41.3398326967973,36.9605301312003,38.0083621344359));
#24003=CARTESIAN_POINT('Ctrl Pts',(-41.3538484641317,36.9769034043186,38.0273878392017));
#24004=CARTESIAN_POINT('Ctrl Pts',(-41.3678642314661,36.9932766774368,38.0464135439676));
#24005=CARTESIAN_POINT('Ctrl Pts',(-41.3817832781924,37.0098530566712,38.0653356739843));
#24006=CARTESIAN_POINT('Ctrl Pts',(-41.3956035416594,37.0266300841779,38.0841514241809));
#24007=CARTESIAN_POINT('Ctrl Pts',(-41.4094238051265,37.0434071116845,38.1029671743776));
#24008=CARTESIAN_POINT('Ctrl Pts',(-41.4231452852938,37.0603847874144,38.1216765446994));
#24009=CARTESIAN_POINT('Ctrl Pts',(-41.4367659487396,37.0775605941696,38.1402767615534));
#24010=CARTESIAN_POINT('Ctrl Pts',(-41.4503866121855,37.0947364009248,38.1588769784074));
#24011=CARTESIAN_POINT('Ctrl Pts',(-41.4639064588701,37.1121103386552,38.1773680417394));
#24012=CARTESIAN_POINT('Ctrl Pts',(-41.4773234852013,37.1296798315523,38.195747210253));
#24013=CARTESIAN_POINT('Ctrl Pts',(-41.4907405115324,37.1472493244494,38.2141263787666));
#24014=CARTESIAN_POINT('Ctrl Pts',(-41.504054717471,37.165014372462,38.2323936524082));
#24015=CARTESIAN_POINT('Ctrl Pts',(-41.5172641298457,37.1829723419318,38.2505463229878));
#24016=CARTESIAN_POINT('Ctrl Pts',(-41.5304735422203,37.2009303114016,38.2686989935672));
#24017=CARTESIAN_POINT('Ctrl Pts',(-41.5435781609927,37.2190812022761,38.2867370610317));
#24018=CARTESIAN_POINT('Ctrl Pts',(-41.5565760439949,37.2374223238246,38.3046578510965));
#24019=CARTESIAN_POINT('Ctrl Pts',(-40.8209716822033,36.4941186642374,37.3424762704269));
#24020=CARTESIAN_POINT('Ctrl Pts',(-40.8375140519548,36.5059060599091,37.3641848666864));
#24021=CARTESIAN_POINT('Ctrl Pts',(-40.8539805753213,36.5179362010818,37.3858193469145));
#24022=CARTESIAN_POINT('Ctrl Pts',(-40.8703686424312,36.5302071774958,37.4073762805876));
#24023=CARTESIAN_POINT('Ctrl Pts',(-40.8867421576984,36.5424672578523,37.4289140727044));
#24024=CARTESIAN_POINT('Ctrl Pts',(-40.9030373558039,36.5549677458436,37.4503744557762));
#24025=CARTESIAN_POINT('Ctrl Pts',(-40.9192516575975,36.5677066598323,37.4717540322971));
#24026=CARTESIAN_POINT('Ctrl Pts',(-40.9354659593912,36.5804455738209,37.4931336088181));
#24027=CARTESIAN_POINT('Ctrl Pts',(-40.9515993648368,36.593422913768,37.5144323787275));
#24028=CARTESIAN_POINT('Ctrl Pts',(-40.9676493211198,36.6066366231236,37.5356469705377));
#24029=CARTESIAN_POINT('Ctrl Pts',(-40.9836992774029,36.6198503324791,37.5568615623479));
#24030=CARTESIAN_POINT('Ctrl Pts',(-40.9996657844525,36.6333004111949,37.5779919759778));
#24031=CARTESIAN_POINT('Ctrl Pts',(-41.0155463151547,36.6469847276582,37.5990348661468));
#24032=CARTESIAN_POINT('Ctrl Pts',(-41.031426845857,36.6606690441215,37.6200777563158));
#24033=CARTESIAN_POINT('Ctrl Pts',(-41.0472214001766,36.6745875982916,37.6410331229643));
#24034=CARTESIAN_POINT('Ctrl Pts',(-41.0629274788306,36.6887381849399,37.6618976488843));
#24035=CARTESIAN_POINT('Ctrl Pts',(-41.0786335574846,36.7028887715881,37.6827621748045));
#24036=CARTESIAN_POINT('Ctrl Pts',(-41.0942511602649,36.7172713905735,37.7035358598319));
#24037=CARTESIAN_POINT('Ctrl Pts',(-41.1097778155592,36.7318837631807,37.7242154153001));
#24038=CARTESIAN_POINT('Ctrl Pts',(-41.1253044708535,36.7464961357878,37.7448949707684));
#24039=CARTESIAN_POINT('Ctrl Pts',(-41.1407401786102,36.761338261968,37.7654803966087));
#24040=CARTESIAN_POINT('Ctrl Pts',(-41.1560824959735,36.7764077904247,37.7859684339199));
#24041=CARTESIAN_POINT('Ctrl Pts',(-41.1714248133369,36.7914773188815,37.8064564712311));
#24042=CARTESIAN_POINT('Ctrl Pts',(-41.186673740424,36.806774249681,37.8268471200493));
#24043=CARTESIAN_POINT('Ctrl Pts',(-41.2018268635633,36.8222961594514,37.8471371520539));
#24044=CARTESIAN_POINT('Ctrl Pts',(-41.2169799867026,36.8378180692218,37.8674271840586));
#24045=CARTESIAN_POINT('Ctrl Pts',(-41.2320373058687,36.8535649579224,37.8876165991963));
#24046=CARTESIAN_POINT('Ctrl Pts',(-41.2469964383245,36.8695343315615,37.9077022013597));
#24047=CARTESIAN_POINT('Ctrl Pts',(-41.2619555707802,36.8855037052005,37.9277878035232));
#24048=CARTESIAN_POINT('Ctrl Pts',(-41.2768165163203,36.9016955636138,37.9477695925484));
#24049=CARTESIAN_POINT('Ctrl Pts',(-41.2915769229406,36.918107342302,37.9676444049552));
#24050=CARTESIAN_POINT('Ctrl Pts',(-41.3063373295609,36.9345191209902,37.9875192173619));
#24051=CARTESIAN_POINT('Ctrl Pts',(-41.3209971972124,36.9511508198986,38.0072870530841));
#24052=CARTESIAN_POINT('Ctrl Pts',(-41.3355542056702,36.9679998050485,38.0269447824567));
#24053=CARTESIAN_POINT('Ctrl Pts',(-41.3501112141281,36.9848487901984,38.0466025118293));
#24054=CARTESIAN_POINT('Ctrl Pts',(-41.3645653633439,37.0019150615336,38.0661501347871));
#24055=CARTESIAN_POINT('Ctrl Pts',(-41.3789143656034,37.0191959164268,38.0855845564669));
#24056=CARTESIAN_POINT('Ctrl Pts',(-41.3932633678628,37.0364767713199,38.1050189781468));
#24057=CARTESIAN_POINT('Ctrl Pts',(-41.4075072231182,37.0539722097134,38.1243401984841));
#24058=CARTESIAN_POINT('Ctrl Pts',(-41.4216436768867,37.0716794611833,38.1435451583937));
#24059=CARTESIAN_POINT('Ctrl Pts',(-41.4357801306552,37.0893867126534,38.1627501183033));
#24060=CARTESIAN_POINT('Ctrl Pts',(-41.4498091828898,37.1073057771408,38.1818388177213));
#24061=CARTESIAN_POINT('Ctrl Pts',(-41.4637286130497,37.1254338172992,38.2008082343046));
#24062=CARTESIAN_POINT('Ctrl Pts',(-41.4776480432095,37.1435618574576,38.2197776508878));
#24063=CARTESIAN_POINT('Ctrl Pts',(-41.4914578512484,37.1618988732265,38.2386277845733));
#24064=CARTESIAN_POINT('Ctrl Pts',(-41.5051558512673,37.1804419612312,38.2573556507129));
#24065=CARTESIAN_POINT('Ctrl Pts',(-41.5188538512862,37.1989850492358,38.2760835168526));
#24066=CARTESIAN_POINT('Ctrl Pts',(-41.5324400432657,37.2177342094461,38.2946891154127));
#24067=CARTESIAN_POINT('Ctrl Pts',(-41.5459122765801,37.2366864733069,38.3131695003217));
#24068=CARTESIAN_POINT('Ctrl Pts',(-40.783693232143,36.4761376056301,37.3202208879071));
#24069=CARTESIAN_POINT('Ctrl Pts',(-40.8008656922496,36.4880359432873,37.3426462956984));
#24070=CARTESIAN_POINT('Ctrl Pts',(-40.817959055311,36.5001935767271,37.3649946966318));
#24071=CARTESIAN_POINT('Ctrl Pts',(-40.834970431829,36.5126084506244,37.3872623124709));
#24072=CARTESIAN_POINT('Ctrl Pts',(-40.8519667030344,36.5250123006901,37.4095101557009));
#24073=CARTESIAN_POINT('Ctrl Pts',(-40.8688811330549,36.5376729344845,37.4316773570879));
#24074=CARTESIAN_POINT('Ctrl Pts',(-40.8857108667677,36.5505882150004,37.4537601751103));
#24075=CARTESIAN_POINT('Ctrl Pts',(-40.9025406004804,36.5635034955164,37.4758429931327));
#24076=CARTESIAN_POINT('Ctrl Pts',(-40.9192856378381,36.5766734227079,37.4978414277164));
#24077=CARTESIAN_POINT('Ctrl Pts',(-40.9359431530081,36.5900957739832,37.5197517662424));
#24078=CARTESIAN_POINT('Ctrl Pts',(-40.9526006681781,36.6035181252586,37.5416621047685));
#24079=CARTESIAN_POINT('Ctrl Pts',(-40.9691706610809,36.6171929005631,37.5634843471441));
#24080=CARTESIAN_POINT('Ctrl Pts',(-40.9856503347759,36.6311177917365,37.5852148100976));
#24081=CARTESIAN_POINT('Ctrl Pts',(-41.0021300084708,36.6450426829098,37.6069452730511));
#24082=CARTESIAN_POINT('Ctrl Pts',(-41.0185193629119,36.6592176899033,37.6285839565095));
#24083=CARTESIAN_POINT('Ctrl Pts',(-41.0348156322482,36.6736404204794,37.6501272085428));
#24084=CARTESIAN_POINT('Ctrl Pts',(-41.0511119015846,36.6880631510554,37.6716704605762));
#24085=CARTESIAN_POINT('Ctrl Pts',(-41.0673150856079,36.7027336050728,37.6931182810147));
#24086=CARTESIAN_POINT('Ctrl Pts',(-41.0834224495998,36.717649306502,37.7144670499681));
#24087=CARTESIAN_POINT('Ctrl Pts',(-41.0995298135917,36.7325650079314,37.7358158189215));
#24088=CARTESIAN_POINT('Ctrl Pts',(-41.1155413574911,36.7477259567159,37.7570655363088));
#24089=CARTESIAN_POINT('Ctrl Pts',(-41.1314543789239,36.7631295940424,37.7782126156749));
#24090=CARTESIAN_POINT('Ctrl Pts',(-41.1473674003568,36.7785332313689,37.799359695041));
#24091=CARTESIAN_POINT('Ctrl Pts',(-41.1631818994208,36.7941795572869,37.8204041364024));
#24092=CARTESIAN_POINT('Ctrl Pts',(-41.1788952066766,36.8100659308439,37.841342387753));
#24093=CARTESIAN_POINT('Ctrl Pts',(-41.1946085139324,36.8259523044009,37.8622806391035));
#24094=CARTESIAN_POINT('Ctrl Pts',(-41.2102206293435,36.8420787255466,37.8831127003765));
#24095=CARTESIAN_POINT('Ctrl Pts',(-41.2257289182373,36.8584424727222,37.9038350557851));
#24096=CARTESIAN_POINT('Ctrl Pts',(-41.2412372071311,36.8748062198979,37.9245574111936));
#24097=CARTESIAN_POINT('Ctrl Pts',(-41.2566416693023,36.8914072929382,37.9451700605687));
#24098=CARTESIAN_POINT('Ctrl Pts',(-41.2719397048379,36.9082428899705,37.9656695249773));
#24099=CARTESIAN_POINT('Ctrl Pts',(-41.2872377403735,36.9250784870027,37.9861689893859));
#24100=CARTESIAN_POINT('Ctrl Pts',(-41.3024293492156,36.942148607963,38.0065552687502));
#24101=CARTESIAN_POINT('Ctrl Pts',(-41.3175119673761,36.9594503718142,38.0268249223433));
#24102=CARTESIAN_POINT('Ctrl Pts',(-41.3325945855365,36.9767521356655,38.0470945759364));
#24103=CARTESIAN_POINT('Ctrl Pts',(-41.347568212958,36.9942855423421,38.0672476036812));
#24104=CARTESIAN_POINT('Ctrl Pts',(-41.3624303224426,37.0120476326152,38.0872806042184));
#24105=CARTESIAN_POINT('Ctrl Pts',(-41.3772924319271,37.0298097228883,38.1073136047554));
#24106=CARTESIAN_POINT('Ctrl Pts',(-41.3920430234184,37.0478004966904,38.1272265780087));
#24107=CARTESIAN_POINT('Ctrl Pts',(-41.4066796073615,37.0660169176001,38.1470161631342));
#24108=CARTESIAN_POINT('Ctrl Pts',(-41.4213161913047,37.0842333385096,38.1668057482597));
#24109=CARTESIAN_POINT('Ctrl Pts',(-41.4358387676443,37.1026754064574,38.1864719451823));
#24110=CARTESIAN_POINT('Ctrl Pts',(-41.4502448853092,37.1213400088539,38.2060114347081));
#24111=CARTESIAN_POINT('Ctrl Pts',(-41.4646510029741,37.1400046112504,38.2255509242339));
#24112=CARTESIAN_POINT('Ctrl Pts',(-41.4789406619095,37.1588917480246,38.2449637062886));
#24113=CARTESIAN_POINT('Ctrl Pts',(-41.4931114503555,37.1779982314699,38.264246504449));
#24114=CARTESIAN_POINT('Ctrl Pts',(-41.5072822388015,37.1971047149152,38.2835293026094));
#24115=CARTESIAN_POINT('Ctrl Pts',(-41.5213341567292,37.2164305449896,38.3026821168296));
#24116=CARTESIAN_POINT('Ctrl Pts',(-41.5352648324485,37.23597245988,38.3217017145054));
#24117=CARTESIAN_POINT('Ctrl Pts',(-40.7464147820825,36.4581565470228,37.2979655053874));
#24118=CARTESIAN_POINT('Ctrl Pts',(-40.7642173325444,36.4701658266656,37.3211077247104));
#24119=CARTESIAN_POINT('Ctrl Pts',(-40.7819375353008,36.4824509523723,37.3441700463492));
#24120=CARTESIAN_POINT('Ctrl Pts',(-40.7995722212268,36.4950097237531,37.3671483443542));
#24121=CARTESIAN_POINT('Ctrl Pts',(-40.8171912483704,36.5075573435279,37.3901062386973));
#24122=CARTESIAN_POINT('Ctrl Pts',(-40.834724910306,36.5203781231252,37.4129802583996));
#24123=CARTESIAN_POINT('Ctrl Pts',(-40.8521700759379,36.5334697701685,37.4357663179235));
#24124=CARTESIAN_POINT('Ctrl Pts',(-40.8696152415697,36.5465614172118,37.4585523774474));
#24125=CARTESIAN_POINT('Ctrl Pts',(-40.8869719108393,36.5599239316479,37.4812504767052));
#24126=CARTESIAN_POINT('Ctrl Pts',(-40.9042369848963,36.573554924843,37.5038565619471));
#24127=CARTESIAN_POINT('Ctrl Pts',(-40.9215020589534,36.5871859180381,37.526462647189));
#24128=CARTESIAN_POINT('Ctrl Pts',(-40.9386755377092,36.6010853899314,37.5489767183103));
#24129=CARTESIAN_POINT('Ctrl Pts',(-40.955754354397,36.6152508558148,37.5713947540483));
#24130=CARTESIAN_POINT('Ctrl Pts',(-40.9728331710848,36.629416321698,37.5938127897864));
#24131=CARTESIAN_POINT('Ctrl Pts',(-40.9898173256472,36.643847781515,37.6161347900547));
#24132=CARTESIAN_POINT('Ctrl Pts',(-41.0067037856659,36.6585426560188,37.6383567682013));
#24133=CARTESIAN_POINT('Ctrl Pts',(-41.0235902456846,36.6732375305227,37.6605787463478));
#24134=CARTESIAN_POINT('Ctrl Pts',(-41.0403790109508,36.6881958195721,37.6827007021974));
#24135=CARTESIAN_POINT('Ctrl Pts',(-41.0570670836403,36.7034148498235,37.7047186846361));
#24136=CARTESIAN_POINT('Ctrl Pts',(-41.0737551563299,36.7186338800749,37.7267366670747));
#24137=CARTESIAN_POINT('Ctrl Pts',(-41.0903425363719,36.7341136514639,37.748650676009));
#24138=CARTESIAN_POINT('Ctrl Pts',(-41.1068262618743,36.7498513976601,37.77045679743));
#24139=CARTESIAN_POINT('Ctrl Pts',(-41.1233099873767,36.7655891438563,37.792262918851));
#24140=CARTESIAN_POINT('Ctrl Pts',(-41.1396900584178,36.7815848648927,37.8139611527556));
#24141=CARTESIAN_POINT('Ctrl Pts',(-41.15596354979,36.7978357022364,37.835547623452));
#24142=CARTESIAN_POINT('Ctrl Pts',(-41.1722370411622,36.8140865395801,37.8571340941484));
#24143=CARTESIAN_POINT('Ctrl Pts',(-41.1884039528183,36.8305924931708,37.8786088015567));
#24144=CARTESIAN_POINT('Ctrl Pts',(-41.2044613981502,36.847350613883,37.8999679102104));
#24145=CARTESIAN_POINT('Ctrl Pts',(-41.220518843482,36.8641087345953,37.9213270188641));
#24146=CARTESIAN_POINT('Ctrl Pts',(-41.2364668222842,36.8811190222625,37.942570528589));
#24147=CARTESIAN_POINT('Ctrl Pts',(-41.2523024867352,36.8983784376388,37.9636946449994));
#24148=CARTESIAN_POINT('Ctrl Pts',(-41.2681381511862,36.9156378530152,37.9848187614099));
#24149=CARTESIAN_POINT('Ctrl Pts',(-41.2838615012189,36.9331463960273,38.0058234844164));
#24150=CARTESIAN_POINT('Ctrl Pts',(-41.2994697290819,36.9509009385799,38.0267050622299));
#24151=CARTESIAN_POINT('Ctrl Pts',(-41.3150779569449,36.9686554811326,38.0475866400434));
#24152=CARTESIAN_POINT('Ctrl Pts',(-41.330571062572,36.9866560231506,38.0683450725754));
#24153=CARTESIAN_POINT('Ctrl Pts',(-41.3459462792817,37.0048993488036,38.0889766519698));
#24154=CARTESIAN_POINT('Ctrl Pts',(-41.3613214959914,37.0231426744568,38.1096082313641));
#24155=CARTESIAN_POINT('Ctrl Pts',(-41.3765788237185,37.0416287836675,38.1301129575333));
#24156=CARTESIAN_POINT('Ctrl Pts',(-41.3917155378364,37.0603543740167,38.1504871678747));
#24157=CARTESIAN_POINT('Ctrl Pts',(-41.4068522519543,37.0790799643659,38.1708613782161));
#24158=CARTESIAN_POINT('Ctrl Pts',(-41.4218683523989,37.098045035774,38.1911050726434));
#24159=CARTESIAN_POINT('Ctrl Pts',(-41.4367611575687,37.1172462004086,38.2112146351116));
#24160=CARTESIAN_POINT('Ctrl Pts',(-41.4516539627386,37.1364473650431,38.2313241975799));
#24161=CARTESIAN_POINT('Ctrl Pts',(-41.4664234725707,37.1558846228228,38.251299628004));
#24162=CARTESIAN_POINT('Ctrl Pts',(-41.4810670494437,37.1755545017087,38.2711373581851));
#24163=CARTESIAN_POINT('Ctrl Pts',(-41.4957106263168,37.1952243805947,38.2909750883661));
#24164=CARTESIAN_POINT('Ctrl Pts',(-41.5102282701928,37.2151268805331,38.3106751182465));
#24165=CARTESIAN_POINT('Ctrl Pts',(-41.5246173883169,37.235258446453,38.330233928689));
#24166=CARTESIAN_POINT('Ctrl Pts',(-40.709927446472,36.4413634896317,37.2767259574961));
#24167=CARTESIAN_POINT('Ctrl Pts',(-40.7283423747484,36.4534559082533,37.3005623856167));
#24168=CARTESIAN_POINT('Ctrl Pts',(-40.7466718917616,36.4658409631829,37.324316242929));
#24169=CARTESIAN_POINT('Ctrl Pts',(-40.7649125306715,36.4785163085151,37.3479830356273));
#24170=CARTESIAN_POINT('Ctrl Pts',(-40.7831369727409,36.4911803987291,37.3716288133124));
#24171=CARTESIAN_POINT('Ctrl Pts',(-40.8012726943898,36.5041342639858,37.3951876808215));
#24172=CARTESIAN_POINT('Ctrl Pts',(-40.8193162714995,36.5173754553539,37.418655189126));
#24173=CARTESIAN_POINT('Ctrl Pts',(-40.8373598486091,36.530616646722,37.4421226974304));
#24174=CARTESIAN_POINT('Ctrl Pts',(-40.855311281094,36.5441451641385,37.465498846419));
#24175=CARTESIAN_POINT('Ctrl Pts',(-40.8731671796206,36.5579584503267,37.4887792215566));
#24176=CARTESIAN_POINT('Ctrl Pts',(-40.8910230781472,36.5717717365149,37.5120595966941));
#24177=CARTESIAN_POINT('Ctrl Pts',(-40.9087834426309,36.585869791409,37.5352441978702));
#24178=CARTESIAN_POINT('Ctrl Pts',(-40.9264449197973,36.6002499503495,37.5583286467043));
#24179=CARTESIAN_POINT('Ctrl Pts',(-40.9441063969636,36.6146301092899,37.5814130955383));
#24180=CARTESIAN_POINT('Ctrl Pts',(-40.961668986729,36.6292923722084,37.6043973919208));
#24181=CARTESIAN_POINT('Ctrl Pts',(-40.9791293731422,36.6442339680676,37.627277195275));
#24182=CARTESIAN_POINT('Ctrl Pts',(-40.9965897595554,36.6591755639269,37.6501569986292));
#24183=CARTESIAN_POINT('Ctrl Pts',(-41.0139479425334,36.674396492656,37.6729323088466));
#24184=CARTESIAN_POINT('Ctrl Pts',(-41.0312006446953,36.6898938778835,37.695598824788));
#24185=CARTESIAN_POINT('Ctrl Pts',(-41.0484533468572,36.7053912631111,37.7182653407295));
#24186=CARTESIAN_POINT('Ctrl Pts',(-41.0656005681211,36.7211651047637,37.7408230622875));
#24187=CARTESIAN_POINT('Ctrl Pts',(-41.0826390709103,36.7372124222201,37.7632677293804));
#24188=CARTESIAN_POINT('Ctrl Pts',(-41.0996775736996,36.7532597396764,37.7857123964734));
#24189=CARTESIAN_POINT('Ctrl Pts',(-41.1166073579336,36.7695805328605,37.8080440089949));
#24190=CARTESIAN_POINT('Ctrl Pts',(-41.1334252270582,36.7861717180241,37.8302583495245));
#24191=CARTESIAN_POINT('Ctrl Pts',(-41.1502430961829,36.8027629031877,37.852472690054));
#24192=CARTESIAN_POINT('Ctrl Pts',(-41.1669490501186,36.819624480252,37.8745697584863));
#24193=CARTESIAN_POINT('Ctrl Pts',(-41.1835399345382,36.8367532635039,37.8965453816507));
#24194=CARTESIAN_POINT('Ctrl Pts',(-41.2001308189578,36.8538820467558,37.9185210048151));
#24195=CARTESIAN_POINT('Ctrl Pts',(-41.2166066337826,36.871278036114,37.9403751826072));
#24196=CARTESIAN_POINT('Ctrl Pts',(-41.2329642680989,36.8889379451001,37.962103787677));
#24197=CARTESIAN_POINT('Ctrl Pts',(-41.2493219024152,36.9065978540862,37.9838323927467));
#24198=CARTESIAN_POINT('Ctrl Pts',(-41.2655613561456,36.9245216826165,38.005435424991));
#24199=CARTESIAN_POINT('Ctrl Pts',(-41.2816795629613,36.9427060446854,38.0269088044348));
#24200=CARTESIAN_POINT('Ctrl Pts',(-41.297797769777,36.9608904067542,38.0483821838785));
#24201=CARTESIAN_POINT('Ctrl Pts',(-41.3137947296017,36.9793353022755,38.0697259104199));
#24202=CARTESIAN_POINT('Ctrl Pts',(-41.3296674218458,36.998037246992,38.0909359529947));
#24203=CARTESIAN_POINT('Ctrl Pts',(-41.3455401140899,37.0167391917085,38.1121459955696));
#24204=CARTESIAN_POINT('Ctrl Pts',(-41.3612885386784,37.0356981855315,38.1332223540776));
#24205=CARTESIAN_POINT('Ctrl Pts',(-41.3769097218979,37.0549106472643,38.1541610478837));
#24206=CARTESIAN_POINT('Ctrl Pts',(-41.3925309051175,37.0741231089972,38.1750997416898));
#24207=CARTESIAN_POINT('Ctrl Pts',(-41.4080248468942,37.0935890385488,38.1959007706948));
#24208=CARTESIAN_POINT('Ctrl Pts',(-41.4233886215108,37.1133047591318,38.2165602061919));
#24209=CARTESIAN_POINT('Ctrl Pts',(-41.4387523961274,37.1330204797148,38.2372196416891));
#24210=CARTESIAN_POINT('Ctrl Pts',(-41.4539860035111,37.1529859912358,38.2577374835804));
#24211=CARTESIAN_POINT('Ctrl Pts',(-41.4690865670421,37.1731975227013,38.2781098565668));
#24212=CARTESIAN_POINT('Ctrl Pts',(-41.4841871305731,37.1934090541668,38.2984822295532));
#24213=CARTESIAN_POINT('Ctrl Pts',(-41.4991546501799,37.213866605481,38.318709133538));
#24214=CARTESIAN_POINT('Ctrl Pts',(-41.5139862994228,37.2345663128649,38.3387867480889));
#24215=CARTESIAN_POINT('Ctrl Pts',(-40.6741154471756,36.4255506093119,37.2563306872475));
#24216=CARTESIAN_POINT('Ctrl Pts',(-40.6931272967145,36.4377032948823,37.28084213635));
#24217=CARTESIAN_POINT('Ctrl Pts',(-40.7120508587019,36.4501655961227,37.3052685576269));
#24218=CARTESIAN_POINT('Ctrl Pts',(-40.7308823526258,36.4629350232734,37.3296050712103));
#24219=CARTESIAN_POINT('Ctrl Pts',(-40.7496971250573,36.4756931117658,37.3539199750994));
#24220=CARTESIAN_POINT('Ctrl Pts',(-40.7684199927572,36.488757780916,37.3781451307628));
#24221=CARTESIAN_POINT('Ctrl Pts',(-40.7870472219303,36.5021264253115,37.4022757071157));
#24222=CARTESIAN_POINT('Ctrl Pts',(-40.8056744511035,36.515495069707,37.4264062834685));
#24223=CARTESIAN_POINT('Ctrl Pts',(-40.8242060416511,36.5291676892768,37.4504422803829));
#24224=CARTESIAN_POINT('Ctrl Pts',(-40.8426382979243,36.5431415573687,37.4743789044973));
#24225=CARTESIAN_POINT('Ctrl Pts',(-40.8610705541975,36.5571154254606,37.4983155286117));
#24226=CARTESIAN_POINT('Ctrl Pts',(-40.8794034760984,36.5713905420004,37.5221527797991));
#24227=CARTESIAN_POINT('Ctrl Pts',(-40.8976334075967,36.585964060183,37.5458859043325));
#24228=CARTESIAN_POINT('Ctrl Pts',(-40.9158633390951,36.6005375783655,37.5696190288658));
#24229=CARTESIAN_POINT('Ctrl Pts',(-40.9339902800941,36.6154094981135,37.593248026619));
#24230=CARTESIAN_POINT('Ctrl Pts',(-40.9520106156417,36.6305768536049,37.6167681853963));
#24231=CARTESIAN_POINT('Ctrl Pts',(-40.9700309511894,36.6457442090964,37.6402883441736));
#24232=CARTESIAN_POINT('Ctrl Pts',(-40.98794468119,36.6612070002508,37.66369966385));
#24233=CARTESIAN_POINT('Ctrl Pts',(-41.0057482332104,36.6769621434121,37.6869974756397));
#24234=CARTESIAN_POINT('Ctrl Pts',(-41.0235517852309,36.6927172865733,37.7102952874294));
#24235=CARTESIAN_POINT('Ctrl Pts',(-41.041245159177,36.7087647816577,37.7334795912088));
#24236=CARTESIAN_POINT('Ctrl Pts',(-41.0588248265598,36.7251014284049,37.7565457634644));
#24237=CARTESIAN_POINT('Ctrl Pts',(-41.0764044939427,36.7414380751521,37.77961193572));
#24238=CARTESIAN_POINT('Ctrl Pts',(-41.0938704546694,36.7580638734756,37.8025599763297));
#24239=CARTESIAN_POINT('Ctrl Pts',(-41.1112192256027,36.7749755077871,37.8253853088963));
#24240=CARTESIAN_POINT('Ctrl Pts',(-41.1285679965361,36.7918871420986,37.848210641463));
#24241=CARTESIAN_POINT('Ctrl Pts',(-41.1457995775841,36.8090846123084,37.8709132658657));
#24242=CARTESIAN_POINT('Ctrl Pts',(-41.162910532351,36.8265644888233,37.8934886546498));
#24243=CARTESIAN_POINT('Ctrl Pts',(-41.180021487118,36.8440443653383,37.9160640434337));
#24244=CARTESIAN_POINT('Ctrl Pts',(-41.1970118155131,36.8618066480654,37.9385121964793));
#24245=CARTESIAN_POINT('Ctrl Pts',(-41.2138781292521,36.8798477947743,37.9608286370792));
#24246=CARTESIAN_POINT('Ctrl Pts',(-41.2307444429911,36.8978889414832,37.9831450776791));
#24247=CARTESIAN_POINT('Ctrl Pts',(-41.2474867419845,36.9162089520781,38.0053298057151));
#24248=CARTESIAN_POINT('Ctrl Pts',(-41.2641016874112,36.9348041731036,38.0273783970134));
#24249=CARTESIAN_POINT('Ctrl Pts',(-41.2807166328378,36.9533993941293,38.0494269883118));
#24250=CARTESIAN_POINT('Ctrl Pts',(-41.2972042246096,36.972269825487,38.0713394427555));
#24251=CARTESIAN_POINT('Ctrl Pts',(-41.3135611747002,36.9914117039544,38.0931113904688));
#24252=CARTESIAN_POINT('Ctrl Pts',(-41.3299181247909,37.0105535824219,38.1148833381822));
#24253=CARTESIAN_POINT('Ctrl Pts',(-41.3461444331136,37.0299669078974,38.1365147790498));
#24254=CARTESIAN_POINT('Ctrl Pts',(-41.3622368637482,37.0496478088925,38.1580013992367));
#24255=CARTESIAN_POINT('Ctrl Pts',(-41.3783292943828,37.0693287098876,38.1794880194235));
#24256=CARTESIAN_POINT('Ctrl Pts',(-41.3942878472441,37.0892771862976,38.2008298188158));
#24257=CARTESIAN_POINT('Ctrl Pts',(-41.4101093398088,37.109489259912,38.2220225413402));
#24258=CARTESIAN_POINT('Ctrl Pts',(-41.4259308323735,37.1297013335263,38.2432152638646));
#24259=CARTESIAN_POINT('Ctrl Pts',(-41.4416152645578,37.1501770042377,38.2642589094087));
#24260=CARTESIAN_POINT('Ctrl Pts',(-41.4571595085048,37.1709121886999,38.2851492813583));
#24261=CARTESIAN_POINT('Ctrl Pts',(-41.4727037524518,37.1916473731622,38.306039653308));
#24262=CARTESIAN_POINT('Ctrl Pts',(-41.4881078080792,37.2126420712653,38.3267767515524));
#24263=CARTESIAN_POINT('Ctrl Pts',(-41.5033686034439,37.2338920961565,38.3473564406104));
#24264=CARTESIAN_POINT('Ctrl Pts',(-40.6383034478792,36.4097377289922,37.2359354169989));
#24265=CARTESIAN_POINT('Ctrl Pts',(-40.6579122186806,36.4219506815113,37.2611218870834));
#24266=CARTESIAN_POINT('Ctrl Pts',(-40.6774298256422,36.4344902290624,37.2862208723249));
#24267=CARTESIAN_POINT('Ctrl Pts',(-40.69685217458,36.4473537380318,37.3112271067932));
#24268=CARTESIAN_POINT('Ctrl Pts',(-40.7162572773736,36.4602058248024,37.3362111368863));
#24269=CARTESIAN_POINT('Ctrl Pts',(-40.7355672911245,36.4733812978462,37.361102580704));
#24270=CARTESIAN_POINT('Ctrl Pts',(-40.7547781723612,36.4868773952691,37.3858962251053));
#24271=CARTESIAN_POINT('Ctrl Pts',(-40.7739890535979,36.500373492692,37.4106898695066));
#24272=CARTESIAN_POINT('Ctrl Pts',(-40.7931008022082,36.514190214415,37.4353857143468));
#24273=CARTESIAN_POINT('Ctrl Pts',(-40.812109416228,36.5283246644106,37.4599785874381));
#24274=CARTESIAN_POINT('Ctrl Pts',(-40.8311180302477,36.5424591144063,37.4845714605293));
#24275=CARTESIAN_POINT('Ctrl Pts',(-40.8500235095659,36.5569112925918,37.509061361728));
#24276=CARTESIAN_POINT('Ctrl Pts',(-40.8688218953962,36.5716781700165,37.5334431619606));
#24277=CARTESIAN_POINT('Ctrl Pts',(-40.8876202812265,36.5864450474411,37.5578249621932));
#24278=CARTESIAN_POINT('Ctrl Pts',(-40.9063115734591,36.6015266240186,37.5820986613173));
#24279=CARTESIAN_POINT('Ctrl Pts',(-40.9248918581412,36.6169197391423,37.6062591755176));
#24280=CARTESIAN_POINT('Ctrl Pts',(-40.9434721428234,36.6323128542659,37.630419689718));
#24281=CARTESIAN_POINT('Ctrl Pts',(-40.9619414198465,36.6480175078458,37.6544670188535));
#24282=CARTESIAN_POINT('Ctrl Pts',(-40.9802958217256,36.6640304089406,37.6783961264914));
#24283=CARTESIAN_POINT('Ctrl Pts',(-40.9986502236047,36.6800433100354,37.7023252341293));
#24284=CARTESIAN_POINT('Ctrl Pts',(-41.0168897502328,36.6963644585517,37.72613612013));
#24285=CARTESIAN_POINT('Ctrl Pts',(-41.0350105822093,36.7129904345898,37.7498237975483));
#24286=CARTESIAN_POINT('Ctrl Pts',(-41.0531314141859,36.7296164106278,37.7735114749666));
#24287=CARTESIAN_POINT('Ctrl Pts',(-41.0711335514053,36.7465472140907,37.7970759436644));
#24288=CARTESIAN_POINT('Ctrl Pts',(-41.0890132241472,36.7637792975502,37.8205122682682));
#24289=CARTESIAN_POINT('Ctrl Pts',(-41.1068928968892,36.7810113810095,37.843948592872));
#24290=CARTESIAN_POINT('Ctrl Pts',(-41.1246501050495,36.7985447443649,37.8672567732451));
#24291=CARTESIAN_POINT('Ctrl Pts',(-41.1422811301639,36.8163757141427,37.8904319276488));
#24292=CARTESIAN_POINT('Ctrl Pts',(-41.1599121552782,36.8342066839207,37.9136070820524));
#24293=CARTESIAN_POINT('Ctrl Pts',(-41.1774169972437,36.8523352600169,37.9366492103513));
#24294=CARTESIAN_POINT('Ctrl Pts',(-41.1947919904053,36.8707576444486,37.9595534864814));
#24295=CARTESIAN_POINT('Ctrl Pts',(-41.2121669835669,36.8891800288803,37.9824577626115));
#24296=CARTESIAN_POINT('Ctrl Pts',(-41.2294121278233,36.9078962215397,38.0052241864391));
#24297=CARTESIAN_POINT('Ctrl Pts',(-41.246523811861,36.926902301522,38.0278479895921));
#24298=CARTESIAN_POINT('Ctrl Pts',(-41.2636354958986,36.9459083815043,38.050471792745));
#24299=CARTESIAN_POINT('Ctrl Pts',(-41.2806137196176,36.9652043486984,38.0729529750912));
#24300=CARTESIAN_POINT('Ctrl Pts',(-41.2974549275547,36.9847861609168,38.095286827943));
#24301=CARTESIAN_POINT('Ctrl Pts',(-41.3142961354918,37.0043679731352,38.1176206807948));
#24302=CARTESIAN_POINT('Ctrl Pts',(-41.3310003275487,37.0242356302634,38.139807204022));
#24303=CARTESIAN_POINT('Ctrl Pts',(-41.3475640055984,37.0443849705206,38.1618417505897));
#24304=CARTESIAN_POINT('Ctrl Pts',(-41.3641276836481,37.0645343107778,38.1838762971574));
#24305=CARTESIAN_POINT('Ctrl Pts',(-41.380550847594,37.0849653340465,38.2057588669369));
#24306=CARTESIAN_POINT('Ctrl Pts',(-41.3968300581068,37.1056737606922,38.2274848764885));
#24307=CARTESIAN_POINT('Ctrl Pts',(-41.4131092686196,37.1263821873379,38.2492108860401));
#24308=CARTESIAN_POINT('Ctrl Pts',(-41.4292445256044,37.1473680172397,38.2707803352369));
#24309=CARTESIAN_POINT('Ctrl Pts',(-41.4452324499675,37.1686268546986,38.2921887061499));
#24310=CARTESIAN_POINT('Ctrl Pts',(-41.4612203743306,37.1898856921576,38.3135970770628));
#24311=CARTESIAN_POINT('Ctrl Pts',(-41.4770609659786,37.2114175370495,38.3348443695669));
#24312=CARTESIAN_POINT('Ctrl Pts',(-41.492750907465,37.2332178794481,38.3559261331319));
#24313=CARTESIAN_POINT('Ctrl Pts',(-40.6031670153025,36.3949061682344,37.2163852571093));
#24314=CARTESIAN_POINT('Ctrl Pts',(-40.623357249323,36.407156485292,37.2422275464382));
#24315=CARTESIAN_POINT('Ctrl Pts',(-40.643453630599,36.4197505664764,37.2679801100193));
#24316=CARTESIAN_POINT('Ctrl Pts',(-40.6634517347483,36.4326856357027,37.2936372773184));
#24317=CARTESIAN_POINT('Ctrl Pts',(-40.6834320815095,36.445609219188,37.319271662244));
#24318=CARTESIAN_POINT('Ctrl Pts',(-40.7033143254858,36.458873185345,37.3448108200719));
#24319=CARTESIAN_POINT('Ctrl Pts',(-40.7230940972037,36.4724746160314,37.3702491372292));
#24320=CARTESIAN_POINT('Ctrl Pts',(-40.7428738689217,36.4860760467178,37.3956874543864));
#24321=CARTESIAN_POINT('Ctrl Pts',(-40.7625511682547,36.5000149418463,37.4210249307097));
#24322=CARTESIAN_POINT('Ctrl Pts',(-40.78212167078,36.5142882351113,37.4462559969579));
#24323=CARTESIAN_POINT('Ctrl Pts',(-40.8016921733053,36.5285615283763,37.4714870632061));
#24324=CARTESIAN_POINT('Ctrl Pts',(-40.8211558789267,36.5431692197013,37.4966117192332));
#24325=CARTESIAN_POINT('Ctrl Pts',(-40.8405085100752,36.5581080959174,37.5216244425211));
#24326=CARTESIAN_POINT('Ctrl Pts',(-40.8598611412237,36.5730469721334,37.546637165809));
#24327=CARTESIAN_POINT('Ctrl Pts',(-40.8791026977786,36.5883170331452,37.571537956199));
#24328=CARTESIAN_POINT('Ctrl Pts',(-40.8982289511076,36.603914920437,37.5963213404317));
#24329=CARTESIAN_POINT('Ctrl Pts',(-40.9173552044367,36.6195128077287,37.6211047246645));
#24330=CARTESIAN_POINT('Ctrl Pts',(-40.9363661543852,36.6354385211834,37.6457707025633));
#24331=CARTESIAN_POINT('Ctrl Pts',(-40.9552576229183,36.6516885583113,37.6703138524221));
#24332=CARTESIAN_POINT('Ctrl Pts',(-40.9741490914513,36.6679385954392,37.6948570022809));
#24333=CARTESIAN_POINT('Ctrl Pts',(-40.9929210784476,36.6845129561356,37.719277323942));
#24334=CARTESIAN_POINT('Ctrl Pts',(-41.0115694583644,36.7014079955075,37.7435694496648));
#24335=CARTESIAN_POINT('Ctrl Pts',(-41.0302178382813,36.7183030348793,37.7678615753875));
#24336=CARTESIAN_POINT('Ctrl Pts',(-41.0487426109916,36.7355187528129,37.7920255050113));
#24337=CARTESIAN_POINT('Ctrl Pts',(-41.0671397052689,36.7530513636207,37.8160559271245));
#24338=CARTESIAN_POINT('Ctrl Pts',(-41.0855367995463,36.7705839744285,37.8400863492377));
#24339=CARTESIAN_POINT('Ctrl Pts',(-41.1038062152716,36.7884334779974,37.8639832636854));
#24340=CARTESIAN_POINT('Ctrl Pts',(-41.1219439372768,36.8065959494778,37.8877414176876));
#24341=CARTESIAN_POINT('Ctrl Pts',(-41.1400816592819,36.8247584209582,37.9114995716897));
#24342=CARTESIAN_POINT('Ctrl Pts',(-41.1580876874573,36.8432338602379,37.9351189650979));
#24343=CARTESIAN_POINT('Ctrl Pts',(-41.1759580644957,36.8620182050557,37.9585944060939));
#24344=CARTESIAN_POINT('Ctrl Pts',(-41.1938284415342,36.8808025498736,37.9820698470898));
#24345=CARTESIAN_POINT('Ctrl Pts',(-41.2115631673208,36.8998958001088,38.0054013355226));
#24346=CARTESIAN_POINT('Ctrl Pts',(-41.2291583441313,36.9192937578614,38.0285837428043));
#24347=CARTESIAN_POINT('Ctrl Pts',(-41.2467535209419,36.938691715614,38.051766150086));
#24348=CARTESIAN_POINT('Ctrl Pts',(-41.2642091486756,36.9583943807689,38.0747994760747));
#24349=CARTESIAN_POINT('Ctrl Pts',(-41.2815213908748,36.9783974216099,38.0976786576474));
#24350=CARTESIAN_POINT('Ctrl Pts',(-41.2988336330739,36.9984004624509,38.1205578392202));
#24351=CARTESIAN_POINT('Ctrl Pts',(-41.3160024896306,37.0187038788512,38.1432828762316));
#24352=CARTESIAN_POINT('Ctrl Pts',(-41.3330241871075,37.0393032072343,38.1658487732862));
#24353=CARTESIAN_POINT('Ctrl Pts',(-41.3500458845845,37.0599025356174,38.1884146703408));
#24354=CARTESIAN_POINT('Ctrl Pts',(-41.3669204228617,37.080797775842,38.2108214272873));
#24355=CARTESIAN_POINT('Ctrl Pts',(-41.3836440931108,37.1019843343765,38.2330641186097));
#24356=CARTESIAN_POINT('Ctrl Pts',(-41.4003677633599,37.1231708929111,38.2553068099321));
#24357=CARTESIAN_POINT('Ctrl Pts',(-41.4169405654734,37.1446487696193,38.2773854354873));
#24358=CARTESIAN_POINT('Ctrl Pts',(-41.4333588568789,37.1664132430457,38.2992951418114));
#24359=CARTESIAN_POINT('Ctrl Pts',(-41.4497771482844,37.1881777164722,38.3212048481356));
#24360=CARTESIAN_POINT('Ctrl Pts',(-41.4660409288741,37.2102287864741,38.3429456350853));
#24361=CARTESIAN_POINT('Ctrl Pts',(-41.4821466239335,37.2325616057495,38.3645127233828));
#24362=CARTESIAN_POINT('Ctrl Pts',(-40.5686122648838,36.3808986978976,37.1975487055119));
#24363=CARTESIAN_POINT('Ctrl Pts',(-40.5893703835316,36.3931671620808,37.2240302748371));
#24364=CARTESIAN_POINT('Ctrl Pts',(-40.6100321454547,36.4057967134211,37.2504200896056));
#24365=CARTESIAN_POINT('Ctrl Pts',(-40.630592780513,36.4187844360772,37.2767120572633));
#24366=CARTESIAN_POINT('Ctrl Pts',(-40.6511351586819,36.4317606262385,37.3029806788743));
#24367=CARTESIAN_POINT('Ctrl Pts',(-40.6715765893685,36.4450943518338,37.3291516268873));
#24368=CARTESIAN_POINT('Ctrl Pts',(-40.6919123616709,36.4587825399943,37.3552188699908));
#24369=CARTESIAN_POINT('Ctrl Pts',(-40.7122481339734,36.4724707281547,37.3812861130943));
#24370=CARTESIAN_POINT('Ctrl Pts',(-40.7324782477483,36.4865133787835,37.4072496511039));
#24371=CARTESIAN_POINT('Ctrl Pts',(-40.7525980408097,36.5009072556416,37.4331035005162));
#24372=CARTESIAN_POINT('Ctrl Pts',(-40.7727178338711,36.5153011324998,37.4589573499286));
#24373=CARTESIAN_POINT('Ctrl Pts',(-40.7927273061048,36.5300462354996,37.4847015105758));
#24374=CARTESIAN_POINT('Ctrl Pts',(-40.8126218461008,36.5451391664803,37.5103300494723));
#24375=CARTESIAN_POINT('Ctrl Pts',(-40.8325163860967,36.5602320974612,37.5359585883689));
#24376=CARTESIAN_POINT('Ctrl Pts',(-40.8522959937176,36.5756728563167,37.5614715053352));
#24377=CARTESIAN_POINT('Ctrl Pts',(-40.8719561106524,36.5914578846304,37.5868629207453));
#24378=CARTESIAN_POINT('Ctrl Pts',(-40.8916162275871,36.607242912944,37.6122543361554));
#24379=CARTESIAN_POINT('Ctrl Pts',(-40.9111568536662,36.6233722105883,37.6375242498129));
#24380=CARTESIAN_POINT('Ctrl Pts',(-40.9305734855941,36.6398420604359,37.6626668380618));
#24381=CARTESIAN_POINT('Ctrl Pts',(-40.949990117522,36.6563119102835,37.6878094263107));
#24382=CARTESIAN_POINT('Ctrl Pts',(-40.9692827551612,36.6731223122178,37.7128246889728));
#24383=CARTESIAN_POINT('Ctrl Pts',(-40.9884469523672,36.6902693921455,37.7377068610782));
#24384=CARTESIAN_POINT('Ctrl Pts',(-41.0076111495731,36.7074164720732,37.7625890331836));
#24385=CARTESIAN_POINT('Ctrl Pts',(-41.026646906203,36.7249002298684,37.7873381145518));
#24386=CARTESIAN_POINT('Ctrl Pts',(-41.0455498353268,36.7427166362666,37.8119484015653));
#24387=CARTESIAN_POINT('Ctrl Pts',(-41.0644527644507,36.7605330426647,37.8365586885788));
#24388=CARTESIAN_POINT('Ctrl Pts',(-41.0832228659336,36.7786820975395,37.861030181063));
#24389=CARTESIAN_POINT('Ctrl Pts',(-41.1018558140411,36.7971596182853,37.885357239356));
#24390=CARTESIAN_POINT('Ctrl Pts',(-41.1204887621484,36.8156371390313,37.909684297649));
#24391=CARTESIAN_POINT('Ctrl Pts',(-41.1389845567548,36.8344431255219,37.9338669215827));
#24392=CARTESIAN_POINT('Ctrl Pts',(-41.1573389353545,36.8535732437653,37.9578995380755));
#24393=CARTESIAN_POINT('Ctrl Pts',(-41.1756933139542,36.8727033620086,37.9819321545683));
#24394=CARTESIAN_POINT('Ctrl Pts',(-41.1939062764172,36.8921576118694,38.0058147634501));
#24395=CARTESIAN_POINT('Ctrl Pts',(-41.2119736254189,36.911931509958,38.0295418607802));
#24396=CARTESIAN_POINT('Ctrl Pts',(-41.2300409744206,36.9317054080466,38.0532689581103));
#24397=CARTESIAN_POINT('Ctrl Pts',(-41.2479627098447,36.951798954232,38.0768405437274));
#24398=CARTESIAN_POINT('Ctrl Pts',(-41.2657347014578,36.9722075177754,38.1002511853549));
#24399=CARTESIAN_POINT('Ctrl Pts',(-41.283506693071,36.9926160813189,38.1236618269823));
#24400=CARTESIAN_POINT('Ctrl Pts',(-41.3011289407505,37.0133396620775,38.1469115244559));
#24401=CARTESIAN_POINT('Ctrl Pts',(-41.3185973833262,37.0343734841502,38.169994919706));
#24402=CARTESIAN_POINT('Ctrl Pts',(-41.336065825902,37.0554073062227,38.1930783149561));
#24403=CARTESIAN_POINT('Ctrl Pts',(-41.3533804632401,37.0767513694522,38.2159954078134));
#24404=CARTESIAN_POINT('Ctrl Pts',(-41.3705373050422,37.0984007549263,38.2387409168482));
#24405=CARTESIAN_POINT('Ctrl Pts',(-41.3876941468442,37.1200501404005,38.2614864258829));
#24406=CARTESIAN_POINT('Ctrl Pts',(-41.4046931929887,37.142004847966,38.284060350934));
#24407=CARTESIAN_POINT('Ctrl Pts',(-41.4215305259077,37.1642598179827,38.3064574896577));
#24408=CARTESIAN_POINT('Ctrl Pts',(-41.4383678588268,37.1865147879992,38.3288546283815));
#24409=CARTESIAN_POINT('Ctrl Pts',(-41.455043478399,37.2090700203066,38.3510749806165));
#24410=CARTESIAN_POINT('Ctrl Pts',(-41.4715535415974,37.2319203168746,38.3731134255079));
#24411=CARTESIAN_POINT('Ctrl Pts',(-40.4995027640465,36.3528837572238,37.1598756023172));
#24412=CARTESIAN_POINT('Ctrl Pts',(-40.5213966519487,36.3651885156582,37.187635731635));
#24413=CARTESIAN_POINT('Ctrl Pts',(-40.5431891751662,36.3778890073104,37.2153000487784));
#24414=CARTESIAN_POINT('Ctrl Pts',(-40.5648748720426,36.3909820368262,37.2428616171533));
#24415=CARTESIAN_POINT('Ctrl Pts',(-40.5865413130269,36.4040634403395,37.2703987121349));
#24416=CARTESIAN_POINT('Ctrl Pts',(-40.6081011171338,36.4175366848114,37.297833240518));
#24417=CARTESIAN_POINT('Ctrl Pts',(-40.6295488906053,36.43139838792,37.325158335514));
#24418=CARTESIAN_POINT('Ctrl Pts',(-40.6509966640768,36.4452600910285,37.35248343051));
#24419=CARTESIAN_POINT('Ctrl Pts',(-40.6723324067354,36.459510252658,37.3796990918922));
#24420=CARTESIAN_POINT('Ctrl Pts',(-40.6935507808691,36.4741452967023,37.4067985076328));
#24421=CARTESIAN_POINT('Ctrl Pts',(-40.7147691550028,36.4887803407466,37.4338979233734));
#24422=CARTESIAN_POINT('Ctrl Pts',(-40.7358701604611,36.5038002670961,37.4608810932608));
#24423=CARTESIAN_POINT('Ctrl Pts',(-40.756848518152,36.5192013076064,37.4877412633747));
#24424=CARTESIAN_POINT('Ctrl Pts',(-40.7778268758429,36.5346023481166,37.5146014334885));
#24425=CARTESIAN_POINT('Ctrl Pts',(-40.7986825855956,36.5503845026598,37.5413386036076));
#24426=CARTESIAN_POINT('Ctrl Pts',(-40.8194104297418,36.5665438130171,37.5679460813723));
#24427=CARTESIAN_POINT('Ctrl Pts',(-40.840138273888,36.5827031233745,37.5945535591371));
#24428=CARTESIAN_POINT('Ctrl Pts',(-40.8607382522283,36.5992395893979,37.6210313443123));
#24429=CARTESIAN_POINT('Ctrl Pts',(-40.8812052109459,36.6161490646851,37.6473728093412));
#24430=CARTESIAN_POINT('Ctrl Pts',(-40.9016721696634,36.6330585399722,37.6737142743702));
#24431=CARTESIAN_POINT('Ctrl Pts',(-40.9220061085886,36.6503410243821,37.6999194190343));
#24432=CARTESIAN_POINT('Ctrl Pts',(-40.9422019403726,36.6679921854215,37.725981683905));
#24433=CARTESIAN_POINT('Ctrl Pts',(-40.9623977721567,36.6856433464611,37.7520439487757));
#24434=CARTESIAN_POINT('Ctrl Pts',(-40.9824554966259,36.7036631839793,37.7779633336328));
#24435=CARTESIAN_POINT('Ctrl Pts',(-41.0023700954427,36.7220471815582,37.8037333504469));
#24436=CARTESIAN_POINT('Ctrl Pts',(-41.0222846942595,36.740431179137,37.8295033672612));
#24437=CARTESIAN_POINT('Ctrl Pts',(-41.0420561672579,36.7591793366235,37.8551240158183));
#24438=CARTESIAN_POINT('Ctrl Pts',(-41.0616795675697,36.7782869559004,37.8805888826929));
#24439=CARTESIAN_POINT('Ctrl Pts',(-41.0813029678815,36.7973945751773,37.9060537495676));
#24440=CARTESIAN_POINT('Ctrl Pts',(-41.1007782953498,36.8168616560897,37.9313628345522));
#24441=CARTESIAN_POINT('Ctrl Pts',(-41.1201006770721,36.8366833211842,37.9565098020388));
#24442=CARTESIAN_POINT('Ctrl Pts',(-41.1394230587942,36.8565049862788,37.9816567695253));
#24443=CARTESIAN_POINT('Ctrl Pts',(-41.15859249461,36.8766812353907,38.006641619305));
#24444=CARTESIAN_POINT('Ctrl Pts',(-41.1776041879939,36.8972070141512,38.0314580967319));
#24445=CARTESIAN_POINT('Ctrl Pts',(-41.1966158813778,36.9177327929118,38.0562745741588));
#24446=CARTESIAN_POINT('Ctrl Pts',(-41.2154698321827,36.9386081011583,38.0809226790329));
#24447=CARTESIAN_POINT('Ctrl Pts',(-41.2341613226239,36.9598277101066,38.1053962407698));
#24448=CARTESIAN_POINT('Ctrl Pts',(-41.2528528130651,36.9810473190549,38.1298698025067));
#24449=CARTESIAN_POINT('Ctrl Pts',(-41.2713818429903,37.0026112285302,38.1541688209045));
#24450=CARTESIAN_POINT('Ctrl Pts',(-41.2897437757637,37.0245140379819,38.1782872125456));
#24451=CARTESIAN_POINT('Ctrl Pts',(-41.308105708537,37.0464168474336,38.2024056041867));
#24452=CARTESIAN_POINT('Ctrl Pts',(-41.3263005439969,37.0686585566726,38.2263433688655));
#24453=CARTESIAN_POINT('Ctrl Pts',(-41.3443237289049,37.0912335960259,38.250094513325));
#24454=CARTESIAN_POINT('Ctrl Pts',(-41.3623469138128,37.1138086353793,38.2738456577845));
#24455=CARTESIAN_POINT('Ctrl Pts',(-41.3801984480191,37.1367170046594,38.2974101818276));
#24456=CARTESIAN_POINT('Ctrl Pts',(-41.3978738639654,37.1599529678564,38.3207821853503));
#24457=CARTESIAN_POINT('Ctrl Pts',(-41.4155492799117,37.1831889310534,38.3441541888731));
#24458=CARTESIAN_POINT('Ctrl Pts',(-41.433048577449,37.2067524879717,38.3673336716789));
#24459=CARTESIAN_POINT('Ctrl Pts',(-41.4503673769252,37.2306377391247,38.3903148297581));
#24460=CARTESIAN_POINT('Ctrl Pts',(-40.4327066305705,36.3281417176076,37.1250374865186));
#24461=CARTESIAN_POINT('Ctrl Pts',(-40.4556822337068,36.3404064517208,37.1540104055611));
#24462=CARTESIAN_POINT('Ctrl Pts',(-40.4785522041448,36.3531021756841,37.1828843032254));
#24463=CARTESIAN_POINT('Ctrl Pts',(-40.5013103265027,36.3662254256052,37.2116513292939));
#24464=CARTESIAN_POINT('Ctrl Pts',(-40.5240482407043,36.3793370226897,37.2403928115787));
#24465=CARTESIAN_POINT('Ctrl Pts',(-40.5466745051614,36.3928753866999,37.2690276117041));
#24466=CARTESIAN_POINT('Ctrl Pts',(-40.5691829815726,36.4068368320582,37.2975479582549));
#24467=CARTESIAN_POINT('Ctrl Pts',(-40.591691457984,36.4207982774164,37.3260683048058));
#24468=CARTESIAN_POINT('Ctrl Pts',(-40.6140821461322,36.4351828039857,37.3544741975048));
#24469=CARTESIAN_POINT('Ctrl Pts',(-40.6363489717272,36.449986497345,37.3827579271217));
#24470=CARTESIAN_POINT('Ctrl Pts',(-40.6586157973222,36.4647901907043,37.4110416567386));
#24471=CARTESIAN_POINT('Ctrl Pts',(-40.680758760124,36.4800130506985,37.4392032229855));
#24472=CARTESIAN_POINT('Ctrl Pts',(-40.7027718529873,36.4956509361219,37.4672349829013));
#24473=CARTESIAN_POINT('Ctrl Pts',(-40.7247849458505,36.5112888215454,37.495266742817));
#24474=CARTESIAN_POINT('Ctrl Pts',(-40.7466681685606,36.5273417322445,37.5231686961282));
#24475=CARTESIAN_POINT('Ctrl Pts',(-40.7684155844015,36.543805302488,37.5509332702886));
#24476=CARTESIAN_POINT('Ctrl Pts',(-40.7901630002423,36.5602688727316,37.5786978444489));
#24477=CARTESIAN_POINT('Ctrl Pts',(-40.8117746090018,36.577143102358,37.6063250391875));
#24478=CARTESIAN_POINT('Ctrl Pts',(-40.8332445475919,36.5944234034702,37.6338073564561));
#24479=CARTESIAN_POINT('Ctrl Pts',(-40.8547144861819,36.6117037045823,37.6612896737247));
#24480=CARTESIAN_POINT('Ctrl Pts',(-40.8760427543934,36.6293900770107,37.6886271132553));
#24481=CARTESIAN_POINT('Ctrl Pts',(-40.897223565927,36.6474777131718,37.7158122555411));
#24482=CARTESIAN_POINT('Ctrl Pts',(-40.9184043774606,36.6655653493329,37.7429973978269));
#24483=CARTESIAN_POINT('Ctrl Pts',(-40.9394377321161,36.684054249053,37.7700302426063));
#24484=CARTESIAN_POINT('Ctrl Pts',(-40.9603179234896,36.7029393876519,37.7969034529082));
#24485=CARTESIAN_POINT('Ctrl Pts',(-40.9811981148631,36.7218245262507,37.8237766632102));
#24486=CARTESIAN_POINT('Ctrl Pts',(-41.0019251427519,36.7411059035437,37.8504902387728));
#24487=CARTESIAN_POINT('Ctrl Pts',(-41.0224933837594,36.7607782804895,37.8770369291384));
#24488=CARTESIAN_POINT('Ctrl Pts',(-41.0430616247668,36.7804506574353,37.9035836195039));
#24489=CARTESIAN_POINT('Ctrl Pts',(-41.0634710786868,36.800514033838,37.9299634244099));
#24490=CARTESIAN_POINT('Ctrl Pts',(-41.0837162081265,36.820962959103,37.9561691838015));
#24491=CARTESIAN_POINT('Ctrl Pts',(-41.1039613375662,36.841411884368,37.9823749431932));
#24492=CARTESIAN_POINT('Ctrl Pts',(-41.1240421423282,36.8622463582954,38.0084066568147));
#24493=CARTESIAN_POINT('Ctrl Pts',(-41.1439531740197,36.8834607216871,38.0342572588823));
#24494=CARTESIAN_POINT('Ctrl Pts',(-41.1638642057111,36.9046750850788,38.0601078609499));
#24495=CARTESIAN_POINT('Ctrl Pts',(-41.1836054641379,36.9262693377276,38.0857773512114));
#24496=CARTESIAN_POINT('Ctrl Pts',(-41.2031715928443,36.9482376148864,38.1112587619649));
#24497=CARTESIAN_POINT('Ctrl Pts',(-41.2227377215506,36.9702058920454,38.1367401727183));
#24498=CARTESIAN_POINT('Ctrl Pts',(-41.2421287203456,36.9925481934999,38.1620335037149));
#24499=CARTESIAN_POINT('Ctrl Pts',(-41.2613393275985,37.0152584521198,38.1871318890929));
#24500=CARTESIAN_POINT('Ctrl Pts',(-41.2805499348514,37.0379687107396,38.2122302744709));
#24501=CARTESIAN_POINT('Ctrl Pts',(-41.2995801503747,37.061046926303,38.2371337139852));
#24502=CARTESIAN_POINT('Ctrl Pts',(-41.3184248101988,37.0844868325701,38.2618354473172));
#24503=CARTESIAN_POINT('Ctrl Pts',(-41.3372694700231,37.1079267388372,38.2865371806492));
#24504=CARTESIAN_POINT('Ctrl Pts',(-41.3559285739644,37.131728335579,38.3110372075577));
#24505=CARTESIAN_POINT('Ctrl Pts',(-41.3743970584991,37.1558851608273,38.3353288769137));
#24506=CARTESIAN_POINT('Ctrl Pts',(-41.3928655430338,37.1800419860756,38.3596205462697));
#24507=CARTESIAN_POINT('Ctrl Pts',(-41.4111434079833,37.2045540395965,38.3837038578382));
#24508=CARTESIAN_POINT('Ctrl Pts',(-41.4292256929962,37.2294146671748,38.4075722732637));
#24509=CARTESIAN_POINT('Ctrl Pts',(-40.3676750517867,36.3058114897981,37.0923047496203));
#24510=CARTESIAN_POINT('Ctrl Pts',(-40.3916895837106,36.3179798469043,37.1224397291744));
#24511=CARTESIAN_POINT('Ctrl Pts',(-40.4155949225065,36.3306148746499,37.1524732849664));
#24512=CARTESIAN_POINT('Ctrl Pts',(-40.4393840426075,36.3437128595723,37.1823965903769));
#24513=CARTESIAN_POINT('Ctrl Pts',(-40.4631520390742,36.3567992140922,37.2122933252813));
#24514=CARTESIAN_POINT('Ctrl Pts',(-40.4868040228878,36.3703477038401,37.2420800051752));
#24515=CARTESIAN_POINT('Ctrl Pts',(-40.5103330551856,36.384354354058,37.271747891473));
#24516=CARTESIAN_POINT('Ctrl Pts',(-40.5338620874834,36.3983610042759,37.3014157777707));
#24517=CARTESIAN_POINT('Ctrl Pts',(-40.5572681679973,36.4128258148029,37.3309648701328));
#24518=CARTESIAN_POINT('Ctrl Pts',(-40.5805444300924,36.4277445420935,37.3603864997192));
#24519=CARTESIAN_POINT('Ctrl Pts',(-40.6038206921875,36.4426632693841,37.3898081293055));
#24520=CARTESIAN_POINT('Ctrl Pts',(-40.6269671355757,36.4580359132583,37.4191022957678));
#24521=CARTESIAN_POINT('Ctrl Pts',(-40.6499769697499,36.4738579638206,37.4482604050325));
#24522=CARTESIAN_POINT('Ctrl Pts',(-40.6729868039241,36.4896800143829,37.4774185142971));
#24523=CARTESIAN_POINT('Ctrl Pts',(-40.6958600286203,36.5059514714516,37.5064405660295));
#24524=CARTESIAN_POINT('Ctrl Pts',(-40.7185899334867,36.5226675614453,37.5353180459871));
#24525=CARTESIAN_POINT('Ctrl Pts',(-40.741319838353,36.5393836514389,37.5641955259447));
#24526=CARTESIAN_POINT('Ctrl Pts',(-40.7639064231285,36.5565443741655,37.592928433796));
#24527=CARTESIAN_POINT('Ctrl Pts',(-40.786343061553,36.5741446951584,37.6215083401248));
#24528=CARTESIAN_POINT('Ctrl Pts',(-40.8087796999776,36.5917450161511,37.6500882464537));
#24529=CARTESIAN_POINT('Ctrl Pts',(-40.8310663917936,36.6097849352079,37.6785151509322));
#24530=CARTESIAN_POINT('Ctrl Pts',(-40.8531965987211,36.628259159931,37.7067807139168));
#24531=CARTESIAN_POINT('Ctrl Pts',(-40.8753268056486,36.646733384654,37.7350462769015));
#24532=CARTESIAN_POINT('Ctrl Pts',(-40.8973005274392,36.6656419148345,37.7631504980711));
#24533=CARTESIAN_POINT('Ctrl Pts',(-40.9191113176179,36.6849792032419,37.7910851324419));
#24534=CARTESIAN_POINT('Ctrl Pts',(-40.9409221077965,36.7043164916494,37.8190197668126));
#24535=CARTESIAN_POINT('Ctrl Pts',(-40.9625699661137,36.724082538062,37.8467848140641));
#24536=CARTESIAN_POINT('Ctrl Pts',(-40.9840485417151,36.7442715436917,37.8743721287291));
#24537=CARTESIAN_POINT('Ctrl Pts',(-41.0055271173165,36.7644605493214,37.9019594433941));
#24538=CARTESIAN_POINT('Ctrl Pts',(-41.0268364099504,36.7850725139334,37.9293690251529));
#24539=CARTESIAN_POINT('Ctrl Pts',(-41.0479701680778,36.8061013905645,37.9565928328155));
#24540=CARTESIAN_POINT('Ctrl Pts',(-41.0691039262052,36.8271302671957,37.9838166404781));
#24541=CARTESIAN_POINT('Ctrl Pts',(-41.0900621495836,36.8485760556048,38.0108546737322));
#24542=CARTESIAN_POINT('Ctrl Pts',(-41.1108386896676,36.8704324642089,38.0376990003894));
#24543=CARTESIAN_POINT('Ctrl Pts',(-41.1316152297516,36.892288872813,38.0645433270466));
#24544=CARTESIAN_POINT('Ctrl Pts',(-41.1522100863028,36.9145559013613,38.0911939467988));
#24545=CARTESIAN_POINT('Ctrl Pts',(-41.1726172173773,36.9372270173422,38.1176430411141));
#24546=CARTESIAN_POINT('Ctrl Pts',(-41.1930243484518,36.959898133323,38.1440921354294));
#24547=CARTESIAN_POINT('Ctrl Pts',(-41.2132437538154,36.9829733364764,38.170339704004));
#24548=CARTESIAN_POINT('Ctrl Pts',(-41.2332695016711,37.0064458571953,38.1963780465497));
#24549=CARTESIAN_POINT('Ctrl Pts',(-41.2532952495268,37.0299183779144,38.2224163890953));
#24550=CARTESIAN_POINT('Ctrl Pts',(-41.2731273396446,37.0537882159297,38.2482455053131));
#24551=CARTESIAN_POINT('Ctrl Pts',(-41.2927599538546,37.0780483685113,38.2738578176767));
#24552=CARTESIAN_POINT('Ctrl Pts',(-41.3123925680647,37.1023085210928,38.2994701300402));
#24553=CARTESIAN_POINT('Ctrl Pts',(-41.3318257061416,37.1269589879621,38.3248656382556));
#24554=CARTESIAN_POINT('Ctrl Pts',(-41.3510536669568,37.151992537375,38.3500368920045));
#24555=CARTESIAN_POINT('Ctrl Pts',(-41.3702816277719,37.1770260867878,38.3752081457535));
#24556=CARTESIAN_POINT('Ctrl Pts',(-41.3893044111062,37.202442718459,38.4001551447491));
#24557=CARTESIAN_POINT('Ctrl Pts',(-41.4081164362138,37.228234975869,38.4248705702491));
#24558=CARTESIAN_POINT('Ctrl Pts',(-40.3026434730029,36.2834812619887,37.0595720127219));
#24559=CARTESIAN_POINT('Ctrl Pts',(-40.3276969337144,36.2955532420878,37.0908690527878));
#24560=CARTESIAN_POINT('Ctrl Pts',(-40.3526376408682,36.3081275736156,37.1220622667074));
#24561=CARTESIAN_POINT('Ctrl Pts',(-40.3774577587123,36.3212002935394,37.1531418514599));
#24562=CARTESIAN_POINT('Ctrl Pts',(-40.402255837444,36.3342614054947,37.184193838984));
#24563=CARTESIAN_POINT('Ctrl Pts',(-40.4269335406142,36.3478200209803,37.2151323986463));
#24564=CARTESIAN_POINT('Ctrl Pts',(-40.4514831287985,36.3618718760578,37.245947824691));
#24565=CARTESIAN_POINT('Ctrl Pts',(-40.4760327169828,36.3759237311353,37.2767632507357));
#24566=CARTESIAN_POINT('Ctrl Pts',(-40.5004541898623,36.3904688256201,37.3074555427608));
#24567=CARTESIAN_POINT('Ctrl Pts',(-40.5247398884576,36.405502586842,37.3380150723166));
#24568=CARTESIAN_POINT('Ctrl Pts',(-40.5490255870529,36.4205363480638,37.3685746018725));
#24569=CARTESIAN_POINT('Ctrl Pts',(-40.5731755110274,36.436058775818,37.3990013685501));
#24570=CARTESIAN_POINT('Ctrl Pts',(-40.5971820865126,36.4520649915192,37.4292858271637));
#24571=CARTESIAN_POINT('Ctrl Pts',(-40.6211886619977,36.4680712072204,37.4595702857772));
#24572=CARTESIAN_POINT('Ctrl Pts',(-40.64505188868,36.4845612106588,37.4897124359308));
#24573=CARTESIAN_POINT('Ctrl Pts',(-40.6687642825718,36.5015298204025,37.5197028216856));
#24574=CARTESIAN_POINT('Ctrl Pts',(-40.6924766764637,36.5184984301463,37.5496932074404));
#24575=CARTESIAN_POINT('Ctrl Pts',(-40.7160382372553,36.535945645973,37.5795318284044));
#24576=CARTESIAN_POINT('Ctrl Pts',(-40.7394415755142,36.5538659868465,37.6092093237936));
#24577=CARTESIAN_POINT('Ctrl Pts',(-40.7628449137732,36.5717863277199,37.6388868191827));
#24578=CARTESIAN_POINT('Ctrl Pts',(-40.7860900291939,36.5901797934051,37.6684031886092));
#24579=CARTESIAN_POINT('Ctrl Pts',(-40.8091696315152,36.6090406066902,37.6977491722927));
#24580=CARTESIAN_POINT('Ctrl Pts',(-40.8322492338366,36.6279014199752,37.7270951559761));
#24581=CARTESIAN_POINT('Ctrl Pts',(-40.8551633227623,36.647229580616,37.756270753536));
#24582=CARTESIAN_POINT('Ctrl Pts',(-40.8779047117461,36.667019018832,37.7852668119755));
#24583=CARTESIAN_POINT('Ctrl Pts',(-40.9006461007299,36.686808457048,37.814262870415));
#24584=CARTESIAN_POINT('Ctrl Pts',(-40.9232147894755,36.7070591725803,37.8430793893553));
#24585=CARTESIAN_POINT('Ctrl Pts',(-40.9456036996708,36.7277648068939,37.8717073283198));
#24586=CARTESIAN_POINT('Ctrl Pts',(-40.9679926098661,36.7484704412076,37.9003352672843));
#24587=CARTESIAN_POINT('Ctrl Pts',(-40.990201741214,36.7696309940287,37.9287746258959));
#24588=CARTESIAN_POINT('Ctrl Pts',(-41.0122241280291,36.7912398220261,37.9570164818294));
#24589=CARTESIAN_POINT('Ctrl Pts',(-41.0342465148442,36.8128486500235,37.9852583377631));
#24590=CARTESIAN_POINT('Ctrl Pts',(-41.0560821568389,36.8349057529144,38.0133026906496));
#24591=CARTESIAN_POINT('Ctrl Pts',(-41.0777242053154,36.8574042067308,38.0411407418964));
#24592=CARTESIAN_POINT('Ctrl Pts',(-41.099366253792,36.8799026605473,38.0689787931431));
#24593=CARTESIAN_POINT('Ctrl Pts',(-41.1208147084676,36.902842464995,38.0966105423863));
#24594=CARTESIAN_POINT('Ctrl Pts',(-41.1420628419104,36.9262164197978,38.1240273202634));
#24595=CARTESIAN_POINT('Ctrl Pts',(-41.1633109753531,36.9495903746006,38.1514440981405));
#24596=CARTESIAN_POINT('Ctrl Pts',(-41.1843587872853,36.9733984794528,38.1786459042931));
#24597=CARTESIAN_POINT('Ctrl Pts',(-41.2051996757437,36.997633262271,38.2056242040064));
#24598=CARTESIAN_POINT('Ctrl Pts',(-41.2260405642022,37.0218680450892,38.2326025037197));
#24599=CARTESIAN_POINT('Ctrl Pts',(-41.2466745289145,37.0465295055564,38.259357296641));
#24600=CARTESIAN_POINT('Ctrl Pts',(-41.2670950975103,37.0716099044525,38.2858801880361));
#24601=CARTESIAN_POINT('Ctrl Pts',(-41.2875156661062,37.0966903033485,38.3124030794313));
#24602=CARTESIAN_POINT('Ctrl Pts',(-41.3077228383188,37.1221896403453,38.3386940689535));
#24603=CARTESIAN_POINT('Ctrl Pts',(-41.3277102754144,37.1480999139227,38.3647449070954));
#24604=CARTESIAN_POINT('Ctrl Pts',(-41.34769771251,37.1740101875002,38.3907957452372));
#24605=CARTESIAN_POINT('Ctrl Pts',(-41.367465414229,37.2003313973215,38.41660643166));
#24606=CARTESIAN_POINT('Ctrl Pts',(-41.3870071794313,37.2270552845631,38.4421688672345));
#24607=CARTESIAN_POINT('Ctrl Pts',(-40.2393823361708,36.2635753108104,37.028954656999));
#24608=CARTESIAN_POINT('Ctrl Pts',(-40.2654318337543,36.2754942589355,37.061362837691));
#24609=CARTESIAN_POINT('Ctrl Pts',(-40.2913657242679,36.2879516667465,37.09366559612));
#24610=CARTESIAN_POINT('Ctrl Pts',(-40.3171753053395,36.3009433405593,37.1258520900638));
#24611=CARTESIAN_POINT('Ctrl Pts',(-40.3429619687014,36.3139234783688,37.1580100038952));
#24612=CARTESIAN_POINT('Ctrl Pts',(-40.3686245428996,36.3274369336001,37.1900518591446));
#24613=CARTESIAN_POINT('Ctrl Pts',(-40.3941544318464,36.3414791671208,37.2219669202645));
#24614=CARTESIAN_POINT('Ctrl Pts',(-40.4196843207932,36.3555214006416,37.2538819813845));
#24615=CARTESIAN_POINT('Ctrl Pts',(-40.4450815241101,36.3700924122414,37.2856702479001));
#24616=CARTESIAN_POINT('Ctrl Pts',(-40.4703375347057,36.3851873092645,37.3173210693114));
#24617=CARTESIAN_POINT('Ctrl Pts',(-40.4955935453012,36.4002822062877,37.3489718907226));
#24618=CARTESIAN_POINT('Ctrl Pts',(-40.5207083627977,36.415900988508,37.3804852665568));
#24619=CARTESIAN_POINT('Ctrl Pts',(-40.5456735746448,36.4320384129698,37.4118506384062));
#24620=CARTESIAN_POINT('Ctrl Pts',(-40.570638786492,36.4481758374317,37.4432160102556));
#24621=CARTESIAN_POINT('Ctrl Pts',(-40.5954543923197,36.4648319038938,37.4744333776537));
#24622=CARTESIAN_POINT('Ctrl Pts',(-40.62011207985,36.4820010226548,37.5054922813855));
#24623=CARTESIAN_POINT('Ctrl Pts',(-40.6447697673802,36.4991701414158,37.5365511851173));
#24624=CARTESIAN_POINT('Ctrl Pts',(-40.6692695362319,36.5168523122129,37.5674516247135));
#24625=CARTESIAN_POINT('Ctrl Pts',(-40.6936031798588,36.5350416022997,37.5981832470913));
#24626=CARTESIAN_POINT('Ctrl Pts',(-40.7179368234858,36.5532308923865,37.6289148694691));
#24627=CARTESIAN_POINT('Ctrl Pts',(-40.7421043415256,36.571927301491,37.6594776741706));
#24628=CARTESIAN_POINT('Ctrl Pts',(-40.7660976386655,36.5911245577982,37.6898614211653));
#24629=CARTESIAN_POINT('Ctrl Pts',(-40.7900909358055,36.6103218141056,37.7202451681601));
#24630=CARTESIAN_POINT('Ctrl Pts',(-40.8139100116979,36.630019917334,37.7504498569997));
#24631=CARTESIAN_POINT('Ctrl Pts',(-40.8375468876434,36.6502122607802,37.7804653675298));
#24632=CARTESIAN_POINT('Ctrl Pts',(-40.8611837635889,36.6704046042263,37.8104808780598));
#24633=CARTESIAN_POINT('Ctrl Pts',(-40.8846384392368,36.6910911875891,37.8403072098336));
#24634=CARTESIAN_POINT('Ctrl Pts',(-40.9079030578806,36.7122650737206,37.8699343693509));
#24635=CARTESIAN_POINT('Ctrl Pts',(-40.9311676765242,36.7334389598521,37.8995615288682));
#24636=CARTESIAN_POINT('Ctrl Pts',(-40.9542422378081,36.7551001484313,37.9289895156833));
#24637=CARTESIAN_POINT('Ctrl Pts',(-40.9771190122039,36.7772413764693,37.9582084695932));
#24638=CARTESIAN_POINT('Ctrl Pts',(-40.9999957865997,36.7993826045072,37.9874274235032));
#24639=CARTESIAN_POINT('Ctrl Pts',(-41.0226747737666,36.8220038716734,38.0164373440725));
#24640=CARTESIAN_POINT('Ctrl Pts',(-41.0451483765286,36.8450975939977,38.0452285109826));
#24641=CARTESIAN_POINT('Ctrl Pts',(-41.0676219792906,36.8681913163219,38.0740196778928));
#24642=CARTESIAN_POINT('Ctrl Pts',(-41.0898901973128,36.8917574934596,38.1025920907146));
#24643=CARTESIAN_POINT('Ctrl Pts',(-41.1119455708393,36.915788225523,38.1309361755002));
#24644=CARTESIAN_POINT('Ctrl Pts',(-41.1340009443657,36.9398189575865,38.1592802602858));
#24645=CARTESIAN_POINT('Ctrl Pts',(-41.1558434730678,36.9643142442173,38.1873960166126));
#24646=CARTESIAN_POINT('Ctrl Pts',(-41.177465839586,36.9892658748842,38.2152740232916));
#24647=CARTESIAN_POINT('Ctrl Pts',(-41.1990882061042,37.0142175055512,38.2431520299707));
#24648=CARTESIAN_POINT('Ctrl Pts',(-41.2204904101162,37.0396254798822,38.2707922865863));
#24649=CARTESIAN_POINT('Ctrl Pts',(-41.2416652815407,37.0654812821836,38.2981855309956));
#24650=CARTESIAN_POINT('Ctrl Pts',(-41.2628401529652,37.0913370844849,38.3255787754048));
#24651=CARTESIAN_POINT('Ctrl Pts',(-41.2837876914865,37.1176407143712,38.352725007199));
#24652=CARTESIAN_POINT('Ctrl Pts',(-41.3045008790847,37.1443833566698,38.379615129462));
#24653=CARTESIAN_POINT('Ctrl Pts',(-41.3252140666829,37.1711259989686,38.406505251725));
#24654=CARTESIAN_POINT('Ctrl Pts',(-41.3456929030499,37.1983076532818,38.4331392640561));
#24655=CARTESIAN_POINT('Ctrl Pts',(-41.3659305269077,37.2259192108402,38.4595082408353));
#24656=CARTESIAN_POINT('Ctrl Pts',(-40.1775226142824,36.2455460982534,36.9999832962673));
#24657=CARTESIAN_POINT('Ctrl Pts',(-40.2045330088359,36.2572679658112,37.0334615519984));
#24658=CARTESIAN_POINT('Ctrl Pts',(-40.2314256153529,36.2695647115615,37.0668335548053));
#24659=CARTESIAN_POINT('Ctrl Pts',(-40.2581908128651,36.2824319360754,37.1000873656423));
#24660=CARTESIAN_POINT('Ctrl Pts',(-40.2849322441245,36.2952877350911,37.1333116486391));
#24661=CARTESIAN_POINT('Ctrl Pts',(-40.3115464920889,36.3087129999843,37.1664179489049));
#24662=CARTESIAN_POINT('Ctrl Pts',(-40.3380240521681,36.3227029362742,37.1993944434065));
#24663=CARTESIAN_POINT('Ctrl Pts',(-40.3645016122471,36.3366928725642,37.2323709379081));
#24664=CARTESIAN_POINT('Ctrl Pts',(-40.3908424839922,36.351247480013,37.2652176260855));
#24665=CARTESIAN_POINT('Ctrl Pts',(-40.4170372605052,36.3663615608482,37.2979227776481));
#24666=CARTESIAN_POINT('Ctrl Pts',(-40.4432320370181,36.3814756416834,37.3306279292107));
#24667=CARTESIAN_POINT('Ctrl Pts',(-40.4692807178519,36.3971491956478,37.3631915436014));
#24668=CARTESIAN_POINT('Ctrl Pts',(-40.495174000398,36.4133766253454,37.3956019915952));
#24669=CARTESIAN_POINT('Ctrl Pts',(-40.5210672829441,36.4296040550429,37.4280124395889));
#24670=CARTESIAN_POINT('Ctrl Pts',(-40.5468051667636,36.4463853601978,37.4602697206352));
#24671=CARTESIAN_POINT('Ctrl Pts',(-40.5723784602946,36.4637145478324,37.4923623149318));
#24672=CARTESIAN_POINT('Ctrl Pts',(-40.5979517538256,36.481043735467,37.5244549092285));
#24673=CARTESIAN_POINT('Ctrl Pts',(-40.62336045662,36.4989208052812,37.5563828162238));
#24674=CARTESIAN_POINT('Ctrl Pts',(-40.6485954946484,36.517339372964,37.588134633731));
#24675=CARTESIAN_POINT('Ctrl Pts',(-40.6738305326767,36.5357579406467,37.6198864512383));
#24676=CARTESIAN_POINT('Ctrl Pts',(-40.6988919055097,36.5547180058848,37.6514621787174));
#24677=CARTESIAN_POINT('Ctrl Pts',(-40.7237706631572,36.5742127976047,37.682850539753));
#24678=CARTESIAN_POINT('Ctrl Pts',(-40.7486494208046,36.5937075893247,37.7142389007886));
#24679=CARTESIAN_POINT('Ctrl Pts',(-40.7733455628527,36.6137371071996,37.7454398948509));
#24680=CARTESIAN_POINT('Ctrl Pts',(-40.7978502697247,36.6342941982205,37.7764423793422));
#24681=CARTESIAN_POINT('Ctrl Pts',(-40.8223549765967,36.6548512892413,37.8074448638336));
#24682=CARTESIAN_POINT('Ctrl Pts',(-40.8466682478773,36.6759359530588,37.8382488382272));
#24683=CARTESIAN_POINT('Ctrl Pts',(-40.8707814007572,36.6975406598657,37.8688433017258));
#24684=CARTESIAN_POINT('Ctrl Pts',(-40.8948945536371,36.7191453666726,37.8994377652244));
#24685=CARTESIAN_POINT('Ctrl Pts',(-40.9188075876976,36.741270116097,37.9298227173039));
#24686=CARTESIAN_POINT('Ctrl Pts',(-40.9425119630467,36.763907006884,37.9599873068021));
#24687=CARTESIAN_POINT('Ctrl Pts',(-40.9662163383959,36.7865438976709,37.9901518963003));
#24688=CARTESIAN_POINT('Ctrl Pts',(-40.9897120546304,36.8096929294357,38.0200961227041));
#24689=CARTESIAN_POINT('Ctrl Pts',(-41.0129907208921,36.8333458351287,38.0498092922445));
#24690=CARTESIAN_POINT('Ctrl Pts',(-41.0362693871538,36.8569987408218,38.079522461785));
#24691=CARTESIAN_POINT('Ctrl Pts',(-41.0593310030467,36.8811555200408,38.1090045739568));
#24692=CARTESIAN_POINT('Ctrl Pts',(-41.0821673327396,36.905807545847,38.1382451000225));
#24693=CARTESIAN_POINT('Ctrl Pts',(-41.1050036624325,36.9304595716531,38.1674856260882));
#24694=CARTESIAN_POINT('Ctrl Pts',(-41.1276147055371,36.955606843627,38.1964845655505));
#24695=CARTESIAN_POINT('Ctrl Pts',(-41.149992387132,36.9812403811018,38.2252315622241));
#24696=CARTESIAN_POINT('Ctrl Pts',(-41.1723700687269,37.0068739185767,38.2539785588976));
#24697=CARTESIAN_POINT('Ctrl Pts',(-41.1945143884316,37.0329937211167,38.2824736122934));
#24698=CARTESIAN_POINT('Ctrl Pts',(-41.2164174380024,37.059590460742,38.3107065461755));
#24699=CARTESIAN_POINT('Ctrl Pts',(-41.2383204875732,37.0861872003675,38.3389394800575));
#24700=CARTESIAN_POINT('Ctrl Pts',(-41.2599822666375,37.1132608766259,38.3669102939456));
#24701=CARTESIAN_POINT('Ctrl Pts',(-41.2813950392781,37.1408018208876,38.3946089988215));
#24702=CARTESIAN_POINT('Ctrl Pts',(-41.3028078119186,37.1683427651494,38.4223077036974));
#24703=CARTESIAN_POINT('Ctrl Pts',(-41.3239715777718,37.1963509769467,38.4497342990905));
#24704=CARTESIAN_POINT('Ctrl Pts',(-41.3448787787706,37.2248164539041,38.4768789903345));
#24705=CARTESIAN_POINT('Ctrl Pts',(-40.115662892394,36.2275168856964,36.9710119355355));
#24706=CARTESIAN_POINT('Ctrl Pts',(-40.1436341839173,36.2390416726869,37.0055602663057));
#24707=CARTESIAN_POINT('Ctrl Pts',(-40.1714855064378,36.2511777563766,37.0400015134906));
#24708=CARTESIAN_POINT('Ctrl Pts',(-40.1992063203907,36.2639205315914,37.0743226412208));
#24709=CARTESIAN_POINT('Ctrl Pts',(-40.2269025195477,36.2766519918134,37.108613293383));
#24710=CARTESIAN_POINT('Ctrl Pts',(-40.2544684412783,36.2899890663684,37.1427840386652));
#24711=CARTESIAN_POINT('Ctrl Pts',(-40.2818936724897,36.3039267054276,37.1768219665485));
#24712=CARTESIAN_POINT('Ctrl Pts',(-40.3093189037011,36.3178643444868,37.2108598944317));
#24713=CARTESIAN_POINT('Ctrl Pts',(-40.3366034438743,36.3324025477847,37.2447650042708));
#24714=CARTESIAN_POINT('Ctrl Pts',(-40.3637369863047,36.3475358124319,37.2785244859848));
#24715=CARTESIAN_POINT('Ctrl Pts',(-40.390870528735,36.3626690770792,37.3122839676987));
#24716=CARTESIAN_POINT('Ctrl Pts',(-40.4178530729061,36.3783974027877,37.3458978206461));
#24717=CARTESIAN_POINT('Ctrl Pts',(-40.4446744261511,36.3947148377209,37.3793533447841));
#24718=CARTESIAN_POINT('Ctrl Pts',(-40.4714957793961,36.4110322726542,37.4128088689221));
#24719=CARTESIAN_POINT('Ctrl Pts',(-40.4981559412074,36.4279388165018,37.4461060636166));
#24720=CARTESIAN_POINT('Ctrl Pts',(-40.5246448407391,36.44542807301,37.4792323484781));
#24721=CARTESIAN_POINT('Ctrl Pts',(-40.5511337402709,36.4629173295182,37.5123586333397));
#24722=CARTESIAN_POINT('Ctrl Pts',(-40.5774513770083,36.4809892983495,37.5453140077341));
#24723=CARTESIAN_POINT('Ctrl Pts',(-40.603587809438,36.4996371436282,37.5780860203707));
#24724=CARTESIAN_POINT('Ctrl Pts',(-40.6297242418677,36.518284988907,37.6108580330073));
#24725=CARTESIAN_POINT('Ctrl Pts',(-40.6556794694938,36.5375087102787,37.6434466832641));
#24726=CARTESIAN_POINT('Ctrl Pts',(-40.6814436876488,36.5573010374112,37.6758396583406));
#24727=CARTESIAN_POINT('Ctrl Pts',(-40.7072079058038,36.5770933645438,37.7082326334171));
#24728=CARTESIAN_POINT('Ctrl Pts',(-40.7327811140074,36.5974542970652,37.7404299327021));
#24729=CARTESIAN_POINT('Ctrl Pts',(-40.7581536518059,36.6183761356608,37.7724193911547));
#24730=CARTESIAN_POINT('Ctrl Pts',(-40.7835261896044,36.6392979742563,37.8044088496072));
#24731=CARTESIAN_POINT('Ctrl Pts',(-40.8086980565178,36.6607807185286,37.8361904666208));
#24732=CARTESIAN_POINT('Ctrl Pts',(-40.8336597436339,36.6828162460109,37.8677522341008));
#24733=CARTESIAN_POINT('Ctrl Pts',(-40.8586214307499,36.7048517734931,37.8993140015807));
#24734=CARTESIAN_POINT('Ctrl Pts',(-40.8833729375871,36.7274400837625,37.9306559189246));
#24735=CARTESIAN_POINT('Ctrl Pts',(-40.9079049138896,36.7505726372986,37.961766144011));
#24736=CARTESIAN_POINT('Ctrl Pts',(-40.9324368901921,36.7737051908346,37.9928763690974));
#24737=CARTESIAN_POINT('Ctrl Pts',(-40.9567493354943,36.7973819871978,38.0237549013357));
#24738=CARTESIAN_POINT('Ctrl Pts',(-40.9808330652556,36.8215940762597,38.0543900735065));
#24739=CARTESIAN_POINT('Ctrl Pts',(-41.004916795017,36.8458061653216,38.0850252456773));
#24740=CARTESIAN_POINT('Ctrl Pts',(-41.0287718087805,36.8705535466221,38.115417057199));
#24741=CARTESIAN_POINT('Ctrl Pts',(-41.0523890946399,36.8958268661709,38.1455540245448));
#24742=CARTESIAN_POINT('Ctrl Pts',(-41.0760063804993,36.9211001857197,38.1756909918906));
#24743=CARTESIAN_POINT('Ctrl Pts',(-41.0993859380063,36.9468994430366,38.2055731144884));
#24744=CARTESIAN_POINT('Ctrl Pts',(-41.122518934678,36.9732148873195,38.2351891011565));
#24745=CARTESIAN_POINT('Ctrl Pts',(-41.1456519313497,36.9995303316023,38.2648050878245));
#24746=CARTESIAN_POINT('Ctrl Pts',(-41.168538366747,37.0263619623512,38.2941549380004));
#24747=CARTESIAN_POINT('Ctrl Pts',(-41.1911695944641,37.0536996393006,38.3232275613553));
#24748=CARTESIAN_POINT('Ctrl Pts',(-41.2138008221812,37.0810373162499,38.3523001847102));
#24749=CARTESIAN_POINT('Ctrl Pts',(-41.2361768417885,37.1088810388806,38.3810955806921));
#24750=CARTESIAN_POINT('Ctrl Pts',(-41.2582891994715,37.1372202851054,38.4096028681809));
#24751=CARTESIAN_POINT('Ctrl Pts',(-41.2804015571544,37.1655595313302,38.4381101556698));
#24752=CARTESIAN_POINT('Ctrl Pts',(-41.3022502524937,37.1943943006115,38.4663293341249));
#24753=CARTESIAN_POINT('Ctrl Pts',(-41.3238270306336,37.223713696968,38.4942497398337));
#24754=CARTESIAN_POINT('Ctrl Pts',(-40.0552080328795,36.2113706699628,36.9436917252841));
#24755=CARTESIAN_POINT('Ctrl Pts',(-40.0841050153821,36.2226541801109,36.9792689639886));
#24756=CARTESIAN_POINT('Ctrl Pts',(-40.1128805203379,36.2345857171285,37.0147390538272));
#24757=CARTESIAN_POINT('Ctrl Pts',(-40.1415230375772,36.2471604949643,37.0500878044519));
#24758=CARTESIAN_POINT('Ctrl Pts',(-40.1701401215908,36.2597241069812,37.0854051670272));
#24759=CARTESIAN_POINT('Ctrl Pts',(-40.1986244533505,36.27292981772,37.1206014050315));
#24760=CARTESIAN_POINT('Ctrl Pts',(-40.2269646594312,36.286772341823,37.1556624627514));
#24761=CARTESIAN_POINT('Ctrl Pts',(-40.255304865512,36.300614865926,37.1907235204712));
#24762=CARTESIAN_POINT('Ctrl Pts',(-40.2835009453131,36.3150942030985,37.2256493971632));
#24763=CARTESIAN_POINT('Ctrl Pts',(-40.3115416405743,36.3302045601569,37.2604261451727));
#24764=CARTESIAN_POINT('Ctrl Pts',(-40.3395823358355,36.3453149172154,37.2952028931822));
#24765=CARTESIAN_POINT('Ctrl Pts',(-40.3674676459623,36.3610562938383,37.3298305117718));
#24766=CARTESIAN_POINT('Ctrl Pts',(-40.3951864368229,36.3774223936394,37.3642951724522));
#24767=CARTESIAN_POINT('Ctrl Pts',(-40.4229052276836,36.3937884934405,37.3987598331327));
#24768=CARTESIAN_POINT('Ctrl Pts',(-40.4504574986905,36.4107793160717,37.4330615351731));
#24769=CARTESIAN_POINT('Ctrl Pts',(-40.4778322487034,36.4283880669659,37.4671865802606));
#24770=CARTESIAN_POINT('Ctrl Pts',(-40.5052069987162,36.4459968178601,37.501311625348));
#24771=CARTESIAN_POINT('Ctrl Pts',(-40.5324042271549,36.4642234966432,37.5352600127589));
#24772=CARTESIAN_POINT('Ctrl Pts',(-40.55941307463,36.4830608159865,37.5690181852644));
#24773=CARTESIAN_POINT('Ctrl Pts',(-40.5864219221051,36.5018981353298,37.6027763577698));
#24774=CARTESIAN_POINT('Ctrl Pts',(-40.6132423880441,36.5213460948331,37.636344314654));
#24775=CARTESIAN_POINT('Ctrl Pts',(-40.6398637634536,36.5413969202162,37.6697086505675));
#24776=CARTESIAN_POINT('Ctrl Pts',(-40.6664851388631,36.5614477455992,37.703072986481));
#24777=CARTESIAN_POINT('Ctrl Pts',(-40.6929074231786,36.5821014364361,37.7362337007163));
#24778=CARTESIAN_POINT('Ctrl Pts',(-40.7191200663288,36.603349737693,37.7691775504777));
#24779=CARTESIAN_POINT('Ctrl Pts',(-40.745332709479,36.6245980389499,37.8021214002391));
#24780=CARTESIAN_POINT('Ctrl Pts',(-40.7713357109083,36.6464409501754,37.8348483848281));
#24781=CARTESIAN_POINT('Ctrl Pts',(-40.7971186878659,36.6688697421607,37.8673454345476));
#24782=CARTESIAN_POINT('Ctrl Pts',(-40.8229016648234,36.691298534146,37.899842484267));
#24783=CARTESIAN_POINT('Ctrl Pts',(-40.8484646167628,36.7143132064151,37.932109598428));
#24784=CARTESIAN_POINT('Ctrl Pts',(-40.8737973365208,36.7379045625412,37.9641338908396));
#24785=CARTESIAN_POINT('Ctrl Pts',(-40.8991300562788,36.7614959186673,37.9961581832512));
#24786=CARTESIAN_POINT('Ctrl Pts',(-40.9242325433185,36.7856639581496,38.0279396532343));
#24787=CARTESIAN_POINT('Ctrl Pts',(-40.9490947741904,36.8103990246712,38.0594656083655));
#24788=CARTESIAN_POINT('Ctrl Pts',(-40.9739570050623,36.8351340911929,38.0909915634966));
#24789=CARTESIAN_POINT('Ctrl Pts',(-40.9985789792395,36.8604361842288,38.1222620031072));
#24790=CARTESIAN_POINT('Ctrl Pts',(-41.0229508649667,36.8862951952653,38.1532644386485));
#24791=CARTESIAN_POINT('Ctrl Pts',(-41.0473227506939,36.9121542063018,38.1842668741896));
#24792=CARTESIAN_POINT('Ctrl Pts',(-41.0714445474545,36.9385701347902,38.215001305004));
#24793=CARTESIAN_POINT('Ctrl Pts',(-41.0953066230155,36.9655324280727,38.2454554563619));
#24794=CARTESIAN_POINT('Ctrl Pts',(-41.1191686985763,36.9924947213551,38.2759096077198));
#24795=CARTESIAN_POINT('Ctrl Pts',(-41.1427710524317,37.0200033788596,38.3060834789756));
#24796=CARTESIAN_POINT('Ctrl Pts',(-41.1661042595398,37.0480474121905,38.3359650189942));
#24797=CARTESIAN_POINT('Ctrl Pts',(-41.1894374666479,37.0760914455213,38.3658465590128));
#24798=CARTESIAN_POINT('Ctrl Pts',(-41.2125015265139,37.1046708540836,38.3954357671606));
#24799=CARTESIAN_POINT('Ctrl Pts',(-41.2352872287921,37.1337742224959,38.4247208254941));
#24800=CARTESIAN_POINT('Ctrl Pts',(-41.2580729310703,37.1628775909081,38.4540058838276));
#24801=CARTESIAN_POINT('Ctrl Pts',(-41.2805802752775,37.192504918553,38.4829867917259));
#24802=CARTESIAN_POINT('Ctrl Pts',(-41.3028002730974,37.2226443721554,38.5116519738488));
#24803=CARTESIAN_POINT('Ctrl Pts',(-39.995899860225,36.196737685331,36.9177032409763));
#24804=CARTESIAN_POINT('Ctrl Pts',(-40.0256928412121,36.2077442217939,36.9542750213889));
#24805=CARTESIAN_POINT('Ctrl Pts',(-40.0553634771827,36.2194357452618,36.9907403169737));
#24806=CARTESIAN_POINT('Ctrl Pts',(-40.0848992390629,36.2318073184586,37.0270837294477));
#24807=CARTESIAN_POINT('Ctrl Pts',(-40.1144087745578,36.2441679062727,37.0633948706585));
#24808=CARTESIAN_POINT('Ctrl Pts',(-40.1437836746807,36.257207336354,37.0995843442551));
#24809=CARTESIAN_POINT('Ctrl Pts',(-40.1730115572085,36.2709201122706,37.1356368955084));
#24810=CARTESIAN_POINT('Ctrl Pts',(-40.2022394397364,36.2846328881872,37.1716894467616));
#24811=CARTESIAN_POINT('Ctrl Pts',(-40.2313203039765,36.2990190096142,37.2076050748172));
#24812=CARTESIAN_POINT('Ctrl Pts',(-40.2602418916486,36.3140724124571,37.2433686403783));
#24813=CARTESIAN_POINT('Ctrl Pts',(-40.2891634793206,36.3291258153,37.2791322059394));
#24814=CARTESIAN_POINT('Ctrl Pts',(-40.3179257897392,36.3448464992021,37.3147437081585));
#24815=CARTESIAN_POINT('Ctrl Pts',(-40.3465166989024,36.361227837519,37.3501881359354));
#24816=CARTESIAN_POINT('Ctrl Pts',(-40.3751076080657,36.3776091758358,37.3856325637123));
#24817=CARTESIAN_POINT('Ctrl Pts',(-40.4035271152963,36.3946511681793,37.4209099162071));
#24818=CARTESIAN_POINT('Ctrl Pts',(-40.4317632410912,36.4123466309417,37.4560053231714));
#24819=CARTESIAN_POINT('Ctrl Pts',(-40.4599993668862,36.430042093704,37.4911007301356));
#24820=CARTESIAN_POINT('Ctrl Pts',(-40.4880521105766,36.4483910264661,37.5260141907377));
#24821=CARTESIAN_POINT('Ctrl Pts',(-40.5159096472599,36.4673856947134,37.5607309881186));
#24822=CARTESIAN_POINT('Ctrl Pts',(-40.5437671839431,36.4863803629608,37.5954477854994));
#24823=CARTESIAN_POINT('Ctrl Pts',(-40.5714295129589,36.5060207662435,37.6299679188363));
#24824=CARTESIAN_POINT('Ctrl Pts',(-40.5988849739737,36.5262986256614,37.664276837067));
#24825=CARTESIAN_POINT('Ctrl Pts',(-40.6263404349885,36.5465764850793,37.6985857552976));
#24826=CARTESIAN_POINT('Ctrl Pts',(-40.6535890273516,36.567491800152,37.732683457609));
#24827=CARTESIAN_POINT('Ctrl Pts',(-40.6806192651293,36.5890357545737,37.7665555710037));
#24828=CARTESIAN_POINT('Ctrl Pts',(-40.7076495029071,36.6105797089953,37.8004276843984));
#24829=CARTESIAN_POINT('Ctrl Pts',(-40.7344613854591,36.6327523022554,37.8340742080738));
#24830=CARTESIAN_POINT('Ctrl Pts',(-40.7610436109349,36.6555441880753,37.8674809592147));
#24831=CARTESIAN_POINT('Ctrl Pts',(-40.7876258364107,36.6783360738951,37.9008877103557));
#24832=CARTESIAN_POINT('Ctrl Pts',(-40.8139784041806,36.7017472517346,37.9340546881708));
#24833=CARTESIAN_POINT('Ctrl Pts',(-40.8400902060065,36.7257678532221,37.9669679119851));
#24834=CARTESIAN_POINT('Ctrl Pts',(-40.8662020078325,36.7497884547095,37.9998811357994));
#24835=CARTESIAN_POINT('Ctrl Pts',(-40.8920730430959,36.7744184792757,38.032540604833));
#24836=CARTESIAN_POINT('Ctrl Pts',(-40.917692406536,36.799647544776,38.0649325523381));
#24837=CARTESIAN_POINT('Ctrl Pts',(-40.9433117699762,36.8248766102762,38.0973244998432));
#24838=CARTESIAN_POINT('Ctrl Pts',(-40.9686794609861,36.8507047161126,38.1294489250522));
#24839=CARTESIAN_POINT('Ctrl Pts',(-40.993784786477,36.8771209751204,38.1612922867512));
#24840=CARTESIAN_POINT('Ctrl Pts',(-41.018890111968,36.9035372341282,38.1931356484502));
#24841=CARTESIAN_POINT('Ctrl Pts',(-41.043733071345,36.9305416456815,38.2246979458846));
#24842=CARTESIAN_POINT('Ctrl Pts',(-41.0683031927061,36.9581228267747,38.2559658747907));
#24843=CARTESIAN_POINT('Ctrl Pts',(-41.0928733140672,36.9857040078678,38.2872338036968));
#24844=CARTESIAN_POINT('Ctrl Pts',(-41.1171705968302,37.0138619578471,38.3182073633337));
#24845=CARTESIAN_POINT('Ctrl Pts',(-41.1411847991091,37.0425848074629,38.3488734976047));
#24846=CARTESIAN_POINT('Ctrl Pts',(-41.1651990013879,37.0713076570786,38.3795396318758));
#24847=CARTESIAN_POINT('Ctrl Pts',(-41.1889301226135,37.1005954056502,38.4098983400543));
#24848=CARTESIAN_POINT('Ctrl Pts',(-41.2123681595503,37.1304357076907,38.4399368252183));
#24849=CARTESIAN_POINT('Ctrl Pts',(-41.2358061964872,37.1602760097311,38.4699753103823));
#24850=CARTESIAN_POINT('Ctrl Pts',(-41.2589511485798,37.1906688645334,38.49969357182));
#24851=CARTESIAN_POINT('Ctrl Pts',(-41.2817932596771,37.2216014607819,38.529079082573));
#24852=CARTESIAN_POINT('Ctrl Pts',(-39.9365916875705,36.1821047006991,36.8917147566685));
#24853=CARTESIAN_POINT('Ctrl Pts',(-39.9672806670422,36.192834263477,36.9292810787893));
#24854=CARTESIAN_POINT('Ctrl Pts',(-39.9978464340274,36.2042857733951,36.9667415801203));
#24855=CARTESIAN_POINT('Ctrl Pts',(-40.0282754405486,36.2164541419529,37.0040796544433));
#24856=CARTESIAN_POINT('Ctrl Pts',(-40.0586774275246,36.2286117055642,37.0413845742898));
#24857=CARTESIAN_POINT('Ctrl Pts',(-40.0889428960108,36.241484854988,37.0785672834787));
#24858=CARTESIAN_POINT('Ctrl Pts',(-40.1190584549858,36.2550678827182,37.1156113282653));
#24859=CARTESIAN_POINT('Ctrl Pts',(-40.1491740139607,36.2686509104485,37.152655373052));
#24860=CARTESIAN_POINT('Ctrl Pts',(-40.1791396626399,36.28294381613,37.1895607524711));
#24861=CARTESIAN_POINT('Ctrl Pts',(-40.2089421427228,36.2979402647574,37.2263111355838));
#24862=CARTESIAN_POINT('Ctrl Pts',(-40.2387446228058,36.3129367133846,37.2630615186965));
#24863=CARTESIAN_POINT('Ctrl Pts',(-40.268383933516,36.3286367045658,37.2996569045451));
#24864=CARTESIAN_POINT('Ctrl Pts',(-40.297846960982,36.3450332813984,37.3360810994186));
#24865=CARTESIAN_POINT('Ctrl Pts',(-40.3273099884479,36.3614298582311,37.372505294292));
#24866=CARTESIAN_POINT('Ctrl Pts',(-40.356596731902,36.3785230202869,37.4087582972411));
#24867=CARTESIAN_POINT('Ctrl Pts',(-40.3856942334791,36.3963051949174,37.4448240660821));
#24868=CARTESIAN_POINT('Ctrl Pts',(-40.4147917350561,36.4140873695479,37.4808898349232));
#24869=CARTESIAN_POINT('Ctrl Pts',(-40.4436999939984,36.4325585562889,37.5167683687165));
#24870=CARTESIAN_POINT('Ctrl Pts',(-40.4724062198898,36.4517105734403,37.5524437909728));
#24871=CARTESIAN_POINT('Ctrl Pts',(-40.5011124457811,36.4708625905918,37.588119213229));
#24872=CARTESIAN_POINT('Ctrl Pts',(-40.5296166378738,36.4906954376539,37.6235915230185));
#24873=CARTESIAN_POINT('Ctrl Pts',(-40.5579061844939,36.5112003311067,37.6588450235664));
#24874=CARTESIAN_POINT('Ctrl Pts',(-40.586195731114,36.5317052245595,37.6940985241142));
#24875=CARTESIAN_POINT('Ctrl Pts',(-40.6142706315245,36.5528821638678,37.7291332145017));
#24876=CARTESIAN_POINT('Ctrl Pts',(-40.6421184639298,36.5747217714543,37.7639335915297));
#24877=CARTESIAN_POINT('Ctrl Pts',(-40.6699662963352,36.5965613790407,37.7987339685576));
#24878=CARTESIAN_POINT('Ctrl Pts',(-40.6975870600099,36.6190636543355,37.8333000313194));
#24879=CARTESIAN_POINT('Ctrl Pts',(-40.724968534004,36.6422186339898,37.8676164838819));
#24880=CARTESIAN_POINT('Ctrl Pts',(-40.7523500079981,36.6653736136441,37.9019329364444));
#24881=CARTESIAN_POINT('Ctrl Pts',(-40.7794921915984,36.6891812970541,37.9359997779136));
#24882=CARTESIAN_POINT('Ctrl Pts',(-40.8063830754924,36.7136311439029,37.9698019331306));
#24883=CARTESIAN_POINT('Ctrl Pts',(-40.8332739593863,36.7380809907517,38.0036040883476));
#24884=CARTESIAN_POINT('Ctrl Pts',(-40.8599135428732,36.7631730004019,38.0371415564316));
#24885=CARTESIAN_POINT('Ctrl Pts',(-40.8862900388817,36.7888960648807,38.0703994963107));
#24886=CARTESIAN_POINT('Ctrl Pts',(-40.9126665348901,36.8146191293595,38.1036574361897));
#24887=CARTESIAN_POINT('Ctrl Pts',(-40.9387799427328,36.8409732479963,38.1366358469971));
#24888=CARTESIAN_POINT('Ctrl Pts',(-40.9646187079874,36.8679467549755,38.169320134854));
#24889=CARTESIAN_POINT('Ctrl Pts',(-40.990457473242,36.8949202619546,38.2020044227108));
#24890=CARTESIAN_POINT('Ctrl Pts',(-41.0160215952354,36.922513156573,38.2343945867653));
#24891=CARTESIAN_POINT('Ctrl Pts',(-41.0412997623967,36.9507132254767,38.2664762932196));
#24892=CARTESIAN_POINT('Ctrl Pts',(-41.066577929558,36.9789132943805,38.2985579996738));
#24893=CARTESIAN_POINT('Ctrl Pts',(-41.0915701412288,37.0077205368345,38.3303312476919));
#24894=CARTESIAN_POINT('Ctrl Pts',(-41.1162653386783,37.0371222027352,38.3617819762153));
#24895=CARTESIAN_POINT('Ctrl Pts',(-41.140960536128,37.0665238686359,38.3932327047388));
#24896=CARTESIAN_POINT('Ctrl Pts',(-41.1653587187131,37.0965199572167,38.4243609129481));
#24897=CARTESIAN_POINT('Ctrl Pts',(-41.1894490903085,37.1270971928855,38.4551528249425));
#24898=CARTESIAN_POINT('Ctrl Pts',(-41.2135394619039,37.1576744285542,38.485944736937));
#24899=CARTESIAN_POINT('Ctrl Pts',(-41.2373220218821,37.1888328105138,38.5164003519141));
#24900=CARTESIAN_POINT('Ctrl Pts',(-41.2607862462568,37.2205585494085,38.5465061912972));
#24901=CARTESIAN_POINT('Ctrl Pts',(-39.8784322174862,36.1689883085647,36.8670608120083));
#24902=CARTESIAN_POINT('Ctrl Pts',(-39.9099874630055,36.1794051227783,36.9055872530872));
#24903=CARTESIAN_POINT('Ctrl Pts',(-39.9414192696731,36.1905810749234,36.9440092667769));
#24904=CARTESIAN_POINT('Ctrl Pts',(-39.9727130222373,36.2025109548909,36.9823089854244));
#24905=CARTESIAN_POINT('Ctrl Pts',(-40.003978987402,36.2144302416788,37.0205746956998));
#24906=CARTESIAN_POINT('Ctrl Pts',(-40.0351071426304,36.2271021176342,37.0587183269245));
#24907=CARTESIAN_POINT('Ctrl Pts',(-40.0660830396764,36.2405206886271,37.0967221725232));
#24908=CARTESIAN_POINT('Ctrl Pts',(-40.0970589367223,36.25393925962,37.1347260181219));
#24909=CARTESIAN_POINT('Ctrl Pts',(-40.1278825746968,36.2681045252642,37.1725900770043));
#24910=CARTESIAN_POINT('Ctrl Pts',(-40.1585396467511,36.2830098989899,37.2102967724828));
#24911=CARTESIAN_POINT('Ctrl Pts',(-40.1891967188056,36.2979152727155,37.2480034679613));
#24912=CARTESIAN_POINT('Ctrl Pts',(-40.2196872240624,36.3135607540937,37.2855527989552));
#24913=CARTESIAN_POINT('Ctrl Pts',(-40.2499970104069,36.3299390702522,37.3229273349807));
#24914=CARTESIAN_POINT('Ctrl Pts',(-40.2803067967514,36.3463173864108,37.3603018710062));
#24915=CARTESIAN_POINT('Ctrl Pts',(-40.3104358633138,36.3634285368788,37.3975016109911));
#24916=CARTESIAN_POINT('Ctrl Pts',(-40.340370225743,36.3812645692036,37.4345092867707));
#24917=CARTESIAN_POINT('Ctrl Pts',(-40.3703045881721,36.3991006015286,37.4715169625502));
#24918=CARTESIAN_POINT('Ctrl Pts',(-40.4000442456191,36.417661515201,37.5083325730667));
#24919=CARTESIAN_POINT('Ctrl Pts',(-40.4295753945039,36.4369386855833,37.5449390284921));
#24920=CARTESIAN_POINT('Ctrl Pts',(-40.4591065433887,36.4562158559656,37.5815454839174));
#24921=CARTESIAN_POINT('Ctrl Pts',(-40.4884291828649,36.4762092825039,37.617942783202));
#24922=CARTESIAN_POINT('Ctrl Pts',(-40.5175297028907,36.4969096763675,37.6541140306777));
#24923=CARTESIAN_POINT('Ctrl Pts',(-40.5466302229165,36.5176100702311,37.6902852781534));
#24924=CARTESIAN_POINT('Ctrl Pts',(-40.5755086226514,36.5390174308226,37.7262304727808));
#24925=CARTESIAN_POINT('Ctrl Pts',(-40.6041514982105,36.5611218137356,37.7619329287079));
#24926=CARTESIAN_POINT('Ctrl Pts',(-40.6327943737695,36.5832261966487,37.797635384635));
#24927=CARTESIAN_POINT('Ctrl Pts',(-40.6612017243305,36.6060276012486,37.8330951008377));
#24928=CARTESIAN_POINT('Ctrl Pts',(-40.6893603645431,36.6295154367558,37.8682956167224));
#24929=CARTESIAN_POINT('Ctrl Pts',(-40.7175190047557,36.6530032722632,37.9034961326072));
#24930=CARTESIAN_POINT('Ctrl Pts',(-40.7454289338183,36.6771775380065,37.9384374471669));
#24931=CARTESIAN_POINT('Ctrl Pts',(-40.7730771971629,36.7020270066669,37.9731033403279));
#24932=CARTESIAN_POINT('Ctrl Pts',(-40.8007254605076,36.7268764753273,38.0077692334889));
#24933=CARTESIAN_POINT('Ctrl Pts',(-40.8281120573416,36.7524011461916,38.0421597042572));
#24934=CARTESIAN_POINT('Ctrl Pts',(-40.855224275867,36.7785891658016,38.0762587881));
#24935=CARTESIAN_POINT('Ctrl Pts',(-40.8823364943923,36.8047771854116,38.1103578719428));
#24936=CARTESIAN_POINT('Ctrl Pts',(-40.9091743338317,36.8316285530159,38.1441655678822));
#24937=CARTESIAN_POINT('Ctrl Pts',(-40.935725336931,36.8591308000021,38.1776661817153));
#24938=CARTESIAN_POINT('Ctrl Pts',(-40.9622763400304,36.8866330469883,38.2111667955484));
#24939=CARTESIAN_POINT('Ctrl Pts',(-40.9885405060285,36.9147861725675,38.2443603263144));
#24940=CARTESIAN_POINT('Ctrl Pts',(-41.0145056437539,36.9435771045273,38.2772313646783));
#24941=CARTESIAN_POINT('Ctrl Pts',(-41.0404707814793,36.9723680364872,38.3101024030422));
#24942=CARTESIAN_POINT('Ctrl Pts',(-41.0661368901876,37.0017967740017,38.3426509480614));
#24943=CARTESIAN_POINT('Ctrl Pts',(-41.0914920560819,37.0318496533715,38.3748618895438));
#24944=CARTESIAN_POINT('Ctrl Pts',(-41.1168472219763,37.0619025327413,38.4070728310262));
#24945=CARTESIAN_POINT('Ctrl Pts',(-41.1418914443299,37.0925795531042,38.4389461680483));
#24946=CARTESIAN_POINT('Ctrl Pts',(-41.1666130977562,37.1238664719334,38.4704671035589));
#24947=CARTESIAN_POINT('Ctrl Pts',(-41.1913347511826,37.1551533907627,38.5019880390694));
#24948=CARTESIAN_POINT('Ctrl Pts',(-41.2157338349727,37.1870502071607,38.5331565721646));
#24949=CARTESIAN_POINT('Ctrl Pts',(-41.2397990229199,37.219542112969,38.5639582326428));
#24950=CARTESIAN_POINT('Ctrl Pts',(-39.8212339521721,36.1571263872747,36.843513753304));
#24951=CARTESIAN_POINT('Ctrl Pts',(-39.8536297885598,36.1672007132204,36.8829707943146));
#24952=CARTESIAN_POINT('Ctrl Pts',(-39.8859025733484,36.1780715372741,36.922325499607));
#24953=CARTESIAN_POINT('Ctrl Pts',(-39.9180365787514,36.1897335612995,36.9615586900972));
#24954=CARTESIAN_POINT('Ctrl Pts',(-39.9501420506494,36.201385229989,37.0007570433356));
#24955=CARTESIAN_POINT('Ctrl Pts',(-39.9821089884994,36.2138266938084,37.0398340962383));
#24956=CARTESIAN_POINT('Ctrl Pts',(-40.0139218412059,36.2270519003014,37.0787708388032));
#24957=CARTESIAN_POINT('Ctrl Pts',(-40.0457346939124,36.2402771067946,37.1177075813681));
#24958=CARTESIAN_POINT('Ctrl Pts',(-40.0773934604703,36.2542860555442,37.1565040123657));
#24959=CARTESIAN_POINT('Ctrl Pts',(-40.1088827396594,36.2690719315407,37.1951412582926));
#24960=CARTESIAN_POINT('Ctrl Pts',(-40.1403720188486,36.2838578075371,37.2337785042195));
#24961=CARTESIAN_POINT('Ctrl Pts',(-40.1716918096762,36.2994206103136,37.2722565638567));
#24962=CARTESIAN_POINT('Ctrl Pts',(-40.2028268758645,36.3157527689609,37.310556718596));
#24963=CARTESIAN_POINT('Ctrl Pts',(-40.2339619420527,36.3320849276083,37.3488568733352));
#24964=CARTESIAN_POINT('Ctrl Pts',(-40.2649122826178,36.349186441611,37.386979121967));
#24965=CARTESIAN_POINT('Ctrl Pts',(-40.2956628409744,36.3670489915034,37.4249049189625));
#24966=CARTESIAN_POINT('Ctrl Pts',(-40.3264133993311,36.3849115413958,37.462830715958));
#24967=CARTESIAN_POINT('Ctrl Pts',(-40.3569641745175,36.4035351266172,37.5005600601234));
#24968=CARTESIAN_POINT('Ctrl Pts',(-40.387300304344,36.422910687258,37.5380745970745));
#24969=CARTESIAN_POINT('Ctrl Pts',(-40.4176364341705,36.4422862478988,37.5755891340256));
#24970=CARTESIAN_POINT('Ctrl Pts',(-40.4477579176795,36.4624137833476,37.6128888625783));
#24971=CARTESIAN_POINT('Ctrl Pts',(-40.4776501015213,36.4832835020608,37.6499556373456));
#24972=CARTESIAN_POINT('Ctrl Pts',(-40.5075422853631,36.5041532207739,37.687022412113));
#24973=CARTESIAN_POINT('Ctrl Pts',(-40.537205168588,36.52576512209,37.7238562319229));
#24974=CARTESIAN_POINT('Ctrl Pts',(-40.5666243209561,36.5481086923639,37.7604391780458));
#24975=CARTESIAN_POINT('Ctrl Pts',(-40.5960434733241,36.5704522626378,37.7970221241688));
#24976=CARTESIAN_POINT('Ctrl Pts',(-40.6252188939058,36.5935275011641,37.8333541954497));
#24977=CARTESIAN_POINT('Ctrl Pts',(-40.6541363895764,36.61732318241,37.8694177172388));
#24978=CARTESIAN_POINT('Ctrl Pts',(-40.683053885247,36.641118863656,37.9054812390279));
#24979=CARTESIAN_POINT('Ctrl Pts',(-40.7117134550993,36.6656349868731,37.941276210189));
#24980=CARTESIAN_POINT('Ctrl Pts',(-40.7401011569678,36.6908596255793,37.976785217362));
#24981=CARTESIAN_POINT('Ctrl Pts',(-40.7684888588364,36.7160842642856,38.0122942245349));
#24982=CARTESIAN_POINT('Ctrl Pts',(-40.7966046918253,36.7420174176848,38.0475172665991));
#24983=CARTESIAN_POINT('Ctrl Pts',(-40.8244349782834,36.7686464699451,38.0824372084235));
#24984=CARTESIAN_POINT('Ctrl Pts',(-40.8522652647416,36.7952755222055,38.117357150248));
#24985=CARTESIAN_POINT('Ctrl Pts',(-40.8798100037906,36.8226004724864,38.1519739907306));
#24986=CARTESIAN_POINT('Ctrl Pts',(-40.9070557956025,36.8506080278818,38.1862708896424));
#24987=CARTESIAN_POINT('Ctrl Pts',(-40.9343015874144,36.8786155832771,38.2205677885543));
#24988=CARTESIAN_POINT('Ctrl Pts',(-40.9612484311292,36.9073057429028,38.2545447448129));
#24989=CARTESIAN_POINT('Ctrl Pts',(-40.98788321778,36.9366645497122,38.2881852294771));
#24990=CARTESIAN_POINT('Ctrl Pts',(-41.0145180044308,36.9660233565217,38.3218257141413));
#24991=CARTESIAN_POINT('Ctrl Pts',(-41.040840733177,36.9960508095882,38.3551297261493));
#24992=CARTESIAN_POINT('Ctrl Pts',(-41.0668385986679,37.0267323013055,38.3880810639305));
#24993=CARTESIAN_POINT('Ctrl Pts',(-41.0928364641588,37.0574137930227,38.4210324017117));
#24994=CARTESIAN_POINT('Ctrl Pts',(-41.118509465574,37.0887493224222,38.4536310642261));
#24995=CARTESIAN_POINT('Ctrl Pts',(-41.143845113639,37.120723645551,38.485861193038));
#24996=CARTESIAN_POINT('Ctrl Pts',(-41.1691807617039,37.1526979686799,38.5180913218498));
#24997=CARTESIAN_POINT('Ctrl Pts',(-41.1941790556189,37.1853110845287,38.5499529159419));
#24998=CARTESIAN_POINT('Ctrl Pts',(-41.2188278343383,37.2185471276312,38.5814304754439));
#24999=CARTESIAN_POINT('Ctrl Pts',(-39.7640356868581,36.1452644659848,36.8199666945997));
#25000=CARTESIAN_POINT('Ctrl Pts',(-39.7972721141141,36.1549963036626,36.8603543355419));
#25001=CARTESIAN_POINT('Ctrl Pts',(-39.8303858770236,36.1655619996249,36.900641732437));
#25002=CARTESIAN_POINT('Ctrl Pts',(-39.8633601352655,36.1769561677082,36.9408083947699));
#25003=CARTESIAN_POINT('Ctrl Pts',(-39.8963051138968,36.1883402182992,36.9809393909714));
#25004=CARTESIAN_POINT('Ctrl Pts',(-39.9291108343684,36.2005512699824,37.0209498655521));
#25005=CARTESIAN_POINT('Ctrl Pts',(-39.9617606427354,36.2135831119758,37.0608195050832));
#25006=CARTESIAN_POINT('Ctrl Pts',(-39.9944104511025,36.2266149539692,37.1006891446142));
#25007=CARTESIAN_POINT('Ctrl Pts',(-40.0269043462439,36.2404675858242,37.1404179477271));
#25008=CARTESIAN_POINT('Ctrl Pts',(-40.0592258325677,36.2551339640915,37.1799857441024));
#25009=CARTESIAN_POINT('Ctrl Pts',(-40.0915473188916,36.2698003423587,37.2195535404778));
#25010=CARTESIAN_POINT('Ctrl Pts',(-40.12369639529,36.2852804665335,37.2589603287583));
#25011=CARTESIAN_POINT('Ctrl Pts',(-40.155656741322,36.3015664676697,37.2981861022112));
#25012=CARTESIAN_POINT('Ctrl Pts',(-40.1876170873539,36.3178524688058,37.3374118756642));
#25013=CARTESIAN_POINT('Ctrl Pts',(-40.2193887019217,36.3349443463432,37.3764566329429));
#25014=CARTESIAN_POINT('Ctrl Pts',(-40.2509554562059,36.3528334138032,37.4153005511544));
#25015=CARTESIAN_POINT('Ctrl Pts',(-40.2825222104901,36.3707224812631,37.4541444693658));
#25016=CARTESIAN_POINT('Ctrl Pts',(-40.3138841034159,36.3894087380334,37.4927875471801));
#25017=CARTESIAN_POINT('Ctrl Pts',(-40.345025214184,36.4088826889328,37.5312101656569));
#25018=CARTESIAN_POINT('Ctrl Pts',(-40.3761663249522,36.4283566398322,37.5696327841337));
#25019=CARTESIAN_POINT('Ctrl Pts',(-40.4070866524941,36.4486182841913,37.6078349419546));
#25020=CARTESIAN_POINT('Ctrl Pts',(-40.4377705001518,36.4696573277541,37.6457972440136));
#25021=CARTESIAN_POINT('Ctrl Pts',(-40.4684543478096,36.4906963713168,37.6837595460726));
#25022=CARTESIAN_POINT('Ctrl Pts',(-40.4989017145245,36.5125128133576,37.721481991065));
#25023=CARTESIAN_POINT('Ctrl Pts',(-40.5290971437017,36.5350955709923,37.7589454273838));
#25024=CARTESIAN_POINT('Ctrl Pts',(-40.5592925728788,36.5576783286271,37.7964088637025));
#25025=CARTESIAN_POINT('Ctrl Pts',(-40.5892360634811,36.5810274010797,37.8336132900617));
#25026=CARTESIAN_POINT('Ctrl Pts',(-40.6189124146098,36.6051309280642,37.8705398177552));
#25027=CARTESIAN_POINT('Ctrl Pts',(-40.6485887657384,36.6292344550487,37.9074663454486));
#25028=CARTESIAN_POINT('Ctrl Pts',(-40.6779979763803,36.6540924357396,37.9441149732111));
#25029=CARTESIAN_POINT('Ctrl Pts',(-40.7071251167728,36.6796922444917,37.980467094396));
#25030=CARTESIAN_POINT('Ctrl Pts',(-40.7362522571653,36.7052920532438,38.016819215581));
#25031=CARTESIAN_POINT('Ctrl Pts',(-40.765097326309,36.7316336891779,38.052874828941));
#25032=CARTESIAN_POINT('Ctrl Pts',(-40.7936456806999,36.7587037740886,38.0886156287471));
#25033=CARTESIAN_POINT('Ctrl Pts',(-40.8221940350909,36.7857738589993,38.1243564285532));
#25034=CARTESIAN_POINT('Ctrl Pts',(-40.8504456737495,36.813572391957,38.1597824135788));
#25035=CARTESIAN_POINT('Ctrl Pts',(-40.878386254274,36.8420852557614,38.1948755975695));
#25036=CARTESIAN_POINT('Ctrl Pts',(-40.9063268347985,36.8705981195658,38.2299687815601));
#25037=CARTESIAN_POINT('Ctrl Pts',(-40.9339563562299,36.8998253132381,38.2647291633114));
#25038=CARTESIAN_POINT('Ctrl Pts',(-40.9612607918061,36.9297519948971,38.2991390942759));
#25039=CARTESIAN_POINT('Ctrl Pts',(-40.9885652273823,36.9596786765562,38.3335490252404));
#25040=CARTESIAN_POINT('Ctrl Pts',(-41.0155445761664,36.9903048451747,38.3676085042373));
#25041=CARTESIAN_POINT('Ctrl Pts',(-41.0421851412539,37.0216149492393,38.4013002383173));
#25042=CARTESIAN_POINT('Ctrl Pts',(-41.0688257063413,37.0529250533041,38.4349919723972));
#25043=CARTESIAN_POINT('Ctrl Pts',(-41.0951274868181,37.0849190917401,38.468315960404));
#25044=CARTESIAN_POINT('Ctrl Pts',(-41.1210771295217,37.1175808191686,38.5012552825171));
#25045=CARTESIAN_POINT('Ctrl Pts',(-41.1470267722253,37.1502425465971,38.5341946046302));
#25046=CARTESIAN_POINT('Ctrl Pts',(-41.172624276265,37.1835719618968,38.5667492597192));
#25047=CARTESIAN_POINT('Ctrl Pts',(-41.1978566457567,37.2175521422934,38.598902718245));
#25048=CARTESIAN_POINT('Ctrl Pts',(-39.7077998441206,36.1346589387687,36.7975281492573));
#25049=CARTESIAN_POINT('Ctrl Pts',(-39.7418511624317,36.144018504291,36.8388168379438));
#25050=CARTESIAN_POINT('Ctrl Pts',(-39.7757808173037,36.1542494580266,36.8800080725771));
#25051=CARTESIAN_POINT('Ctrl Pts',(-39.8095708106025,36.1653463593505,36.9210800011996));
#25052=CARTESIAN_POINT('Ctrl Pts',(-39.8433307999561,36.1764334071412,36.9621154598563));
#25053=CARTESIAN_POINT('Ctrl Pts',(-39.8769513743958,36.1883848649453,37.0030318227539));
#25054=CARTESIAN_POINT('Ctrl Pts',(-39.910414731496,36.201194391942,37.0438074224316));
#25055=CARTESIAN_POINT('Ctrl Pts',(-39.9438780885963,36.2140039189387,37.0845830221094));
#25056=CARTESIAN_POINT('Ctrl Pts',(-39.9771842271081,36.227671514648,37.125217857045));
#25057=CARTESIAN_POINT('Ctrl Pts',(-40.0103155112345,36.2421899302918,37.165690409025));
#25058=CARTESIAN_POINT('Ctrl Pts',(-40.0434467953608,36.2567083459355,37.206162961005));
#25059=CARTESIAN_POINT('Ctrl Pts',(-40.076403223862,36.2720775809692,37.2464732285173));
#25060=CARTESIAN_POINT('Ctrl Pts',(-40.1091673462115,36.2882894863336,37.2865998653457));
#25061=CARTESIAN_POINT('Ctrl Pts',(-40.1419314685611,36.304501391698,37.3267265021742));
#25062=CARTESIAN_POINT('Ctrl Pts',(-40.1745032835359,36.3215559667863,37.3666695068207));
#25063=CARTESIAN_POINT('Ctrl Pts',(-40.206865544319,36.339444170883,37.4064077276318));
#25064=CARTESIAN_POINT('Ctrl Pts',(-40.2392278051021,36.3573323749797,37.4461459484429));
#25065=CARTESIAN_POINT('Ctrl Pts',(-40.2713805104875,36.3760542074162,37.4856793839357));
#25066=CARTESIAN_POINT('Ctrl Pts',(-40.3033066356117,36.3955997453937,37.5249870993869));
#25067=CARTESIAN_POINT('Ctrl Pts',(-40.335232760736,36.4151452833711,37.5642948148381));
#25068=CARTESIAN_POINT('Ctrl Pts',(-40.3669323044075,36.4355145261586,37.6033768087801));
#25069=CARTESIAN_POINT('Ctrl Pts',(-40.3983884817113,36.4566966793738,37.642212385552));
#25070=CARTESIAN_POINT('Ctrl Pts',(-40.4298446590152,36.477878832589,37.6810479623239));
#25071=CARTESIAN_POINT('Ctrl Pts',(-40.461057468776,36.4998738954397,37.7196371204753));
#25072=CARTESIAN_POINT('Ctrl Pts',(-40.4920103837744,36.5226702133831,37.7579594252896));
#25073=CARTESIAN_POINT('Ctrl Pts',(-40.5229632987728,36.5454665313265,37.7962817301039));
#25074=CARTESIAN_POINT('Ctrl Pts',(-40.5536563178532,36.5690641035108,37.8343371801503));
#25075=CARTESIAN_POINT('Ctrl Pts',(-40.5840731889565,36.5934504275596,37.8721056232587));
#25076=CARTESIAN_POINT('Ctrl Pts',(-40.6144900600598,36.6178367516085,37.9098740663671));
#25077=CARTESIAN_POINT('Ctrl Pts',(-40.6446307820518,36.6430118266113,37.9473555011279));
#25078=CARTESIAN_POINT('Ctrl Pts',(-40.6744793952223,36.6689623155878,37.9845300792268));
#25079=CARTESIAN_POINT('Ctrl Pts',(-40.7043280083928,36.6949128045642,38.0217046573258));
#25080=CARTESIAN_POINT('Ctrl Pts',(-40.7338845116276,36.7216387065447,38.058572377375));
#25081=CARTESIAN_POINT('Ctrl Pts',(-40.7631332544355,36.7491258640507,38.0951137159004));
#25082=CARTESIAN_POINT('Ctrl Pts',(-40.7923819972434,36.7766130215566,38.1316550544258));
#25083=CARTESIAN_POINT('Ctrl Pts',(-40.821322978534,36.8048614335622,38.1678700100637));
#25084=CARTESIAN_POINT('Ctrl Pts',(-40.8499408735779,36.8338561370629,38.2037394048213));
#25085=CARTESIAN_POINT('Ctrl Pts',(-40.8785587686217,36.8628508405637,38.239608799579));
#25086=CARTESIAN_POINT('Ctrl Pts',(-40.9068535763509,36.8925918344768,38.2751326321173));
#25087=CARTESIAN_POINT('Ctrl Pts',(-40.9348103140075,36.9230633661018,38.3102920902048));
#25088=CARTESIAN_POINT('Ctrl Pts',(-40.9627670516641,36.9535348977268,38.3454515482923));
#25089=CARTESIAN_POINT('Ctrl Pts',(-40.9903857182032,36.9847369659249,38.3802466306157));
#25090=CARTESIAN_POINT('Ctrl Pts',(-41.0176516886709,37.0166530449538,38.4146589105926));
#25091=CARTESIAN_POINT('Ctrl Pts',(-41.0449176591385,37.0485691239827,38.4490711905695));
#25092=CARTESIAN_POINT('Ctrl Pts',(-41.0718309325168,37.0811992126505,38.4831006669151));
#25093=CARTESIAN_POINT('Ctrl Pts',(-41.0983772571203,37.1145260296501,38.5167293181798));
#25094=CARTESIAN_POINT('Ctrl Pts',(-41.1249235817238,37.1478528466497,38.5503579694445));
#25095=CARTESIAN_POINT('Ctrl Pts',(-41.1511029565612,37.1818763907364,38.5835857943725));
#25096=CARTESIAN_POINT('Ctrl Pts',(-41.1769015182838,37.2165786433123,38.6163951957028));
#25097=CARTESIAN_POINT('Ctrl Pts',(-39.6523857950171,36.125116607414,36.776029662523));
#25098=CARTESIAN_POINT('Ctrl Pts',(-39.6872293819169,36.1340785824282,36.818193511888));
#25099=CARTESIAN_POINT('Ctrl Pts',(-39.7219528960408,36.1439495968667,36.860263368761));
#25100=CARTESIAN_POINT('Ctrl Pts',(-39.7565371387752,36.154724192588,36.9022159727179));
#25101=CARTESIAN_POINT('Ctrl Pts',(-39.7910906723076,36.1654892209686,36.9441313247103));
#25102=CARTESIAN_POINT('Ctrl Pts',(-39.8255051802735,36.1771562262313,36.9859296302228));
#25103=CARTESIAN_POINT('Ctrl Pts',(-39.85976166862,36.1897187691237,37.0275878199396));
#25104=CARTESIAN_POINT('Ctrl Pts',(-39.8940181569666,36.2022813120162,37.0692460096564));
#25105=CARTESIAN_POINT('Ctrl Pts',(-39.9281166243022,36.2157393920279,37.1107640818852));
#25106=CARTESIAN_POINT('Ctrl Pts',(-39.9620382510075,36.2300855813778,37.1521191219778));
#25107=CARTESIAN_POINT('Ctrl Pts',(-39.9959598777127,36.2444317707276,37.1934741620704));
#25108=CARTESIAN_POINT('Ctrl Pts',(-40.0297046624065,36.2596660688321,37.2346661683455));
#25109=CARTESIAN_POINT('Ctrl Pts',(-40.0632539806756,36.2757800675803,37.2756724061182));
#25110=CARTESIAN_POINT('Ctrl Pts',(-40.0968032989448,36.2918940663284,37.316678643891));
#25111=CARTESIAN_POINT('Ctrl Pts',(-40.1301571494261,36.3088877650658,37.3574991114952));
#25112=CARTESIAN_POINT('Ctrl Pts',(-40.1632971234634,36.3267517846313,37.3981112793026));
#25113=CARTESIAN_POINT('Ctrl Pts',(-40.1964370975007,36.3446158041968,37.43872344711));
#25114=CARTESIAN_POINT('Ctrl Pts',(-40.2293631937494,36.3633501438654,37.4791273134714));
#25115=CARTESIAN_POINT('Ctrl Pts',(-40.262057239643,36.3829444637826,37.5193005786902));
#25116=CARTESIAN_POINT('Ctrl Pts',(-40.2947512855366,36.4025387836998,37.559473843909));
#25117=CARTESIAN_POINT('Ctrl Pts',(-40.3272132797466,36.4229930830697,37.5994165063532));
#25118=CARTESIAN_POINT('Ctrl Pts',(-40.3594253058539,36.4442960727581,37.6391065208739));
#25119=CARTESIAN_POINT('Ctrl Pts',(-40.3916373319611,36.4655990624466,37.6787965353945));
#25120=CARTESIAN_POINT('Ctrl Pts',(-40.4235993886555,36.4877507415875,37.7182339003787));
#25121=CARTESIAN_POINT('Ctrl Pts',(-40.4552938354456,36.5107388842303,37.7573968495623));
#25122=CARTESIAN_POINT('Ctrl Pts',(-40.4869882822357,36.5337270268732,37.7965597987459));
#25123=CARTESIAN_POINT('Ctrl Pts',(-40.5184151178338,36.5575516320839,37.8354483305377));
#25124=CARTESIAN_POINT('Ctrl Pts',(-40.5495569971425,36.5821995505885,37.8740409815837));
#25125=CARTESIAN_POINT('Ctrl Pts',(-40.5806988764513,36.6068474690932,37.9126336326297));
#25126=CARTESIAN_POINT('Ctrl Pts',(-40.6115557982068,36.6323186998909,37.9509304013623));
#25127=CARTESIAN_POINT('Ctrl Pts',(-40.6421107318609,36.6585991849036,37.9889101510342));
#25128=CARTESIAN_POINT('Ctrl Pts',(-40.6726656655151,36.6848796699162,38.0268899007062));
#25129=CARTESIAN_POINT('Ctrl Pts',(-40.7029186098265,36.711969408076,38.0645526297744));
#25130=CARTESIAN_POINT('Ctrl Pts',(-40.7328528675943,36.7398534480183,38.1018775514305));
#25131=CARTESIAN_POINT('Ctrl Pts',(-40.762787125362,36.7677374879607,38.1392024730866));
#25132=CARTESIAN_POINT('Ctrl Pts',(-40.7924026953714,36.7964158285534,38.1761895858147));
#25133=CARTESIAN_POINT('Ctrl Pts',(-40.8216832321981,36.8258726416493,38.2128184756916));
#25134=CARTESIAN_POINT('Ctrl Pts',(-40.8509637690248,36.8553294547451,38.2494473655685));
#25135=CARTESIAN_POINT('Ctrl Pts',(-40.8799092714797,36.8855647391474,38.2857180311063));
#25136=CARTESIAN_POINT('Ctrl Pts',(-40.9085037639673,36.9165618074033,38.3216104538048));
#25137=CARTESIAN_POINT('Ctrl Pts',(-40.9370982564548,36.9475588756594,38.3575028765032));
#25138=CARTESIAN_POINT('Ctrl Pts',(-40.965341737812,36.979317726509,38.3930170549038));
#25139=CARTESIAN_POINT('Ctrl Pts',(-40.9932186199006,37.0118208316117,38.4281333880261));
#25140=CARTESIAN_POINT('Ctrl Pts',(-41.0210955019892,37.0443239367144,38.4632497211483));
#25141=CARTESIAN_POINT('Ctrl Pts',(-41.0486057836766,37.0775712947497,38.4979682075655));
#25142=CARTESIAN_POINT('Ctrl Pts',(-41.0757342814917,37.1115445558401,38.5322696854552));
#25143=CARTESIAN_POINT('Ctrl Pts',(-41.1028627793069,37.1455178169305,38.566571163345));
#25144=CARTESIAN_POINT('Ctrl Pts',(-41.1296094921476,37.1802169796957,38.6004556313137));
#25145=CARTESIAN_POINT('Ctrl Pts',(-41.1559596579721,37.2156228929789,38.6339043878506));
#25146=CARTESIAN_POINT('Ctrl Pts',(-39.5969717459136,36.1155742760594,36.7545311757887));
#25147=CARTESIAN_POINT('Ctrl Pts',(-39.6326076014021,36.1241386605654,36.7975701858321));
#25148=CARTESIAN_POINT('Ctrl Pts',(-39.6681249747779,36.1336497357067,36.8405186649448));
#25149=CARTESIAN_POINT('Ctrl Pts',(-39.7035034669478,36.1441020258255,36.8833519442363));
#25150=CARTESIAN_POINT('Ctrl Pts',(-39.7388505446591,36.154545034796,36.9261471895641));
#25151=CARTESIAN_POINT('Ctrl Pts',(-39.7740589861511,36.1659275875173,36.9688274376917));
#25152=CARTESIAN_POINT('Ctrl Pts',(-39.809108605744,36.1782431463054,37.0113682174476));
#25153=CARTESIAN_POINT('Ctrl Pts',(-39.8441582253369,36.1905587050936,37.0539089972035));
#25154=CARTESIAN_POINT('Ctrl Pts',(-39.8790490214964,36.2038072694078,37.0963103067254));
#25155=CARTESIAN_POINT('Ctrl Pts',(-39.9137609907805,36.2179812324638,37.1385478349306));
#25156=CARTESIAN_POINT('Ctrl Pts',(-39.9484729600646,36.2321551955198,37.1807853631357));
#25157=CARTESIAN_POINT('Ctrl Pts',(-39.983006100951,36.2472545566949,37.2228591081738));
#25158=CARTESIAN_POINT('Ctrl Pts',(-40.0173406151398,36.2632706488268,37.2647449468908));
#25159=CARTESIAN_POINT('Ctrl Pts',(-40.0516751293285,36.2792867409589,37.3066307856078));
#25160=CARTESIAN_POINT('Ctrl Pts',(-40.0858110153162,36.2962195633453,37.3483287161697));
#25161=CARTESIAN_POINT('Ctrl Pts',(-40.1197287026078,36.3140593983796,37.3898148309734));
#25162=CARTESIAN_POINT('Ctrl Pts',(-40.1536463898993,36.331899233414,37.4313009457772));
#25163=CARTESIAN_POINT('Ctrl Pts',(-40.1873458770115,36.3506460803144,37.472575243007));
#25164=CARTESIAN_POINT('Ctrl Pts',(-40.2208078436743,36.3702891821715,37.5136140579935));
#25165=CARTESIAN_POINT('Ctrl Pts',(-40.2542698103372,36.3899322840284,37.55465287298));
#25166=CARTESIAN_POINT('Ctrl Pts',(-40.2874942550859,36.4104716399808,37.5954562039263));
#25167=CARTESIAN_POINT('Ctrl Pts',(-40.3204621299964,36.4318954661425,37.6360006561957));
#25168=CARTESIAN_POINT('Ctrl Pts',(-40.353430004907,36.4533192923041,37.6765451084652));
#25169=CARTESIAN_POINT('Ctrl Pts',(-40.386141308535,36.4756275877353,37.7168306802822));
#25170=CARTESIAN_POINT('Ctrl Pts',(-40.4185772871168,36.4988075550775,37.7568342738351));
#25171=CARTESIAN_POINT('Ctrl Pts',(-40.4510132656987,36.5219875224197,37.796837867388));
#25172=CARTESIAN_POINT('Ctrl Pts',(-40.4831739178143,36.546039160657,37.8365594809252));
#25173=CARTESIAN_POINT('Ctrl Pts',(-40.5150408053285,36.5709486736174,37.8759763399087));
#25174=CARTESIAN_POINT('Ctrl Pts',(-40.5469076928428,36.5958581865779,37.9153931988922));
#25175=CARTESIAN_POINT('Ctrl Pts',(-40.5784808143618,36.6216255731705,37.9545053015968));
#25176=CARTESIAN_POINT('Ctrl Pts',(-40.6097420684995,36.6482360542194,37.9932902228416));
#25177=CARTESIAN_POINT('Ctrl Pts',(-40.6410033226373,36.6748465352682,38.0320751440866));
#25178=CARTESIAN_POINT('Ctrl Pts',(-40.6719527080254,36.7023001096073,38.0705328821738));
#25179=CARTESIAN_POINT('Ctrl Pts',(-40.702572480753,36.730581031986,38.1086413869606));
#25180=CARTESIAN_POINT('Ctrl Pts',(-40.7331922534806,36.7588619543647,38.1467498917474));
#25181=CARTESIAN_POINT('Ctrl Pts',(-40.7634824122088,36.7879702235447,38.1845091615657));
#25182=CARTESIAN_POINT('Ctrl Pts',(-40.7934255908184,36.8178891462356,38.2218975465619));
#25183=CARTESIAN_POINT('Ctrl Pts',(-40.823368769428,36.8478080689265,38.2592859315581));
#25184=CARTESIAN_POINT('Ctrl Pts',(-40.8529649666086,36.878537643818,38.2963034300953));
#25185=CARTESIAN_POINT('Ctrl Pts',(-40.882197213927,36.9100602487049,38.3329288174047));
#25186=CARTESIAN_POINT('Ctrl Pts',(-40.9114294612455,36.9415828535918,38.3695542047142));
#25187=CARTESIAN_POINT('Ctrl Pts',(-40.9402977574209,36.9738984870931,38.405787479192));
#25188=CARTESIAN_POINT('Ctrl Pts',(-40.9687855511304,37.0069886182696,38.4416078654595));
#25189=CARTESIAN_POINT('Ctrl Pts',(-40.9972733448399,37.0400787494461,38.477428251727));
#25190=CARTESIAN_POINT('Ctrl Pts',(-41.0253806348363,37.0739433768488,38.5128357482158));
#25191=CARTESIAN_POINT('Ctrl Pts',(-41.0530913058632,37.10856308203,38.5478100527307));
#25192=CARTESIAN_POINT('Ctrl Pts',(-41.0808019768901,37.1431827872113,38.5827843572455));
#25193=CARTESIAN_POINT('Ctrl Pts',(-41.1081160277341,37.1785575686551,38.6173254682549));
#25194=CARTESIAN_POINT('Ctrl Pts',(-41.1350177976604,37.2146671426455,38.6514135799984));
#25195=CARTESIAN_POINT('Ctrl Pts',(-39.5423802548784,36.107096302736,36.7339737388304));
#25196=CARTESIAN_POINT('Ctrl Pts',(-39.5787857407974,36.1152377518645,36.7778620020655));
#25197=CARTESIAN_POINT('Ctrl Pts',(-39.6150749250676,36.1243636643348,36.8216638675484));
#25198=CARTESIAN_POINT('Ctrl Pts',(-39.6512261654248,36.1344685839076,36.8653532108844));
#25199=CARTESIAN_POINT('Ctrl Pts',(-39.6873453051588,36.144564530781,36.9090037601118));
#25200=CARTESIAN_POINT('Ctrl Pts',(-39.7233267441435,36.1556377464239,36.9525419848725));
#25201=CARTESIAN_POINT('Ctrl Pts',(-39.7591490619367,36.1676816263223,36.9959419643159));
#25202=CARTESIAN_POINT('Ctrl Pts',(-39.7949713797299,36.1797255062207,37.0393419437593));
#25203=CARTESIAN_POINT('Ctrl Pts',(-39.8306345746389,36.1927400498046,37.0826036758357));
#25204=CARTESIAN_POINT('Ctrl Pts',(-39.8661174157609,36.2067174976021,37.125701404476));
#25205=CARTESIAN_POINT('Ctrl Pts',(-39.9016002568831,36.2206949453995,37.1687991331163));
#25206=CARTESIAN_POINT('Ctrl Pts',(-39.9369027425454,36.2356352967486,37.2117328562867));
#25207=CARTESIAN_POINT('Ctrl Pts',(-39.9720038567691,36.2515296464936,37.2544770133768));
#25208=CARTESIAN_POINT('Ctrl Pts',(-40.0071049709929,36.2674239962385,37.2972211704668));
#25209=CARTESIAN_POINT('Ctrl Pts',(-40.0420047121196,36.2842723436275,37.3397757594581));
#25210=CARTESIAN_POINT('Ctrl Pts',(-40.0766823039535,36.3020646483887,37.382115445547));
#25211=CARTESIAN_POINT('Ctrl Pts',(-40.1113598957873,36.31985695315,37.4244551316359));
#25212=CARTESIAN_POINT('Ctrl Pts',(-40.1458153367065,36.3385932144465,37.4665799128291));
#25213=CARTESIAN_POINT('Ctrl Pts',(-40.180028115093,36.3582622688683,37.5084647102876));
#25214=CARTESIAN_POINT('Ctrl Pts',(-40.2142408934795,36.37793132329,37.5503495077461));
#25215=CARTESIAN_POINT('Ctrl Pts',(-40.2482110077184,36.3985331699072,37.5919943194928));
#25216=CARTESIAN_POINT('Ctrl Pts',(-40.2819182351279,36.4200555354481,37.6333743524638));
#25217=CARTESIAN_POINT('Ctrl Pts',(-40.3156254625376,36.4415779009889,37.6747543854349));
#25218=CARTESIAN_POINT('Ctrl Pts',(-40.3490698015163,36.4640207844321,37.7158696376735));
#25219=CARTESIAN_POINT('Ctrl Pts',(-40.3822313423855,36.4873708172573,37.7566956313795));
#25220=CARTESIAN_POINT('Ctrl Pts',(-40.4153928832547,36.5107208500824,37.7975216250854));
#25221=CARTESIAN_POINT('Ctrl Pts',(-40.4482716244472,36.5349780311859,37.8380583583306));
#25222=CARTESIAN_POINT('Ctrl Pts',(-40.4808479928981,36.5601279126792,37.8782816976643));
#25223=CARTESIAN_POINT('Ctrl Pts',(-40.513424361349,36.5852777941724,37.9185050369981));
#25224=CARTESIAN_POINT('Ctrl Pts',(-40.5456983555303,36.6113203748713,37.9584149805247));
#25225=CARTESIAN_POINT('Ctrl Pts',(-40.5776507623225,36.638240144732,37.9979877678588));
#25226=CARTESIAN_POINT('Ctrl Pts',(-40.6096031691147,36.6651599145927,38.0375605551929));
#25227=CARTESIAN_POINT('Ctrl Pts',(-40.6412339870097,36.6929568723436,38.0767961844664));
#25228=CARTESIAN_POINT('Ctrl Pts',(-40.6725243856593,36.7216144642273,38.115671296607));
#25229=CARTESIAN_POINT('Ctrl Pts',(-40.703814784309,36.750272056111,38.1545464087476));
#25230=CARTESIAN_POINT('Ctrl Pts',(-40.7347647622311,36.779790280771,38.1930610019186));
#25231=CARTESIAN_POINT('Ctrl Pts',(-40.7653558942499,36.8101515604333,38.23119214614));
#25232=CARTESIAN_POINT('Ctrl Pts',(-40.7959470262687,36.8405128400955,38.2693232903614));
#25233=CARTESIAN_POINT('Ctrl Pts',(-40.8261793109386,36.8717171733253,38.3070709838326));
#25234=CARTESIAN_POINT('Ctrl Pts',(-40.8560347501336,36.9037459792209,38.3444127529239));
#25235=CARTESIAN_POINT('Ctrl Pts',(-40.8858901893285,36.9357747851167,38.3817545220151));
#25236=CARTESIAN_POINT('Ctrl Pts',(-40.9153687816438,36.9686280621686,38.4186903649647));
#25237=CARTESIAN_POINT('Ctrl Pts',(-40.944452977432,37.0022862484628,38.4551982912251));
#25238=CARTESIAN_POINT('Ctrl Pts',(-40.9735371732202,37.035944434757,38.4917062174854));
#25239=CARTESIAN_POINT('Ctrl Pts',(-41.0022269711084,37.0704075287042,38.5277862253329));
#25240=CARTESIAN_POINT('Ctrl Pts',(-41.0305052907871,37.1056550106378,38.5634168334495));
#25241=CARTESIAN_POINT('Ctrl Pts',(-41.0587836104657,37.1409024925713,38.5990474415661));
#25242=CARTESIAN_POINT('Ctrl Pts',(-41.0866504505995,37.1769343608268,38.6342286482694));
#25243=CARTESIAN_POINT('Ctrl Pts',(-41.1140892205275,37.2137291623881,38.6689395070162));
#25244=CARTESIAN_POINT('Ctrl Pts',(-39.4885029329456,36.0995357124289,36.7142288179568));
#25245=CARTESIAN_POINT('Ctrl Pts',(-39.5256578065064,36.1072322970532,36.7589432482088));
#25246=CARTESIAN_POINT('Ctrl Pts',(-39.5626991277534,36.1159511992982,36.8035760623136));
#25247=CARTESIAN_POINT('Ctrl Pts',(-39.5996039709717,36.1256870222641,36.8480996360113));
#25248=CARTESIAN_POINT('Ctrl Pts',(-39.6364760444026,36.135414200271,36.8925836748425));
#25249=CARTESIAN_POINT('Ctrl Pts',(-39.6732118801939,36.1461564933479,36.9369586649175));
#25250=CARTESIAN_POINT('Ctrl Pts',(-39.7097887820638,36.1579072646444,36.9811971902702));
#25251=CARTESIAN_POINT('Ctrl Pts',(-39.7463656839339,36.1696580359408,37.0254357156229));
#25252=CARTESIAN_POINT('Ctrl Pts',(-39.7827836500186,36.182417284859,37.0695377740005));
#25253=CARTESIAN_POINT('Ctrl Pts',(-39.8190201803537,36.1961771284081,37.113476118036));
#25254=CARTESIAN_POINT('Ctrl Pts',(-39.8552567106888,36.2099369719573,37.1574144620715));
#25255=CARTESIAN_POINT('Ctrl Pts',(-39.8913118034313,36.2246974094365,37.2011890895288));
#25256=CARTESIAN_POINT('Ctrl Pts',(-39.927163182874,36.2404493214864,37.2447729553587));
#25257=CARTESIAN_POINT('Ctrl Pts',(-39.9630145623167,36.2562012335362,37.2883568211886));
#25258=CARTESIAN_POINT('Ctrl Pts',(-39.9986622266328,36.2729446193549,37.3317499231716));
#25259=CARTESIAN_POINT('Ctrl Pts',(-40.0340841517748,36.2906691344516,37.3749254519539));
#25260=CARTESIAN_POINT('Ctrl Pts',(-40.0695060769167,36.3083936495484,37.4181009807362));
#25261=CARTESIAN_POINT('Ctrl Pts',(-40.1047022610957,36.3270992930248,37.4610589341247));
#25262=CARTESIAN_POINT('Ctrl Pts',(-40.1396509592288,36.3467745080664,37.5037727716212));
#25263=CARTESIAN_POINT('Ctrl Pts',(-40.1745996573619,36.366449723108,37.5464866091177));
#25264=CARTESIAN_POINT('Ctrl Pts',(-40.2093008676697,36.3870945087132,37.5889563285476));
#25265=CARTESIAN_POINT('Ctrl Pts',(-40.2437331508764,36.4086961100169,37.6311556910557));
#25266=CARTESIAN_POINT('Ctrl Pts',(-40.2781654340831,36.4302977113206,37.6733550535639));
#25267=CARTESIAN_POINT('Ctrl Pts',(-40.3123287884256,36.4528561272191,37.7152840569987));
#25268=CARTESIAN_POINT('Ctrl Pts',(-40.3462021069497,36.4763574205668,37.7569167965795));
#25269=CARTESIAN_POINT('Ctrl Pts',(-40.3800754254738,36.4998587139144,37.7985495361603));
#25270=CARTESIAN_POINT('Ctrl Pts',(-40.4136587064533,36.5243028835146,37.8398860097669));
#25271=CARTESIAN_POINT('Ctrl Pts',(-40.4469312012788,36.54967482714,37.8809006786862));
#25272=CARTESIAN_POINT('Ctrl Pts',(-40.4802036961043,36.5750467707654,37.9219153476056));
#25273=CARTESIAN_POINT('Ctrl Pts',(-40.5131654030913,36.6013464871283,37.9626082097524));
#25274=CARTESIAN_POINT('Ctrl Pts',(-40.5457959576725,36.6285577276059,38.0029541240585));
#25275=CARTESIAN_POINT('Ctrl Pts',(-40.5784265122537,36.6557689680836,38.0433000383647));
#25276=CARTESIAN_POINT('Ctrl Pts',(-40.6107259127679,36.6838917312907,38.083299002776));
#25277=CARTESIAN_POINT('Ctrl Pts',(-40.6426742038376,36.7129086422805,38.1229263049318));
#25278=CARTESIAN_POINT('Ctrl Pts',(-40.6746224949072,36.7419255532703,38.1625536070876));
#25279=CARTESIAN_POINT('Ctrl Pts',(-40.7062196749005,36.7718366105629,38.2018092449689));
#25280=CARTESIAN_POINT('Ctrl Pts',(-40.7374462223,36.8026233343645,38.2406689654636));
#25281=CARTESIAN_POINT('Ctrl Pts',(-40.7686727696995,36.833410058166,38.2795286859583));
#25282=CARTESIAN_POINT('Ctrl Pts',(-40.7995286829138,36.8650724469085,38.3179924870875));
#25283=CARTESIAN_POINT('Ctrl Pts',(-40.8299948983795,36.8975909387715,38.3560366049504));
#25284=CARTESIAN_POINT('Ctrl Pts',(-40.8604611138452,36.9301094306343,38.3940807228133));
#25285=CARTESIAN_POINT('Ctrl Pts',(-40.8905376300156,36.9634840239645,38.4317051554743));
#25286=CARTESIAN_POINT('Ctrl Pts',(-40.9202058648666,36.9976940991033,38.4688866576175));
#25287=CARTESIAN_POINT('Ctrl Pts',(-40.9498740997176,37.0319041742421,38.5060681597608));
#25288=CARTESIAN_POINT('Ctrl Pts',(-40.9791340517388,37.0669497294479,38.5428067294934));
#25289=CARTESIAN_POINT('Ctrl Pts',(-41.0079676433999,37.1028091126999,38.579079668808));
#25290=CARTESIAN_POINT('Ctrl Pts',(-41.0368012350609,37.1386684959519,38.6153526081226));
#25291=CARTESIAN_POINT('Ctrl Pts',(-41.0652084648935,37.1753417054242,38.6511599151723));
#25292=CARTESIAN_POINT('Ctrl Pts',(-41.0931717822014,37.2128060834914,38.6864794673074));
#25293=CARTESIAN_POINT('Ctrl Pts',(-39.4346256110129,36.0919751221218,36.6944838970834));
#25294=CARTESIAN_POINT('Ctrl Pts',(-39.4725298722153,36.0992268422418,36.7400244943522));
#25295=CARTESIAN_POINT('Ctrl Pts',(-39.5103233304392,36.1075387342617,36.7854882570788));
#25296=CARTESIAN_POINT('Ctrl Pts',(-39.5479817765187,36.1169054606204,36.8308460611382));
#25297=CARTESIAN_POINT('Ctrl Pts',(-39.5856067836463,36.126263869761,36.8761635895733));
#25298=CARTESIAN_POINT('Ctrl Pts',(-39.6230970162442,36.1366752402719,36.9213753449624));
#25299=CARTESIAN_POINT('Ctrl Pts',(-39.660428502191,36.1481329029665,36.9664524162245));
#25300=CARTESIAN_POINT('Ctrl Pts',(-39.6977599881378,36.159590565661,37.0115294874866));
#25301=CARTESIAN_POINT('Ctrl Pts',(-39.7349327253984,36.1720945199135,37.0564718721653));
#25302=CARTESIAN_POINT('Ctrl Pts',(-39.7719229449465,36.1856367592142,37.101250831596));
#25303=CARTESIAN_POINT('Ctrl Pts',(-39.8089131644947,36.199178998515,37.1460297910268));
#25304=CARTESIAN_POINT('Ctrl Pts',(-39.8457208643172,36.2137595221243,37.1906453227709));
#25305=CARTESIAN_POINT('Ctrl Pts',(-39.8823225089789,36.2293689964792,37.2350688973405));
#25306=CARTESIAN_POINT('Ctrl Pts',(-39.9189241536405,36.244978470834,37.2794924719103));
#25307=CARTESIAN_POINT('Ctrl Pts',(-39.955319741146,36.2616168950825,37.323724086885));
#25308=CARTESIAN_POINT('Ctrl Pts',(-39.991485999596,36.2792736205146,37.3677354583607));
#25309=CARTESIAN_POINT('Ctrl Pts',(-40.0276522580461,36.2969303459467,37.4117468298364));
#25310=CARTESIAN_POINT('Ctrl Pts',(-40.0635891854849,36.315605371603,37.4555379554203));
#25311=CARTESIAN_POINT('Ctrl Pts',(-40.0992738033646,36.3352867472645,37.4990808329548));
#25312=CARTESIAN_POINT('Ctrl Pts',(-40.1349584212442,36.354968122926,37.5426237104893));
#25313=CARTESIAN_POINT('Ctrl Pts',(-40.170390727621,36.3756558475192,37.5859183376024));
#25314=CARTESIAN_POINT('Ctrl Pts',(-40.2055480666248,36.3973366845857,37.6289370296476));
#25315=CARTESIAN_POINT('Ctrl Pts',(-40.2407054056287,36.4190175216522,37.6719557216929));
#25316=CARTESIAN_POINT('Ctrl Pts',(-40.2755877753349,36.441691470006,37.7146984763238));
#25317=CARTESIAN_POINT('Ctrl Pts',(-40.310172871514,36.4653440238763,37.7571379617795));
#25318=CARTESIAN_POINT('Ctrl Pts',(-40.344757967693,36.4889965777465,37.7995774472352));
#25319=CARTESIAN_POINT('Ctrl Pts',(-40.3790457884594,36.5136277358433,37.8417136612032));
#25320=CARTESIAN_POINT('Ctrl Pts',(-40.4130144096595,36.5392217416009,37.8835196597081));
#25321=CARTESIAN_POINT('Ctrl Pts',(-40.4469830308596,36.5648157473584,37.925325658213));
#25322=CARTESIAN_POINT('Ctrl Pts',(-40.4806324506522,36.5913725993853,37.9668014389802));
#25323=CARTESIAN_POINT('Ctrl Pts',(-40.5139411530224,36.6188753104799,38.0079204802583));
#25324=CARTESIAN_POINT('Ctrl Pts',(-40.5472498553926,36.6463780215745,38.0490395215364));
#25325=CARTESIAN_POINT('Ctrl Pts',(-40.5802178385262,36.6748265902378,38.0898018210857));
#25326=CARTESIAN_POINT('Ctrl Pts',(-40.6128240220158,36.7042028203337,38.1301813132566));
#25327=CARTESIAN_POINT('Ctrl Pts',(-40.6454302055053,36.7335790504297,38.1705608054276));
#25328=CARTESIAN_POINT('Ctrl Pts',(-40.6776745875699,36.7638829403548,38.2105574880192));
#25329=CARTESIAN_POINT('Ctrl Pts',(-40.7095365503501,36.7950951082957,38.2501457847872));
#25330=CARTESIAN_POINT('Ctrl Pts',(-40.7413985131303,36.8263072762366,38.2897340815552));
#25331=CARTESIAN_POINT('Ctrl Pts',(-40.7728780548889,36.8584277204919,38.3289139903424));
#25332=CARTESIAN_POINT('Ctrl Pts',(-40.8039550466254,36.8914358983219,38.367660456977));
#25333=CARTESIAN_POINT('Ctrl Pts',(-40.8350320383618,36.9244440761519,38.4064069236116));
#25334=CARTESIAN_POINT('Ctrl Pts',(-40.8657064783874,36.9583399857604,38.4447199459838));
#25335=CARTESIAN_POINT('Ctrl Pts',(-40.8959587523012,36.9931019497439,38.48257502401));
#25336=CARTESIAN_POINT('Ctrl Pts',(-40.9262110262151,37.0278639137272,38.5204301020362));
#25337=CARTESIAN_POINT('Ctrl Pts',(-40.9560411323692,37.0634919301915,38.5578272336539));
#25338=CARTESIAN_POINT('Ctrl Pts',(-40.9854299960126,37.0999632147619,38.5947425041665));
#25339=CARTESIAN_POINT('Ctrl Pts',(-41.0148188596561,37.1364344993323,38.631657774679));
#25340=CARTESIAN_POINT('Ctrl Pts',(-41.0437664791875,37.1737490500216,38.6680911820752));
#25341=CARTESIAN_POINT('Ctrl Pts',(-41.0722543438753,37.2118830045948,38.7040194275986));
#25342=CARTESIAN_POINT('Ctrl Pts',(-39.3814629558515,36.0853326504592,36.6755521234339));
#25343=CARTESIAN_POINT('Ctrl Pts',(-39.4200963515739,36.0921175602388,36.7218957884221));
#25344=CARTESIAN_POINT('Ctrl Pts',(-39.4586222625692,36.1000005779042,36.7681680489437));
#25345=CARTESIAN_POINT('Ctrl Pts',(-39.497015155909,36.1089764651429,36.814338236632));
#25346=CARTESIAN_POINT('Ctrl Pts',(-39.5353739581419,36.1179443822105,36.8604674273371));
#25347=CARTESIAN_POINT('Ctrl Pts',(-39.5735999766239,36.1280032283558,36.9064947237168));
#25348=CARTESIAN_POINT('Ctrl Pts',(-39.6116679223089,36.139146336545,36.9523896741349));
#25349=CARTESIAN_POINT('Ctrl Pts',(-39.6497358679937,36.1502894447343,36.9982846245528));
#25350=CARTESIAN_POINT('Ctrl Pts',(-39.6876457386624,36.1625168143152,37.0440472263331));
#25351=CARTESIAN_POINT('Ctrl Pts',(-39.7253724546258,36.1758203444221,37.0896472031976));
#25352=CARTESIAN_POINT('Ctrl Pts',(-39.7630991705892,36.189123874529,37.1352471800621));
#25353=CARTESIAN_POINT('Ctrl Pts',(-39.8006427296317,36.2035035643805,37.1806845293466));
#25354=CARTESIAN_POINT('Ctrl Pts',(-39.8379782945584,36.2189498900012,37.2259291901463));
#25355=CARTESIAN_POINT('Ctrl Pts',(-39.8753138594851,36.234396215622,37.2711738509459));
#25356=CARTESIAN_POINT('Ctrl Pts',(-39.9124414281179,36.2509091761096,37.3162258206219));
#25357=CARTESIAN_POINT('Ctrl Pts',(-39.9493364385308,36.2684778369691,37.3610552933582));
#25358=CARTESIAN_POINT('Ctrl Pts',(-39.9862314489437,36.2860464978287,37.4058847660944));
#25359=CARTESIAN_POINT('Ctrl Pts',(-40.0228938989954,36.3046708580366,37.4504917392803));
#25360=CARTESIAN_POINT('Ctrl Pts',(-40.0592995345528,36.3243385870607,37.4948467016043));
#25361=CARTESIAN_POINT('Ctrl Pts',(-40.0957051701101,36.3440063160846,37.5392016639285));
#25362=CARTESIAN_POINT('Ctrl Pts',(-40.1318539890504,36.3647174127763,37.5833046128045));
#25363=CARTESIAN_POINT('Ctrl Pts',(-40.1677220770696,36.3864581668707,37.6271263704259));
#25364=CARTESIAN_POINT('Ctrl Pts',(-40.2035901650887,36.4081989209652,37.6709481280473));
#25365=CARTESIAN_POINT('Ctrl Pts',(-40.2391775200882,36.4309693311908,37.7144886918567));
#25366=CARTESIAN_POINT('Ctrl Pts',(-40.2744605992144,36.4547543256888,37.7577192561222));
#25367=CARTESIAN_POINT('Ctrl Pts',(-40.3097436783406,36.4785393201868,37.8009498203877));
#25368=CARTESIAN_POINT('Ctrl Pts',(-40.344722479535,36.5033388975689,37.843870382588));
#25369=CARTESIAN_POINT('Ctrl Pts',(-40.3793738624689,36.5291366442977,37.8864525471272));
#25370=CARTESIAN_POINT('Ctrl Pts',(-40.4140252454028,36.5549343910266,37.9290347116664));
#25371=CARTESIAN_POINT('Ctrl Pts',(-40.4483492080622,36.5817303055995,37.9712784760635));
#25372=CARTESIAN_POINT('Ctrl Pts',(-40.4823230432667,36.6095066545203,38.0131558924017));
#25373=CARTESIAN_POINT('Ctrl Pts',(-40.5162968784713,36.6372830034411,38.0550333087399));
#25374=CARTESIAN_POINT('Ctrl Pts',(-40.5499205842402,36.6660397850891,38.0965443745774));
#25375=CARTESIAN_POINT('Ctrl Pts',(-40.5831719165406,36.6957579694511,38.1376616266135));
#25376=CARTESIAN_POINT('Ctrl Pts',(-40.616423248841,36.7254761538132,38.1787788786495));
#25377=CARTESIAN_POINT('Ctrl Pts',(-40.6493022057342,36.7561557391554,38.2195023144866));
#25378=CARTESIAN_POINT('Ctrl Pts',(-40.6817870357346,36.7877764241078,38.2598049917394));
#25379=CARTESIAN_POINT('Ctrl Pts',(-40.714271865735,36.8193971090602,38.3001076689922));
#25380=CARTESIAN_POINT('Ctrl Pts',(-40.7463625669486,36.851958891778,38.3399895853106));
#25381=CARTESIAN_POINT('Ctrl Pts',(-40.7780379091856,36.8854402263731,38.3794243548364));
#25382=CARTESIAN_POINT('Ctrl Pts',(-40.8097132514226,36.9189215609682,38.4188591243623));
#25383=CARTESIAN_POINT('Ctrl Pts',(-40.8409732328363,36.9533224454876,38.457846744796));
#25384=CARTESIAN_POINT('Ctrl Pts',(-40.8717971725931,36.9886201180083,38.4963614216827));
#25385=CARTESIAN_POINT('Ctrl Pts',(-40.9026211123499,37.023917790529,38.5348760985694));
#25386=CARTESIAN_POINT('Ctrl Pts',(-40.9330090086526,37.0601122489923,38.572917829663));
#25387=CARTESIAN_POINT('Ctrl Pts',(-40.9629407573583,37.0971795455297,38.6104614460067));
#25388=CARTESIAN_POINT('Ctrl Pts',(-40.992872506064,37.134246842067,38.6480050623504));
#25389=CARTESIAN_POINT('Ctrl Pts',(-41.0223481054269,37.1721869745165,38.6850505617546));
#25390=CARTESIAN_POINT('Ctrl Pts',(-41.0513480545682,37.2109748407208,38.7215734340293));
#25391=CARTESIAN_POINT('Ctrl Pts',(-39.328929483429,36.0794935374574,36.6573329044902));
#25392=CARTESIAN_POINT('Ctrl Pts',(-39.368273666578,36.0857923759536,36.7044587632537));
#25393=CARTESIAN_POINT('Ctrl Pts',(-39.4075142338028,36.0932273061387,36.7515192758672));
#25394=CARTESIAN_POINT('Ctrl Pts',(-39.446624290186,36.1017932315173,36.7984821877224));
#25395=CARTESIAN_POINT('Ctrl Pts',(-39.4856996186549,36.1103515507519,36.8454033986921));
#25396=CARTESIAN_POINT('Ctrl Pts',(-39.5246446655334,36.1200388569976,36.8922271792333));
#25397=CARTESIAN_POINT('Ctrl Pts',(-39.5634327857681,36.1308485224857,36.9389214939046));
#25398=CARTESIAN_POINT('Ctrl Pts',(-39.6022209060027,36.1416581879739,36.9856158085758));
#25399=CARTESIAN_POINT('Ctrl Pts',(-39.6408520971723,36.1535902120295,37.0321806544619));
#25400=CARTESIAN_POINT('Ctrl Pts',(-39.6792999289752,36.1666364311187,37.078584173284));
#25401=CARTESIAN_POINT('Ctrl Pts',(-39.7177477607781,36.1796826502079,37.124987692106));
#25402=CARTESIAN_POINT('Ctrl Pts',(-39.7560122307984,36.1938430635127,37.1712298809617));
#25403=CARTESIAN_POINT('Ctrl Pts',(-39.7940671596448,36.2091079829044,37.2172791023278));
#25404=CARTESIAN_POINT('Ctrl Pts',(-39.8321220884911,36.2243729022961,37.2633283236939));
#25405=CARTESIAN_POINT('Ctrl Pts',(-39.8699674737866,36.2407423268217,37.3091845746951));
#25406=CARTESIAN_POINT('Ctrl Pts',(-39.9075774228251,36.258205057003,37.354816481842));
#25407=CARTESIAN_POINT('Ctrl Pts',(-39.9451873718635,36.2756677871843,37.400448388989));
#25408=CARTESIAN_POINT('Ctrl Pts',(-39.9825618823067,36.2942238219334,37.4458559494362));
#25409=CARTESIAN_POINT('Ctrl Pts',(-40.0196753836261,36.3138604657633,37.4910080966812));
#25410=CARTESIAN_POINT('Ctrl Pts',(-40.0567888849456,36.3334971095933,37.5361602439262));
#25411=CARTESIAN_POINT('Ctrl Pts',(-40.0936413748243,36.3542143612781,37.5810569751502));
#25412=CARTESIAN_POINT('Ctrl Pts',(-40.1302076398849,36.3759980466904,37.6256675733451));
#25413=CARTESIAN_POINT('Ctrl Pts',(-40.1667739049455,36.3977817321028,37.6702781715401));
#25414=CARTESIAN_POINT('Ctrl Pts',(-40.2030539428982,36.42063184988,37.7146026339187));
#25415=CARTESIAN_POINT('Ctrl Pts',(-40.2390229320341,36.4445327666565,37.7586106350066));
#25416=CARTESIAN_POINT('Ctrl Pts',(-40.27499192117,36.468433683433,37.8026186360944));
#25417=CARTESIAN_POINT('Ctrl Pts',(-40.3106498592423,36.4933853977163,37.8463101731435));
#25418=CARTESIAN_POINT('Ctrl Pts',(-40.3459723501384,36.5193708382809,37.8896553537003));
#25419=CARTESIAN_POINT('Ctrl Pts',(-40.3812948410344,36.5453562788454,37.933000534257));
#25420=CARTESIAN_POINT('Ctrl Pts',(-40.4162818825551,36.5723754440713,37.9759993556171));
#25421=CARTESIAN_POINT('Ctrl Pts',(-40.4509095376073,36.6004098482494,38.0186223992661));
#25422=CARTESIAN_POINT('Ctrl Pts',(-40.4855371926595,36.6284442524275,38.0612454429149));
#25423=CARTESIAN_POINT('Ctrl Pts',(-40.5198054590814,36.6574938938075,38.1034927061915));
#25424=CARTESIAN_POINT('Ctrl Pts',(-40.5536908915443,36.687538897489,38.145335284775));
#25425=CARTESIAN_POINT('Ctrl Pts',(-40.5875763240073,36.7175839011704,38.1871778633585));
#25426=CARTESIAN_POINT('Ctrl Pts',(-40.6210789203957,36.7486242652774,38.2286157546364));
#25427=CARTESIAN_POINT('Ctrl Pts',(-40.6541757592299,36.7806387529162,38.2696206080363));
#25428=CARTESIAN_POINT('Ctrl Pts',(-40.687272598064,36.8126532405551,38.3106254614361));
#25429=CARTESIAN_POINT('Ctrl Pts',(-40.7199636772774,36.845641849727,38.3511972743978));
#25430=CARTESIAN_POINT('Ctrl Pts',(-40.7522266306062,36.8795820106068,38.3913082888937));
#25431=CARTESIAN_POINT('Ctrl Pts',(-40.7844895839349,36.9135221714866,38.4314193033897));
#25432=CARTESIAN_POINT('Ctrl Pts',(-40.8163244093647,36.9484138819554,38.4710695169156));
#25433=CARTESIAN_POINT('Ctrl Pts',(-40.8477093264549,36.9842332701427,38.5102318019748));
#25434=CARTESIAN_POINT('Ctrl Pts',(-40.8790942435451,37.0200526583299,38.5493940870341));
#25435=CARTESIAN_POINT('Ctrl Pts',(-40.9100292503363,37.0567997219994,38.5880684411817));
#25436=CARTESIAN_POINT('Ctrl Pts',(-40.9404931820171,37.0944493199032,38.6262284045748));
#25437=CARTESIAN_POINT('Ctrl Pts',(-40.9709571136978,37.132098917807,38.664388367968));
#25438=CARTESIAN_POINT('Ctrl Pts',(-41.0009499683659,37.1706510475943,38.7020339382242));
#25439=CARTESIAN_POINT('Ctrl Pts',(-41.030451225803,37.2100793330453,38.7391393593644));
#25440=CARTESIAN_POINT('Ctrl Pts',(-39.2238625385841,36.0678153114539,36.6208944666028));
#25441=CARTESIAN_POINT('Ctrl Pts',(-39.2646282965863,36.073142007383,36.6695847129169));
#25442=CARTESIAN_POINT('Ctrl Pts',(-39.3052981762699,36.0796807626077,36.7182217297142));
#25443=CARTESIAN_POINT('Ctrl Pts',(-39.34584255874,36.0874267642663,36.7667700899032));
#25444=CARTESIAN_POINT('Ctrl Pts',(-39.3863509396808,36.0951658878348,36.8152753414023));
#25445=CARTESIAN_POINT('Ctrl Pts',(-39.4267340433523,36.104110114281,36.8636920902664));
#25446=CARTESIAN_POINT('Ctrl Pts',(-39.4669625126864,36.1142528943672,36.911985133444));
#25447=CARTESIAN_POINT('Ctrl Pts',(-39.5071909820206,36.1243956744533,36.9602781766217));
#25448=CARTESIAN_POINT('Ctrl Pts',(-39.5472648141921,36.1357370074583,37.0084475107197));
#25449=CARTESIAN_POINT('Ctrl Pts',(-39.5871548776739,36.148268604512,37.0564581134567));
#25450=CARTESIAN_POINT('Ctrl Pts',(-39.6270449411558,36.1608002015658,37.1044687161937));
#25451=CARTESIAN_POINT('Ctrl Pts',(-39.6667512331317,36.1745220617773,37.1523205841918));
#25452=CARTESIAN_POINT('Ctrl Pts',(-39.7062448898175,36.1894241687108,37.1999789266909));
#25453=CARTESIAN_POINT('Ctrl Pts',(-39.7457385465032,36.2043262756443,37.24763726919));
#25454=CARTESIAN_POINT('Ctrl Pts',(-39.7850195651239,36.220408628246,37.2951020828413));
#25455=CARTESIAN_POINT('Ctrl Pts',(-39.8240593914136,36.2376594970707,37.3423388588098));
#25456=CARTESIAN_POINT('Ctrl Pts',(-39.8630992177033,36.2549103658954,37.3895756347783));
#25457=CARTESIAN_POINT('Ctrl Pts',(-39.9018978489292,36.2733297497268,37.4365843697479));
#25458=CARTESIAN_POINT('Ctrl Pts',(-39.9404270817729,36.2929042231687,37.4833308868348));
#25459=CARTESIAN_POINT('Ctrl Pts',(-39.9789563146166,36.3124786966106,37.5300774039217));
#25460=CARTESIAN_POINT('Ctrl Pts',(-40.017216146372,36.3332082582817,37.5765616998417));
#25461=CARTESIAN_POINT('Ctrl Pts',(-40.0551787655156,36.3550778063297,37.6227499791836));
#25462=CARTESIAN_POINT('Ctrl Pts',(-40.0931413846591,36.3769473543777,37.6689382585255));
#25463=CARTESIAN_POINT('Ctrl Pts',(-40.130806788518,36.3999568872584,37.7148305180427));
#25464=CARTESIAN_POINT('Ctrl Pts',(-40.1681475976734,36.4240896485919,37.7603933927753));
#25465=CARTESIAN_POINT('Ctrl Pts',(-40.2054884068288,36.4482224099254,37.8059562675079));
#25466=CARTESIAN_POINT('Ctrl Pts',(-40.2425046186569,36.4734783980113,37.8511897542544));
#25467=CARTESIAN_POINT('Ctrl Pts',(-40.2791693254774,36.4998392262471,37.8960609668463));
#25468=CARTESIAN_POINT('Ctrl Pts',(-40.3158340322977,36.526200054483,37.9409321794382));
#25469=CARTESIAN_POINT('Ctrl Pts',(-40.352147231541,36.5536657210148,37.9854411147245));
#25470=CARTESIAN_POINT('Ctrl Pts',(-40.3880825262885,36.5822162357075,38.0295554129948));
#25471=CARTESIAN_POINT('Ctrl Pts',(-40.4240178210361,36.6107667504003,38.073669711265));
#25472=CARTESIAN_POINT('Ctrl Pts',(-40.4595752087639,36.6404021112443,38.1173893694198));
#25473=CARTESIAN_POINT('Ctrl Pts',(-40.4947288415519,36.6711007535647,38.160682601098));
#25474=CARTESIAN_POINT('Ctrl Pts',(-40.5298824743399,36.7017993958849,38.2039758327763));
#25475=CARTESIAN_POINT('Ctrl Pts',(-40.5646323497188,36.7335613175213,38.2468426349361));
#25476=CARTESIAN_POINT('Ctrl Pts',(-40.5989532062203,36.7663634105331,38.2892518406301));
#25477=CARTESIAN_POINT('Ctrl Pts',(-40.6332740627219,36.799165503545,38.331661046324));
#25478=CARTESIAN_POINT('Ctrl Pts',(-40.6671658979351,36.833007765625,38.3736126525723));
#25479=CARTESIAN_POINT('Ctrl Pts',(-40.7006040734473,36.8678655790743,38.4150761570084));
#25480=CARTESIAN_POINT('Ctrl Pts',(-40.7340422489594,36.9027233925236,38.4565396614444));
#25481=CARTESIAN_POINT('Ctrl Pts',(-40.7670267624215,36.938596754891,38.4975150611547));
#25482=CARTESIAN_POINT('Ctrl Pts',(-40.7995336341785,36.9754595744115,38.5379725625591));
#25483=CARTESIAN_POINT('Ctrl Pts',(-40.8320405059355,37.0123223939319,38.5784300639635));
#25484=CARTESIAN_POINT('Ctrl Pts',(-40.8640697337037,37.0501746680138,38.618369664219));
#25485=CARTESIAN_POINT('Ctrl Pts',(-40.8955980313347,37.0889888686504,38.6577623217111));
#25486=CARTESIAN_POINT('Ctrl Pts',(-40.9271263289655,37.1278030692871,38.6971549792031));
#25487=CARTESIAN_POINT('Ctrl Pts',(-40.9581536942437,37.1675791937501,38.7360006911634));
#25488=CARTESIAN_POINT('Ctrl Pts',(-40.9886575682726,37.2082883176943,38.7742712100345));
#25489=CARTESIAN_POINT('Ctrl Pts',(-39.1213009037391,36.0593349777119,36.5872926664368));
#25490=CARTESIAN_POINT('Ctrl Pts',(-39.1634150972342,36.0636128402979,36.6374640999373));
#25491=CARTESIAN_POINT('Ctrl Pts',(-39.2054433505444,36.0691789179925,36.6875969316031));
#25492=CARTESIAN_POINT('Ctrl Pts',(-39.2473531680651,36.0760288520249,36.7376523940249));
#25493=CARTESIAN_POINT('Ctrl Pts',(-39.2892257716136,36.0828727036338,36.7876634095199));
#25494=CARTESIAN_POINT('Ctrl Pts',(-39.3309801462962,36.0909981320292,36.8375971891504));
#25495=CARTESIAN_POINT('Ctrl Pts',(-39.3725840666773,36.100398815097,36.8874151893489));
#25496=CARTESIAN_POINT('Ctrl Pts',(-39.4141879870585,36.1097994981648,36.9372331895473));
#25497=CARTESIAN_POINT('Ctrl Pts',(-39.4556414498437,36.1204754351501,36.9869354063684));
#25498=CARTESIAN_POINT('Ctrl Pts',(-39.4969124627552,36.1324183387962,37.0364834761731));
#25499=CARTESIAN_POINT('Ctrl Pts',(-39.5381834756667,36.1443612424423,37.0860315459778));
#25500=CARTESIAN_POINT('Ctrl Pts',(-39.5792720354387,36.1575711117933,37.1354254648433));
#25501=CARTESIAN_POINT('Ctrl Pts',(-39.6201464322449,36.1720377072933,37.1846271081025));
#25502=CARTESIAN_POINT('Ctrl Pts',(-39.6610208290511,36.1865043027934,37.2338287513618));
#25503=CARTESIAN_POINT('Ctrl Pts',(-39.7016810596549,36.2022276232881,37.2828381151187));
#25504=CARTESIAN_POINT('Ctrl Pts',(-39.7420957453741,36.219195492734,37.3316173723016));
#25505=CARTESIAN_POINT('Ctrl Pts',(-39.7825104310933,36.2361633621799,37.3803966294844));
#25506=CARTESIAN_POINT('Ctrl Pts',(-39.822679568738,36.2543757792275,37.4289457762338));
#25507=CARTESIAN_POINT('Ctrl Pts',(-39.8625721590876,36.2738186501582,37.4772273412781));
#25508=CARTESIAN_POINT('Ctrl Pts',(-39.9024647494372,36.2932615210888,37.5255089063225));
#25509=CARTESIAN_POINT('Ctrl Pts',(-39.942080789334,36.3139348443555,37.5735228858394));
#25510=CARTESIAN_POINT('Ctrl Pts',(-39.9813897066777,36.335822630304,37.6212322219917));
#25511=CARTESIAN_POINT('Ctrl Pts',(-40.0206986240214,36.3577104162525,37.668941558144));
#25512=CARTESIAN_POINT('Ctrl Pts',(-40.0597004156941,36.3808126631406,37.7163462471529));
#25513=CARTESIAN_POINT('Ctrl Pts',(-40.0983649837487,36.4051115100372,37.763409701623));
#25514=CARTESIAN_POINT('Ctrl Pts',(-40.1370295518033,36.4294103569339,37.8104731560931));
#25515=CARTESIAN_POINT('Ctrl Pts',(-40.1753568931785,36.4549058019088,37.8571953722981));
#25516=CARTESIAN_POINT('Ctrl Pts',(-40.2133174303323,36.481578140267,37.9035402895529));
#25517=CARTESIAN_POINT('Ctrl Pts',(-40.2512779674861,36.5082504786252,37.9498852068076));
#25518=CARTESIAN_POINT('Ctrl Pts',(-40.2888716974199,36.5360997082516,37.9958528214448));
#25519=CARTESIAN_POINT('Ctrl Pts',(-40.3260696085235,36.5651043110576,38.0414076549687));
#25520=CARTESIAN_POINT('Ctrl Pts',(-40.3632675196271,36.5941089138638,38.0869624884926));
#25521=CARTESIAN_POINT('Ctrl Pts',(-40.4000696089563,36.6242688875483,38.1321045372966));
#25522=CARTESIAN_POINT('Ctrl Pts',(-40.4364474754407,36.6555609337657,38.1767989596455));
#25523=CARTESIAN_POINT('Ctrl Pts',(-40.4728253419251,36.686852979983,38.2214933819945));
#25524=CARTESIAN_POINT('Ctrl Pts',(-40.5087789826821,36.7192770962499,38.2657401743488));
#25525=CARTESIAN_POINT('Ctrl Pts',(-40.5442806508694,36.7528082398403,38.3095051853305));
#25526=CARTESIAN_POINT('Ctrl Pts',(-40.5797823190567,36.7863393834308,38.3532701963122));
#25527=CARTESIAN_POINT('Ctrl Pts',(-40.6148320118633,36.8209775516863,38.3965534224558));
#25528=CARTESIAN_POINT('Ctrl Pts',(-40.6494026793325,36.8566959960423,38.4393214552702));
#25529=CARTESIAN_POINT('Ctrl Pts',(-40.6839733468017,36.8924144403984,38.4820894880846));
#25530=CARTESIAN_POINT('Ctrl Pts',(-40.7180649861996,36.9292131580259,38.5243423241839));
#25531=CARTESIAN_POINT('Ctrl Pts',(-40.7516512860782,36.9670637357012,38.5660473493613));
#25532=CARTESIAN_POINT('Ctrl Pts',(-40.7852375859569,37.0049143133765,38.6077523745386));
#25533=CARTESIAN_POINT('Ctrl Pts',(-40.8183185436573,37.0438167481007,38.6489095854915));
#25534=CARTESIAN_POINT('Ctrl Pts',(-40.850868626706,37.0837410057141,38.6894872124688));
#25535=CARTESIAN_POINT('Ctrl Pts',(-40.8834187097547,37.1236652633276,38.7300648394461));
#25536=CARTESIAN_POINT('Ctrl Pts',(-40.9154379155743,37.1646113406675,38.7700628792342));
#25537=CARTESIAN_POINT('Ctrl Pts',(-40.9469015299415,37.2065476288528,38.8094504554143));
#25538=CARTESIAN_POINT('Ctrl Pts',(-39.0207460949714,36.0533905312094,36.5559457683958));
#25539=CARTESIAN_POINT('Ctrl Pts',(-39.0641468291962,36.0565585379072,36.6075281860324));
#25540=CARTESIAN_POINT('Ctrl Pts',(-39.1074736387074,36.0610908816947,36.6590890062573));
#25541=CARTESIAN_POINT('Ctrl Pts',(-39.1506910132618,36.0669838469081,36.7105859702823));
#25542=CARTESIAN_POINT('Ctrl Pts',(-39.1938700127939,36.0728715794419,36.762037207394));
#25543=CARTESIAN_POINT('Ctrl Pts',(-39.2369397677751,36.0801175176109,36.8134246970649));
#25544=CARTESIAN_POINT('Ctrl Pts',(-39.2798650412689,36.0887157332477,36.864706397297));
#25545=CARTESIAN_POINT('Ctrl Pts',(-39.3227903147626,36.0973139488844,36.9159880975291));
#25546=CARTESIAN_POINT('Ctrl Pts',(-39.3655711029354,36.1072644412216,36.9671640037434));
#25547=CARTESIAN_POINT('Ctrl Pts',(-39.4081724052227,36.1185590693907,37.0181922470333));
#25548=CARTESIAN_POINT('Ctrl Pts',(-39.45077370751,36.1298536975599,37.0692204903233));
#25549=CARTESIAN_POINT('Ctrl Pts',(-39.4931955201093,36.1424924605521,37.1201010661334));
#25550=CARTESIAN_POINT('Ctrl Pts',(-39.5354031361866,36.1564650181319,37.1707923471893));
#25551=CARTESIAN_POINT('Ctrl Pts',(-39.5776107522639,36.1704375757116,37.2214836282453));
#25552=CARTESIAN_POINT('Ctrl Pts',(-39.6196041680497,36.1857439266316,37.2719856100209));
#25553=CARTESIAN_POINT('Ctrl Pts',(-39.6613490271611,36.2023715481965,37.3222569749733));
#25554=CARTESIAN_POINT('Ctrl Pts',(-39.7030938862725,36.2189991697614,37.3725283399257));
#25555=CARTESIAN_POINT('Ctrl Pts',(-39.7445901849912,36.2369480604885,37.422569083569));
#25556=CARTESIAN_POINT('Ctrl Pts',(-39.7858039736614,36.256203535727,37.4723382657212));
#25557=CARTESIAN_POINT('Ctrl Pts',(-39.8270177623316,36.2754590109655,37.5221074478735));
#25558=CARTESIAN_POINT('Ctrl Pts',(-39.8679490372736,36.296021068996,37.5716050640911));
#25559=CARTESIAN_POINT('Ctrl Pts',(-39.9085643110985,36.3178728872391,37.6207906185448));
#25560=CARTESIAN_POINT('Ctrl Pts',(-39.9491795849234,36.3397247054822,37.6699761729984));
#25561=CARTESIAN_POINT('Ctrl Pts',(-39.9894788539988,36.3628662819846,37.718849661295));
#25562=CARTESIAN_POINT('Ctrl Pts',(-40.0294291480157,36.3872786837715,37.7673710982308));
#25563=CARTESIAN_POINT('Ctrl Pts',(-40.0693794420325,36.4116910855584,37.8158925351664));
#25564=CARTESIAN_POINT('Ctrl Pts',(-40.108980757423,36.4373743104501,37.8640619164087));
#25565=CARTESIAN_POINT('Ctrl Pts',(-40.1482006948761,36.4643073460468,37.9118398328035));
#25566=CARTESIAN_POINT('Ctrl Pts',(-40.1874206323292,36.4912403816436,37.9596177491984));
#25567=CARTESIAN_POINT('Ctrl Pts',(-40.226259188349,36.5194232255428,38.0070041964814));
#25568=CARTESIAN_POINT('Ctrl Pts',(-40.2646845876771,36.5488328203184,38.0539604060487));
#25569=CARTESIAN_POINT('Ctrl Pts',(-40.3031099870053,36.5782424150938,38.100916615616));
#25570=CARTESIAN_POINT('Ctrl Pts',(-40.3411222262111,36.6088787581198,38.147442583275));
#25571=CARTESIAN_POINT('Ctrl Pts',(-40.3786902060768,36.6407167846715,38.1935002444121));
#25572=CARTESIAN_POINT('Ctrl Pts',(-40.4162581859424,36.6725548112233,38.2395579055492));
#25573=CARTESIAN_POINT('Ctrl Pts',(-40.4533819031105,36.7055945184568,38.2851472560515));
#25574=CARTESIAN_POINT('Ctrl Pts',(-40.4900309853024,36.7398088753693,38.3302309975876));
#25575=CARTESIAN_POINT('Ctrl Pts',(-40.5266800674943,36.7740232322819,38.3753147391237));
#25576=CARTESIAN_POINT('Ctrl Pts',(-40.5628545114368,36.8094122358185,38.4198928676681));
#25577=CARTESIAN_POINT('Ctrl Pts',(-40.5985247214753,36.8459469329247,38.4639289122053));
#25578=CARTESIAN_POINT('Ctrl Pts',(-40.6341949315138,36.8824816300309,38.5079649567424));
#25579=CARTESIAN_POINT('Ctrl Pts',(-40.6693609044662,36.9201620174461,38.5514589133412));
#25580=CARTESIAN_POINT('Ctrl Pts',(-40.7039938697502,36.9589572674526,38.594375197988));
#25581=CARTESIAN_POINT('Ctrl Pts',(-40.7386268350342,36.9977525174592,38.6372914826347));
#25582=CARTESIAN_POINT('Ctrl Pts',(-40.7727267895576,37.0376626265932,38.6796300914979));
#25583=CARTESIAN_POINT('Ctrl Pts',(-40.8062658348873,37.0786549429194,38.7213563857966));
#25584=CARTESIAN_POINT('Ctrl Pts',(-40.839804880217,37.1196472592456,38.7630826800952));
#25585=CARTESIAN_POINT('Ctrl Pts',(-40.8727830133582,37.1617217791039,38.8041966561039));
#25586=CARTESIAN_POINT('Ctrl Pts',(-40.9051732536821,37.2048440797748,38.8446646769594));
#25587=CARTESIAN_POINT('Ctrl Pts',(-38.9201912862036,36.0474460847069,36.5245988703548));
#25588=CARTESIAN_POINT('Ctrl Pts',(-38.9648785611582,36.0495042355166,36.5775922721275));
#25589=CARTESIAN_POINT('Ctrl Pts',(-39.0095039268703,36.053002845397,36.6305810809114));
#25590=CARTESIAN_POINT('Ctrl Pts',(-39.0540288584583,36.0579388417914,36.6835195465397));
#25591=CARTESIAN_POINT('Ctrl Pts',(-39.0985142539742,36.0628704552501,36.7364110052682));
#25592=CARTESIAN_POINT('Ctrl Pts',(-39.142899389254,36.0692369031925,36.7892522049794));
#25593=CARTESIAN_POINT('Ctrl Pts',(-39.1871460158604,36.0770326513983,36.8419976052451));
#25594=CARTESIAN_POINT('Ctrl Pts',(-39.2313926424668,36.084828399604,36.8947430055108));
#25595=CARTESIAN_POINT('Ctrl Pts',(-39.2755007560271,36.0940534472931,36.9473926011183));
#25596=CARTESIAN_POINT('Ctrl Pts',(-39.3194323476903,36.1046997999852,36.9999010178936));
#25597=CARTESIAN_POINT('Ctrl Pts',(-39.3633639393533,36.1153461526773,37.0524094346688));
#25598=CARTESIAN_POINT('Ctrl Pts',(-39.4071190047799,36.1274138093109,37.1047766674234));
#25599=CARTESIAN_POINT('Ctrl Pts',(-39.4506598401283,36.1408923289704,37.1569575862761));
#25600=CARTESIAN_POINT('Ctrl Pts',(-39.4942006754768,36.1543708486299,37.2091385051288));
#25601=CARTESIAN_POINT('Ctrl Pts',(-39.5375272764445,36.1692602299752,37.2611331049231));
#25602=CARTESIAN_POINT('Ctrl Pts',(-39.5806023089482,36.185547603659,37.3128965776451));
#25603=CARTESIAN_POINT('Ctrl Pts',(-39.6236773414518,36.2018349773427,37.3646600503671));
#25604=CARTESIAN_POINT('Ctrl Pts',(-39.6665008012444,36.2195203417495,37.4161923909043));
#25605=CARTESIAN_POINT('Ctrl Pts',(-39.7090357882352,36.2385884212958,37.4674491901644));
#25606=CARTESIAN_POINT('Ctrl Pts',(-39.7515707752261,36.2576565008421,37.5187059894245));
#25607=CARTESIAN_POINT('Ctrl Pts',(-39.7938172852132,36.2781072936366,37.5696872423429));
#25608=CARTESIAN_POINT('Ctrl Pts',(-39.8357389155194,36.2999231441743,37.6203490150978));
#25609=CARTESIAN_POINT('Ctrl Pts',(-39.8776605458256,36.3217389947119,37.6710107878528));
#25610=CARTESIAN_POINT('Ctrl Pts',(-39.9192572923035,36.3449199008286,37.7213530754372));
#25611=CARTESIAN_POINT('Ctrl Pts',(-39.9604933122826,36.3694458575057,37.7713324948385));
#25612=CARTESIAN_POINT('Ctrl Pts',(-40.0017293322618,36.3939718141829,37.8213119142398));
#25613=CARTESIAN_POINT('Ctrl Pts',(-40.0426046216675,36.4198428189912,37.8709284605194));
#25614=CARTESIAN_POINT('Ctrl Pts',(-40.0830839594199,36.4470365518267,37.9201393760542));
#25615=CARTESIAN_POINT('Ctrl Pts',(-40.1235632971723,36.474230284662,37.969350291589));
#25616=CARTESIAN_POINT('Ctrl Pts',(-40.163646679278,36.5027467428342,38.018155571518));
#25617=CARTESIAN_POINT('Ctrl Pts',(-40.2032995668307,36.5325613295791,38.0665131571287));
#25618=CARTESIAN_POINT('Ctrl Pts',(-40.2429524543834,36.562375916324,38.1148707427393));
#25619=CARTESIAN_POINT('Ctrl Pts',(-40.2821748434659,36.5934886286912,38.1627806292535));
#25620=CARTESIAN_POINT('Ctrl Pts',(-40.3209329367128,36.6258726355774,38.2102015291787));
#25621=CARTESIAN_POINT('Ctrl Pts',(-40.3596910299596,36.6582566424635,38.257622429104));
#25622=CARTESIAN_POINT('Ctrl Pts',(-40.3979848235389,36.6919119406636,38.3045543377541));
#25623=CARTESIAN_POINT('Ctrl Pts',(-40.4357813197353,36.7268095108983,38.3509568098446));
#25624=CARTESIAN_POINT('Ctrl Pts',(-40.4735778159318,36.7617070811331,38.397359281935));
#25625=CARTESIAN_POINT('Ctrl Pts',(-40.5108770110103,36.7978469199508,38.4432323128804));
#25626=CARTESIAN_POINT('Ctrl Pts',(-40.5476467636181,36.8351978698072,38.4885363691403));
#25627=CARTESIAN_POINT('Ctrl Pts',(-40.584416516226,36.8725488196634,38.5338404254003));
#25628=CARTESIAN_POINT('Ctrl Pts',(-40.6206568227329,36.9111108768664,38.5785755024985));
#25629=CARTESIAN_POINT('Ctrl Pts',(-40.6563364534222,36.9508507992041,38.6227030466147));
#25630=CARTESIAN_POINT('Ctrl Pts',(-40.6920160841115,36.9905907215418,38.6668305907309));
#25631=CARTESIAN_POINT('Ctrl Pts',(-40.727135035458,37.0315085050857,38.7103505975043));
#25632=CARTESIAN_POINT('Ctrl Pts',(-40.7616630430686,37.0735688801247,38.7532255591243));
#25633=CARTESIAN_POINT('Ctrl Pts',(-40.7961910506793,37.1156292551636,38.7961005207444));
#25634=CARTESIAN_POINT('Ctrl Pts',(-40.8301281111422,37.1588322175403,38.8383304329737));
#25635=CARTESIAN_POINT('Ctrl Pts',(-40.8634449774227,37.2031405306967,38.8798788985044));
#25636=CARTESIAN_POINT('Ctrl Pts',(-38.8216486787866,36.0440450754439,36.4955134247666));
#25637=CARTESIAN_POINT('Ctrl Pts',(-38.8675604854068,36.0449321771633,36.5498474686122));
#25638=CARTESIAN_POINT('Ctrl Pts',(-38.9134244761254,36.047335827461,36.6041963012607));
#25639=CARTESIAN_POINT('Ctrl Pts',(-38.9591989734608,36.0512537858363,36.6585105300504));
#25640=CARTESIAN_POINT('Ctrl Pts',(-39.0049328251677,36.0551682652464,36.7127765303266));
#25641=CARTESIAN_POINT('Ctrl Pts',(-39.0505773373462,36.0605943642153,36.7670079822283));
#25642=CARTESIAN_POINT('Ctrl Pts',(-39.0960911068884,36.0675271092293,36.8211556889297));
#25643=CARTESIAN_POINT('Ctrl Pts',(-39.1416048764306,36.0744598542433,36.8753033956312));
#25644=CARTESIAN_POINT('Ctrl Pts',(-39.1869878983544,36.0828992445309,36.929367351204));
#25645=CARTESIAN_POINT('Ctrl Pts',(-39.2321990079216,36.0928375767059,36.9832985122337));
#25646=CARTESIAN_POINT('Ctrl Pts',(-39.2774101174888,36.1027759088809,37.0372296732634));
#25647=CARTESIAN_POINT('Ctrl Pts',(-39.3224493097507,36.1142131818435,37.0910280338458));
#25648=CARTESIAN_POINT('Ctrl Pts',(-39.3672757328278,36.127138976372,37.1446447927315));
#25649=CARTESIAN_POINT('Ctrl Pts',(-39.412102155905,36.1400647709004,37.1982615516173));
#25650=CARTESIAN_POINT('Ctrl Pts',(-39.456715804891,36.1544790855687,37.2516967029369));
#25651=CARTESIAN_POINT('Ctrl Pts',(-39.5010762146839,36.170368804263,37.3049017759191));
#25652=CARTESIAN_POINT('Ctrl Pts',(-39.5454366244767,36.1862585229573,37.3581068489013));
#25653=CARTESIAN_POINT('Ctrl Pts',(-39.5895437902214,36.2036236439281,37.411081837722));
#25654=CARTESIAN_POINT('Ctrl Pts',(-39.6333577068124,36.2224483779869,37.463778689801));
#25655=CARTESIAN_POINT('Ctrl Pts',(-39.6771716234035,36.2412731120458,37.51647554188));
#25656=CARTESIAN_POINT('Ctrl Pts',(-39.7206922860459,36.2615574571228,37.568894251449));
#25657=CARTESIAN_POINT('Ctrl Pts',(-39.763880222015,36.2832829796017,37.6209872710733));
#25658=CARTESIAN_POINT('Ctrl Pts',(-39.8070681579841,36.3050085020806,37.6730802906977));
#25659=CARTESIAN_POINT('Ctrl Pts',(-39.8499233625534,36.3281751995749,37.7248476146753));
#25660=CARTESIAN_POINT('Ctrl Pts',(-39.8924069668004,36.3527620274664,37.7762422867567));
#25661=CARTESIAN_POINT('Ctrl Pts',(-39.9348905710474,36.3773488553579,37.8276369588381));
#25662=CARTESIAN_POINT('Ctrl Pts',(-39.9770025703228,36.4033558109476,37.8786589733977));
#25663=CARTESIAN_POINT('Ctrl Pts',(-40.0187047698331,36.4307592767579,37.9292620503397));
#25664=CARTESIAN_POINT('Ctrl Pts',(-40.0604069693434,36.4581627425682,37.9798651272818));
#25665=CARTESIAN_POINT('Ctrl Pts',(-40.1016993645249,36.4869627155928,38.0300492610674));
#25666=CARTESIAN_POINT('Ctrl Pts',(-40.1425445038216,36.5171330482867,38.0797689315001));
#25667=CARTESIAN_POINT('Ctrl Pts',(-40.1833896431183,36.5473033809806,38.1294886019328));
#25668=CARTESIAN_POINT('Ctrl Pts',(-40.2237875220601,36.5788440700355,38.1787438035703));
#25669=CARTESIAN_POINT('Ctrl Pts',(-40.2637015000916,36.6117264852023,38.2274898584855));
#25670=CARTESIAN_POINT('Ctrl Pts',(-40.3036154781231,36.6446089003691,38.2762359134006));
#25671=CARTESIAN_POINT('Ctrl Pts',(-40.3430455508759,36.6788330380435,38.3244728162577));
#25672=CARTESIAN_POINT('Ctrl Pts',(-40.381955955092,36.7143678371214,38.372156812246));
#25673=CARTESIAN_POINT('Ctrl Pts',(-40.420866359308,36.7499026361994,38.4198408082342));
#25674=CARTESIAN_POINT('Ctrl Pts',(-40.4592570907285,36.7867480927872,38.4669718921339));
#25675=CARTESIAN_POINT('Ctrl Pts',(-40.4970933281026,36.8248707711673,38.5135073114282));
#25676=CARTESIAN_POINT('Ctrl Pts',(-40.5349295654766,36.8629934495474,38.5600427307225));
#25677=CARTESIAN_POINT('Ctrl Pts',(-40.5722113046629,36.9023933455436,38.6059824803173));
#25678=CARTESIAN_POINT('Ctrl Pts',(-40.6089047294248,36.9430347093574,38.6512848873549));
#25679=CARTESIAN_POINT('Ctrl Pts',(-40.6455981541867,36.9836760731712,38.6965872943927));
#25680=CARTESIAN_POINT('Ctrl Pts',(-40.6817032605078,37.0255589003514,38.7412523539138));
#25681=CARTESIAN_POINT('Ctrl Pts',(-40.7171872983561,37.068645191732,38.7852395481339));
#25682=CARTESIAN_POINT('Ctrl Pts',(-40.7526713362044,37.1117314831127,38.8292267423539));
#25683=CARTESIAN_POINT('Ctrl Pts',(-40.7875343016955,37.1560212339757,38.872536066457));
#25684=CARTESIAN_POINT('Ctrl Pts',(-40.8217445702653,37.201474264566,38.9151282310574));
#25685=CARTESIAN_POINT('Ctrl Pts',(-38.7247757052312,36.0427370989735,36.4682927109237));
#25686=CARTESIAN_POINT('Ctrl Pts',(-38.7718578692351,36.0424028155446,36.5239060150788));
#25687=CARTESIAN_POINT('Ctrl Pts',(-38.8189082888934,36.043660957969,36.5795557599548));
#25688=CARTESIAN_POINT('Ctrl Pts',(-38.8658820090438,36.0465103227804,36.6351887739484));
#25689=CARTESIAN_POINT('Ctrl Pts',(-38.9128140187114,36.0493571574882,36.6907723884083));
#25690=CARTESIAN_POINT('Ctrl Pts',(-38.9596694593267,36.0537923896288,36.74633929494));
#25691=CARTESIAN_POINT('Ctrl Pts',(-39.0064036414297,36.0598117889971,36.8018364953211));
#25692=CARTESIAN_POINT('Ctrl Pts',(-39.0531378235326,36.0658311883654,36.8573336957021));
#25693=CARTESIAN_POINT('Ctrl Pts',(-39.099750741452,36.0734347542309,36.912761183198));
#25694=CARTESIAN_POINT('Ctrl Pts',(-39.1461979370387,36.0826152345168,36.9680660925603));
#25695=CARTESIAN_POINT('Ctrl Pts',(-39.1926451326255,36.0917957148027,37.0233710019225));
#25696=CARTESIAN_POINT('Ctrl Pts',(-39.2389266002433,36.102553108395,37.0785533264399));
#25697=CARTESIAN_POINT('Ctrl Pts',(-39.2849981978721,36.1148771551806,37.133560434694));
#25698=CARTESIAN_POINT('Ctrl Pts',(-39.3310697955009,36.1272012019662,37.1885675429481));
#25699=CARTESIAN_POINT('Ctrl Pts',(-39.3769315175499,36.1410919004496,37.2433994282638));
#25700=CARTESIAN_POINT('Ctrl Pts',(-39.4225396223406,36.156536002056,37.298003793462));
#25701=CARTESIAN_POINT('Ctrl Pts',(-39.4681477271312,36.1719801036622,37.3526081586602));
#25702=CARTESIAN_POINT('Ctrl Pts',(-39.513502209129,36.1889776065172,37.4069849971147));
#25703=CARTESIAN_POINT('Ctrl Pts',(-39.5585598104479,36.2075122988592,37.4610824456581));
#25704=CARTESIAN_POINT('Ctrl Pts',(-39.6036174117667,36.2260469912013,37.5151798942014));
#25705=CARTESIAN_POINT('Ctrl Pts',(-39.6483781269388,36.2461188707815,37.5689979462689));
#25706=CARTESIAN_POINT('Ctrl Pts',(-39.6927992643964,36.2677087935801,37.6224852716482));
#25707=CARTESIAN_POINT('Ctrl Pts',(-39.737220401854,36.2892987163787,37.6759725970276));
#25708=CARTESIAN_POINT('Ctrl Pts',(-39.7813019562067,36.3124066797758,37.7291291892284));
#25709=CARTESIAN_POINT('Ctrl Pts',(-39.8250018836525,36.3370106440169,37.7819043489209));
#25710=CARTESIAN_POINT('Ctrl Pts',(-39.8687018110983,36.3616146082581,37.8346795086135));
#25711=CARTESIAN_POINT('Ctrl Pts',(-39.9120201063341,36.3877145703575,37.8870732293937));
#25712=CARTESIAN_POINT('Ctrl Pts',(-39.9549154535338,36.4152856368725,37.9390355395383));
#25713=CARTESIAN_POINT('Ctrl Pts',(-39.9978108007334,36.4428567033876,37.9909978496829));
#25714=CARTESIAN_POINT('Ctrl Pts',(-40.0402831946916,36.4718988709725,38.0425287428864));
#25715=CARTESIAN_POINT('Ctrl Pts',(-40.0822921263801,36.5023844399883,38.0935790703672));
#25716=CARTESIAN_POINT('Ctrl Pts',(-40.1243010580686,36.532870009004,38.144629397848));
#25717=CARTESIAN_POINT('Ctrl Pts',(-40.1658465223896,36.5647989757511,38.1951991534113));
#25718=CARTESIAN_POINT('Ctrl Pts',(-40.2068888943955,36.598140887239,38.2452401049829));
#25719=CARTESIAN_POINT('Ctrl Pts',(-40.2479312664015,36.6314827987268,38.2952810565544));
#25720=CARTESIAN_POINT('Ctrl Pts',(-40.2884705411118,36.6662376509092,38.3447931980618));
#25721=CARTESIAN_POINT('Ctrl Pts',(-40.3284680532555,36.7023722955423,38.3937293061547));
#25722=CARTESIAN_POINT('Ctrl Pts',(-40.3684655653993,36.7385069401753,38.4426654142476));
#25723=CARTESIAN_POINT('Ctrl Pts',(-40.4079213101227,36.7760213728738,38.4910254829877));
#25724=CARTESIAN_POINT('Ctrl Pts',(-40.4467976555966,36.8148798133799,38.5387633878407));
#25725=CARTESIAN_POINT('Ctrl Pts',(-40.4856740010705,36.8537382538859,38.5865012926936));
#25726=CARTESIAN_POINT('Ctrl Pts',(-40.5239709425773,36.8939406974841,38.6336170278665));
#25727=CARTESIAN_POINT('Ctrl Pts',(-40.561651953523,36.9354488001637,38.680065655637));
#25728=CARTESIAN_POINT('Ctrl Pts',(-40.5993329644687,36.9769569028435,38.7265142834075));
#25729=CARTESIAN_POINT('Ctrl Pts',(-40.6363980402809,37.0197706595677,38.7722957981391));
#25730=CARTESIAN_POINT('Ctrl Pts',(-40.6728118292859,37.0638492357256,38.817366534653));
#25731=CARTESIAN_POINT('Ctrl Pts',(-40.709225618291,37.1079278118835,38.862437271167));
#25732=CARTESIAN_POINT('Ctrl Pts',(-40.7449881160701,37.1532712021262,38.9067972239939));
#25733=CARTESIAN_POINT('Ctrl Pts',(-40.7800652133139,37.1998361591463,38.9504040838028));
#25734=CARTESIAN_POINT('Ctrl Pts',(-38.6279027316758,36.0414291225031,36.4410719970808));
#25735=CARTESIAN_POINT('Ctrl Pts',(-38.6761552530635,36.0398734539259,36.4979645615455));
#25736=CARTESIAN_POINT('Ctrl Pts',(-38.7243921016613,36.039986088477,36.5549152186491));
#25737=CARTESIAN_POINT('Ctrl Pts',(-38.7725650446267,36.0417668597245,36.6118670178464));
#25738=CARTESIAN_POINT('Ctrl Pts',(-38.8206952122552,36.0435460497299,36.66876824649));
#25739=CARTESIAN_POINT('Ctrl Pts',(-38.8687615813073,36.0469904150423,36.7256706076517));
#25740=CARTESIAN_POINT('Ctrl Pts',(-38.916716175971,36.0520964687649,36.7825173017124));
#25741=CARTESIAN_POINT('Ctrl Pts',(-38.9646707706347,36.0572025224874,36.8393639957731));
#25742=CARTESIAN_POINT('Ctrl Pts',(-39.0125135845495,36.063970263931,36.896155015192));
#25743=CARTESIAN_POINT('Ctrl Pts',(-39.0601968661558,36.0723928923278,36.9528336728868));
#25744=CARTESIAN_POINT('Ctrl Pts',(-39.1078801477621,36.0808155207247,37.0095123305816));
#25745=CARTESIAN_POINT('Ctrl Pts',(-39.1554038907358,36.0908930349464,37.066078619034));
#25746=CARTESIAN_POINT('Ctrl Pts',(-39.2027206629163,36.1026153339892,37.1224760766564));
#25747=CARTESIAN_POINT('Ctrl Pts',(-39.2500374350968,36.114337633032,37.1788735342789));
#25748=CARTESIAN_POINT('Ctrl Pts',(-39.2971472302088,36.1277047153306,37.2351021535907));
#25749=CARTESIAN_POINT('Ctrl Pts',(-39.3440030299973,36.1427031998488,37.2911058110049));
#25750=CARTESIAN_POINT('Ctrl Pts',(-39.3908588297857,36.1577016843671,37.347109468419));
#25751=CARTESIAN_POINT('Ctrl Pts',(-39.4374606280368,36.1743315691062,37.4028881565074));
#25752=CARTESIAN_POINT('Ctrl Pts',(-39.4837619140834,36.1925762197316,37.4583862015151));
#25753=CARTESIAN_POINT('Ctrl Pts',(-39.5300632001299,36.210820870357,37.5138842465228));
#25754=CARTESIAN_POINT('Ctrl Pts',(-39.5760639678317,36.2306802844402,37.5691016410887));
#25755=CARTESIAN_POINT('Ctrl Pts',(-39.6217183067778,36.2521346075585,37.6239832722232));
#25756=CARTESIAN_POINT('Ctrl Pts',(-39.667372645724,36.2735889306768,37.6788649033576));
#25757=CARTESIAN_POINT('Ctrl Pts',(-39.7126805498601,36.2966381599766,37.7334107637814));
#25758=CARTESIAN_POINT('Ctrl Pts',(-39.7575968005046,36.3212592605674,37.7875664110852));
#25759=CARTESIAN_POINT('Ctrl Pts',(-39.8025130511491,36.3458803611583,37.8417220583889));
#25760=CARTESIAN_POINT('Ctrl Pts',(-39.8470376423455,36.3720733297673,37.8954874853898));
#25761=CARTESIAN_POINT('Ctrl Pts',(-39.8911261372345,36.3998119969872,37.948809028737));
#25762=CARTESIAN_POINT('Ctrl Pts',(-39.9352146321234,36.427550664207,38.0021305720841));
#25763=CARTESIAN_POINT('Ctrl Pts',(-39.9788670248583,36.4568350263522,38.0550082247054));
#25764=CARTESIAN_POINT('Ctrl Pts',(-40.0220397489386,36.4876358316899,38.1073892092343));
#25765=CARTESIAN_POINT('Ctrl Pts',(-40.0652124730189,36.5184366370274,38.1597701937633));
#25766=CARTESIAN_POINT('Ctrl Pts',(-40.1079055227192,36.5507538814668,38.2116545032524));
#25767=CARTESIAN_POINT('Ctrl Pts',(-40.1500762886995,36.5845552892756,38.2629903514803));
#25768=CARTESIAN_POINT('Ctrl Pts',(-40.1922470546799,36.6183566970844,38.3143261997082));
#25769=CARTESIAN_POINT('Ctrl Pts',(-40.2338955313476,36.6536422637751,38.3651135798659));
#25770=CARTESIAN_POINT('Ctrl Pts',(-40.2749801514191,36.6903767539631,38.4153018000635));
#25771=CARTESIAN_POINT('Ctrl Pts',(-40.3160647714905,36.7271112441511,38.4654900202611));
#25772=CARTESIAN_POINT('Ctrl Pts',(-40.3565855295169,36.7652946529604,38.5150790738416));
#25773=CARTESIAN_POINT('Ctrl Pts',(-40.3965019830907,36.8048888555924,38.5640194642532));
#25774=CARTESIAN_POINT('Ctrl Pts',(-40.4364184366645,36.8444830582244,38.6129598546648));
#25775=CARTESIAN_POINT('Ctrl Pts',(-40.4757305804917,36.8854880494245,38.6612515754158));
#25776=CARTESIAN_POINT('Ctrl Pts',(-40.5143991776212,36.9278628909701,38.7088464239191));
#25777=CARTESIAN_POINT('Ctrl Pts',(-40.5530677747507,36.9702377325157,38.7564412724223));
#25778=CARTESIAN_POINT('Ctrl Pts',(-40.5910928200539,37.013982418784,38.8033392423644));
#25779=CARTESIAN_POINT('Ctrl Pts',(-40.6284363602157,37.0590532797192,38.8494935211722));
#25780=CARTESIAN_POINT('Ctrl Pts',(-40.6657799003775,37.1041241406544,38.89564779998));
#25781=CARTESIAN_POINT('Ctrl Pts',(-40.7024419304448,37.1505211702767,38.9410583815309));
#25782=CARTESIAN_POINT('Ctrl Pts',(-40.7383858563626,37.1981980537265,38.9856799365482));
#25783=CARTESIAN_POINT('Ctrl Pts',(-38.5327022782564,36.042218146015,36.4157194736928));
#25784=CARTESIAN_POINT('Ctrl Pts',(-38.582070920586,36.0393906665048,36.4738298424583));
#25785=CARTESIAN_POINT('Ctrl Pts',(-38.6314419402381,36.0383071559065,36.5320222263094));
#25786=CARTESIAN_POINT('Ctrl Pts',(-38.6807637016069,36.0389686897623,36.5902357592848));
#25787=CARTESIAN_POINT('Ctrl Pts',(-38.7300416675413,36.0396296362069,36.6483976013454));
#25788=CARTESIAN_POINT('Ctrl Pts',(-38.7792704554811,36.0420325293332,36.7065805465471));
#25789=CARTESIAN_POINT('Ctrl Pts',(-38.8283986715219,36.0461748081124,36.7647238488323));
#25790=CARTESIAN_POINT('Ctrl Pts',(-38.8775268875627,36.0503170868915,36.8228671511175));
#25791=CARTESIAN_POINT('Ctrl Pts',(-38.9265545245766,36.0561987507077,36.8809708020488));
#25792=CARTESIAN_POINT('Ctrl Pts',(-38.9754304000649,36.0638136102815,36.9389741400892));
#25793=CARTESIAN_POINT('Ctrl Pts',(-39.0243062755532,36.0714284698554,36.9969774781296));
#25794=CARTESIAN_POINT('Ctrl Pts',(-39.0730303824243,36.0807765240684,37.0548804948621));
#25795=CARTESIAN_POINT('Ctrl Pts',(-39.1215518562211,36.0918479683989,37.1126227396887));
#25796=CARTESIAN_POINT('Ctrl Pts',(-39.1700733300179,36.1029194127294,37.1703649845152));
#25797=CARTESIAN_POINT('Ctrl Pts',(-39.2183921637013,36.1157142455581,37.2279464490573));
#25798=CARTESIAN_POINT('Ctrl Pts',(-39.2664579168746,36.1302190676599,37.2853070196423));
#25799=CARTESIAN_POINT('Ctrl Pts',(-39.3145236700479,36.1447238897616,37.3426675902273));
#25800=CARTESIAN_POINT('Ctrl Pts',(-39.3623363357353,36.1609386990197,37.3998072585318));
#25801=CARTESIAN_POINT('Ctrl Pts',(-39.4098460026943,36.1788465295219,37.4566663730815));
#25802=CARTESIAN_POINT('Ctrl Pts',(-39.4573556696534,36.1967543600241,37.5135254876311));
#25803=CARTESIAN_POINT('Ctrl Pts',(-39.5045623309918,36.2163552091614,37.5701040401762));
#25804=CARTESIAN_POINT('Ctrl Pts',(-39.5514167086316,36.2376285797793,37.6263429657525));
#25805=CARTESIAN_POINT('Ctrl Pts',(-39.5982710862714,36.2589019503972,37.6825818913288));
#25806=CARTESIAN_POINT('Ctrl Pts',(-39.6447731734175,36.2818478393999,37.7384811817772));
#25807=CARTESIAN_POINT('Ctrl Pts',(-39.6908744278377,36.3064422611834,37.7939824817302));
#25808=CARTESIAN_POINT('Ctrl Pts',(-39.7369756822578,36.3310366829669,37.8494837816833));
#25809=CARTESIAN_POINT('Ctrl Pts',(-39.7826760972645,36.3572796339542,37.9045870830887));
#25810=CARTESIAN_POINT('Ctrl Pts',(-39.8279279676327,36.3851436901509,37.959234861785));
#25811=CARTESIAN_POINT('Ctrl Pts',(-39.873179838001,36.4130077463476,38.0138826404814));
#25812=CARTESIAN_POINT('Ctrl Pts',(-39.917983157166,36.4424929037033,38.0680748885401));
#25813=CARTESIAN_POINT('Ctrl Pts',(-39.9622911563025,36.4735683570419,38.1217550328776));
#25814=CARTESIAN_POINT('Ctrl Pts',(-40.0065991554391,36.5046438103804,38.1754351772151));
#25815=CARTESIAN_POINT('Ctrl Pts',(-40.0504118281197,36.5373095551866,38.2286032100432));
#25816=CARTESIAN_POINT('Ctrl Pts',(-40.0936834393859,36.5715314693577,38.2812036272513));
#25817=CARTESIAN_POINT('Ctrl Pts',(-40.136955050652,36.6057533835288,38.3338040444593));
#25818=CARTESIAN_POINT('Ctrl Pts',(-40.1796855942259,36.641531462094,38.3858368384154));
#25819=CARTESIAN_POINT('Ctrl Pts',(-40.2218304643064,36.6788283371755,38.4372476896451));
#25820=CARTESIAN_POINT('Ctrl Pts',(-40.263975334387,36.7161252122571,38.4886585408747));
#25821=CARTESIAN_POINT('Ctrl Pts',(-40.3055345248605,36.754940878439,38.5394474419187));
#25822=CARTESIAN_POINT('Ctrl Pts',(-40.346464652041,36.7952347999842,38.589561371138));
#25823=CARTESIAN_POINT('Ctrl Pts',(-40.3873947792216,36.8355287215294,38.6396753003573));
#25824=CARTESIAN_POINT('Ctrl Pts',(-40.4276958371702,36.8773008925874,38.6891142504804));
#25825=CARTESIAN_POINT('Ctrl Pts',(-40.4673257547153,36.9205076940649,38.737826608198));
#25826=CARTESIAN_POINT('Ctrl Pts',(-40.5069556722604,36.9637144955425,38.7865389659155));
#25827=CARTESIAN_POINT('Ctrl Pts',(-40.5459144436521,37.0083559211679,38.8345247241592));
#25828=CARTESIAN_POINT('Ctrl Pts',(-40.5841613979055,37.0543853594171,38.8817337855118));
#25829=CARTESIAN_POINT('Ctrl Pts',(-40.6224083521588,37.1004147976663,38.9289428468643));
#25830=CARTESIAN_POINT('Ctrl Pts',(-40.6599434837245,37.147832241859,38.9753752044751));
#25831=CARTESIAN_POINT('Ctrl Pts',(-40.6967276065595,37.1965881851941,39.0209823812249));
#25832=CARTESIAN_POINT('Ctrl Pts',(-38.4389275238392,36.0447816639384,36.3919506587633));
#25833=CARTESIAN_POINT('Ctrl Pts',(-38.4893637622182,36.0406398859262,36.4512238512357));
#25834=CARTESIAN_POINT('Ctrl Pts',(-38.539822323781,36.0383173783364,36.5106051639133));
#25835=CARTESIAN_POINT('Ctrl Pts',(-38.5902480567288,36.0378166779306,36.5700296922399));
#25836=CARTESIAN_POINT('Ctrl Pts',(-38.6406290139668,36.0373164221236,36.6294014543442));
#25837=CARTESIAN_POINT('Ctrl Pts',(-38.6909771928631,36.0386347396562,36.6888163459556));
#25838=CARTESIAN_POINT('Ctrl Pts',(-38.74123765991,36.0417701921486,36.7482095411327));
#25839=CARTESIAN_POINT('Ctrl Pts',(-38.7914981269569,36.044905644641,36.8076027363098));
#25840=CARTESIAN_POINT('Ctrl Pts',(-38.8416708741728,36.0498582315951,36.8669742256202));
#25841=CARTESIAN_POINT('Ctrl Pts',(-38.8917011594712,36.0566225493811,36.9262592304807));
#25842=CARTESIAN_POINT('Ctrl Pts',(-38.9417314447696,36.063386867167,36.9855442353412));
#25843=CARTESIAN_POINT('Ctrl Pts',(-38.9916192602048,36.0719629147108,37.0447427463364));
#25844=CARTESIAN_POINT('Ctrl Pts',(-39.0413101745598,36.0823413349242,37.1037901736122));
#25845=CARTESIAN_POINT('Ctrl Pts',(-39.0910010889149,36.0927197551375,37.1628376008879));
#25846=CARTESIAN_POINT('Ctrl Pts',(-39.1404950942985,36.1049005463721,37.2217339350668));
#25847=CARTESIAN_POINT('Ctrl Pts',(-39.1897381891798,36.1188704185053,37.2804149159938));
#25848=CARTESIAN_POINT('Ctrl Pts',(-39.2389812840611,36.1328402906386,37.3390958969207));
#25849=CARTESIAN_POINT('Ctrl Pts',(-39.287973460617,36.1485992414516,37.3975615152759));
#25850=CARTESIAN_POINT('Ctrl Pts',(-39.3366612648428,36.1661300767903,37.4557479808452));
#25851=CARTESIAN_POINT('Ctrl Pts',(-39.3853490690688,36.1836609121289,37.5139344464145));
#25852=CARTESIAN_POINT('Ctrl Pts',(-39.4337324932325,36.2029636292092,37.5718417499571));
#25853=CARTESIAN_POINT('Ctrl Pts',(-39.4817587475222,36.224017167372,37.6294067104208));
#25854=CARTESIAN_POINT('Ctrl Pts',(-39.5297850018119,36.2450707055347,37.6869716708845));
#25855=CARTESIAN_POINT('Ctrl Pts',(-39.5774540786024,36.2678750614369,37.7441942791276));
#25856=CARTESIAN_POINT('Ctrl Pts',(-39.6247139674825,36.2924053538775,37.8010121011491));
#25857=CARTESIAN_POINT('Ctrl Pts',(-39.6719738563627,36.3169356463181,37.8578299231705));
#25858=CARTESIAN_POINT('Ctrl Pts',(-39.7188245498275,36.3431918714014,37.914242949947));
#25859=CARTESIAN_POINT('Ctrl Pts',(-39.7652149303884,36.3711453816896,37.9701896307907));
#25860=CARTESIAN_POINT('Ctrl Pts',(-39.8116053109493,36.3990988919778,38.0261363116345));
#25861=CARTESIAN_POINT('Ctrl Pts',(-39.8575353712387,36.4287496830316,38.0816166376605));
#25862=CARTESIAN_POINT('Ctrl Pts',(-39.9029549982392,36.4600654036945,38.1365700758237));
#25863=CARTESIAN_POINT('Ctrl Pts',(-39.9483746252396,36.4913811243574,38.1915235139868));
#25864=CARTESIAN_POINT('Ctrl Pts',(-39.9932838117383,36.5243617696561,38.2459500555599));
#25865=CARTESIAN_POINT('Ctrl Pts',(-40.0376335585701,36.5589713553244,38.299790317254));
#25866=CARTESIAN_POINT('Ctrl Pts',(-40.0819833054019,36.5935809409928,38.353630578948));
#25867=CARTESIAN_POINT('Ctrl Pts',(-40.1257736055232,36.6298194615343,38.4068845522123));
#25868=CARTESIAN_POINT('Ctrl Pts',(-40.1689566805506,36.6676473781038,38.4594941331138));
#25869=CARTESIAN_POINT('Ctrl Pts',(-40.2121397555781,36.7054752946732,38.5121037140154));
#25870=CARTESIAN_POINT('Ctrl Pts',(-40.2547155986539,36.7448926012632,38.5640688941992));
#25871=CARTESIAN_POINT('Ctrl Pts',(-40.2966377564584,36.7858562907448,38.615332975899));
#25872=CARTESIAN_POINT('Ctrl Pts',(-40.3385599142629,36.8268199802263,38.6665970575989));
#25873=CARTESIAN_POINT('Ctrl Pts',(-40.3798283801375,36.8693300460936,38.7171600326734));
#25874=CARTESIAN_POINT('Ctrl Pts',(-40.4203981272041,36.913340106793,38.7669667332631));
#25875=CARTESIAN_POINT('Ctrl Pts',(-40.4609678742707,36.9573501674925,38.8167734338529));
#25876=CARTESIAN_POINT('Ctrl Pts',(-40.5008388960863,37.0028602160348,38.8658238520481));
#25877=CARTESIAN_POINT('Ctrl Pts',(-40.5399676904852,37.0498205976687,38.9140644702981));
#25878=CARTESIAN_POINT('Ctrl Pts',(-40.5790964848841,37.0967809793025,38.9623050885482));
#25879=CARTESIAN_POINT('Ctrl Pts',(-40.6174830456522,37.14519168657,39.0097358991921));
#25880=CARTESIAN_POINT('Ctrl Pts',(-40.6550854902779,37.1949998998915,39.056305151788));
#25881=CARTESIAN_POINT('Ctrl Pts',(-38.3451527694219,36.0473451818618,36.3681818438339));
#25882=CARTESIAN_POINT('Ctrl Pts',(-38.3966566038503,36.0418891053477,36.428617860013));
#25883=CARTESIAN_POINT('Ctrl Pts',(-38.4482027073239,36.0383276007663,36.4891881015171));
#25884=CARTESIAN_POINT('Ctrl Pts',(-38.4997324118508,36.0366646660989,36.5498236251951));
#25885=CARTESIAN_POINT('Ctrl Pts',(-38.5512163603923,36.0350032080402,36.6104053073431));
#25886=CARTESIAN_POINT('Ctrl Pts',(-38.6026839302451,36.0352369499792,36.6710521453642));
#25887=CARTESIAN_POINT('Ctrl Pts',(-38.6540766482982,36.0373655761849,36.7316952334331));
#25888=CARTESIAN_POINT('Ctrl Pts',(-38.7054693663512,36.0394942023905,36.792338321502));
#25889=CARTESIAN_POINT('Ctrl Pts',(-38.7567872237691,36.0435177124826,36.8529776491916));
#25890=CARTESIAN_POINT('Ctrl Pts',(-38.8079719188776,36.0494314884807,36.9135443208722));
#25891=CARTESIAN_POINT('Ctrl Pts',(-38.8591566139861,36.0553452644788,36.9741109925528));
#25892=CARTESIAN_POINT('Ctrl Pts',(-38.9102081379853,36.0631493053533,37.0346049978107));
#25893=CARTESIAN_POINT('Ctrl Pts',(-38.9610684928986,36.0728347014494,37.0949576075357));
#25894=CARTESIAN_POINT('Ctrl Pts',(-39.0119288478118,36.0825200975455,37.1553102172607));
#25895=CARTESIAN_POINT('Ctrl Pts',(-39.0625980248957,36.0940868471861,37.2155214210763));
#25896=CARTESIAN_POINT('Ctrl Pts',(-39.113018461485,36.1075217693508,37.2755228123452));
#25897=CARTESIAN_POINT('Ctrl Pts',(-39.1634388980743,36.1209566915156,37.3355242036141));
#25898=CARTESIAN_POINT('Ctrl Pts',(-39.2136105854986,36.1362597838835,37.3953157720199));
#25899=CARTESIAN_POINT('Ctrl Pts',(-39.2634765269914,36.1534136240587,37.4548295886088));
#25900=CARTESIAN_POINT('Ctrl Pts',(-39.3133424684842,36.1705674642338,37.5143434051978));
#25901=CARTESIAN_POINT('Ctrl Pts',(-39.3629026554732,36.1895720492569,37.5735794597381));
#25902=CARTESIAN_POINT('Ctrl Pts',(-39.4121007864128,36.2104057549646,37.6324704550892));
#25903=CARTESIAN_POINT('Ctrl Pts',(-39.4612989173524,36.2312394606722,37.6913614504403));
#25904=CARTESIAN_POINT('Ctrl Pts',(-39.5101349837871,36.253902283474,37.749907376478));
#25905=CARTESIAN_POINT('Ctrl Pts',(-39.5585535071273,36.2783684465717,37.8080417205678));
#25906=CARTESIAN_POINT('Ctrl Pts',(-39.6069720304676,36.3028346096693,37.8661760646576));
#25907=CARTESIAN_POINT('Ctrl Pts',(-39.6549730023906,36.3291041088485,37.9238988168053));
#25908=CARTESIAN_POINT('Ctrl Pts',(-39.7025018931441,36.3571470732283,37.9811443997964));
#25909=CARTESIAN_POINT('Ctrl Pts',(-39.7500307838977,36.3851900376081,38.0383899827877));
#25910=CARTESIAN_POINT('Ctrl Pts',(-39.7970875853114,36.4150064623599,38.095158386781));
#25911=CARTESIAN_POINT('Ctrl Pts',(-39.8436188401758,36.4465624503471,38.1513851187698));
#25912=CARTESIAN_POINT('Ctrl Pts',(-39.8901500950402,36.4781184383343,38.2076118507586));
#25913=CARTESIAN_POINT('Ctrl Pts',(-39.9361557953568,36.5114139841255,38.2632969010767));
#25914=CARTESIAN_POINT('Ctrl Pts',(-39.9815836777543,36.5464112412911,38.3183770072567));
#25915=CARTESIAN_POINT('Ctrl Pts',(-40.0270115601517,36.5814084984567,38.3734571134366));
#25916=CARTESIAN_POINT('Ctrl Pts',(-40.0718616168206,36.6181074609745,38.4279322660091));
#25917=CARTESIAN_POINT('Ctrl Pts',(-40.1160828967949,36.656466419032,38.4817405765826));
#25918=CARTESIAN_POINT('Ctrl Pts',(-40.1603041767692,36.6948253770893,38.535548887156));
#25919=CARTESIAN_POINT('Ctrl Pts',(-40.2038966724473,36.7348443240874,38.5886903464796));
#25920=CARTESIAN_POINT('Ctrl Pts',(-40.2468108608757,36.7764777815053,38.6411045806601));
#25921=CARTESIAN_POINT('Ctrl Pts',(-40.2897250493041,36.8181112389233,38.6935188148405));
#25922=CARTESIAN_POINT('Ctrl Pts',(-40.3319609231047,36.8613591995997,38.7452058148664));
#25923=CARTESIAN_POINT('Ctrl Pts',(-40.3734704996928,36.9061725195211,38.7961068583283));
#25924=CARTESIAN_POINT('Ctrl Pts',(-40.414980076281,36.9509858394425,38.8470079017903));
#25925=CARTESIAN_POINT('Ctrl Pts',(-40.4557633485205,36.9973645109018,38.8971229799369));
#25926=CARTESIAN_POINT('Ctrl Pts',(-40.495773983065,37.0452558359202,38.9463951550846));
#25927=CARTESIAN_POINT('Ctrl Pts',(-40.5357846176094,37.0931471609388,38.9956673302322));
#25928=CARTESIAN_POINT('Ctrl Pts',(-40.57502260758,37.1425511312811,39.044096593909));
#25929=CARTESIAN_POINT('Ctrl Pts',(-40.6134433739962,37.1934116145889,39.0916279223511));
#25930=CARTESIAN_POINT('Ctrl Pts',(-38.2528053810356,36.051685450517,36.345998711413));
#25931=CARTESIAN_POINT('Ctrl Pts',(-38.3053282503167,36.0448725367672,36.4075425279015));
#25932=CARTESIAN_POINT('Ctrl Pts',(-38.357915230494,36.0400291326329,36.4692488577792));
#25933=CARTESIAN_POINT('Ctrl Pts',(-38.4105040239329,36.0371609165339,36.5310445960988));
#25934=CARTESIAN_POINT('Ctrl Pts',(-38.4630461209646,36.0342952472778,36.5927854626717));
#25935=CARTESIAN_POINT('Ctrl Pts',(-38.5155900182526,36.0334012603794,36.6546155674746));
#25936=CARTESIAN_POINT('Ctrl Pts',(-38.5680735815496,36.0344799595119,36.7164617913297));
#25937=CARTESIAN_POINT('Ctrl Pts',(-38.6205571448467,36.0355586586442,36.7783080151848));
#25938=CARTESIAN_POINT('Ctrl Pts',(-38.6729803643777,36.0386100435895,36.840170346572));
#25939=CARTESIAN_POINT('Ctrl Pts',(-38.7252812502133,36.0436304561532,36.9019756302016));
#25940=CARTESIAN_POINT('Ctrl Pts',(-38.7775821360489,36.0486508687169,36.9637809138313));
#25941=CARTESIAN_POINT('Ctrl Pts',(-38.8297606784486,36.055640307948,37.0255291381914));
#25942=CARTESIAN_POINT('Ctrl Pts',(-38.881755178192,36.0645904625521,37.0871472846484));
#25943=CARTESIAN_POINT('Ctrl Pts',(-38.9337496779355,36.073540617156,37.1487654311053));
#25944=CARTESIAN_POINT('Ctrl Pts',(-38.9855601253396,36.0844514854511,37.2102534881825));
#25945=CARTESIAN_POINT('Ctrl Pts',(-39.0371252575936,36.097310122788,37.2715387463425));
#25946=CARTESIAN_POINT('Ctrl Pts',(-39.0886903898476,36.1101687601249,37.3328240045024));
#25947=CARTESIAN_POINT('Ctrl Pts',(-39.1400101973423,36.1249751640943,37.3939064523297));
#25948=CARTESIAN_POINT('Ctrl Pts',(-39.1910239983568,36.1417117873728,37.4547138610926));
#25949=CARTESIAN_POINT('Ctrl Pts',(-39.2420377993713,36.1584484106512,37.5155212698555));
#25950=CARTESIAN_POINT('Ctrl Pts',(-39.2927455844049,36.1771152501096,37.576053628229));
#25951=CARTESIAN_POINT('Ctrl Pts',(-39.3430873960814,36.197690197282,37.6362393588477));
#25952=CARTESIAN_POINT('Ctrl Pts',(-39.3934292077581,36.2182651444544,37.6964250894664));
#25953=CARTESIAN_POINT('Ctrl Pts',(-39.443405036709,36.240748195499,37.7562641811227));
#25954=CARTESIAN_POINT('Ctrl Pts',(-39.49295579152,36.2651127331137,37.8156858768529));
#25955=CARTESIAN_POINT('Ctrl Pts',(-39.542506546331,36.2894772707283,37.8751075725831));
#25956=CARTESIAN_POINT('Ctrl Pts',(-39.5916322177749,36.3157232903655,37.9341118613208));
#25957=CARTESIAN_POINT('Ctrl Pts',(-39.6402747199215,36.3438197288223,37.9926289735902));
#25958=CARTESIAN_POINT('Ctrl Pts',(-39.688917222068,36.371916167279,38.0511460858596));
#25959=CARTESIAN_POINT('Ctrl Pts',(-39.7370765458555,36.4018630193127,38.1091760107623));
#25960=CARTESIAN_POINT('Ctrl Pts',(-39.7846957480054,36.4336248492489,38.1666501310679));
#25961=CARTESIAN_POINT('Ctrl Pts',(-39.8323149501553,36.4653866791851,38.2241242513735));
#25962=CARTESIAN_POINT('Ctrl Pts',(-39.8793940217993,36.4989634811011,38.2810425563783));
#25963=CARTESIAN_POINT('Ctrl Pts',(-39.9258772967491,36.5343155305869,38.3373377431282));
#25964=CARTESIAN_POINT('Ctrl Pts',(-39.972360571699,36.5696675800726,38.3936329298781));
#25965=CARTESIAN_POINT('Ctrl Pts',(-40.0182480412996,36.606794870538,38.4493049878891));
#25966=CARTESIAN_POINT('Ctrl Pts',(-40.0634854479255,36.6456534827089,38.5042880874195));
#25967=CARTESIAN_POINT('Ctrl Pts',(-40.1087228545514,36.6845120948799,38.5592711869499));
#25968=CARTESIAN_POINT('Ctrl Pts',(-40.1533101897776,36.725102021514,38.6135653177595));
#25969=CARTESIAN_POINT('Ctrl Pts',(-40.1971947326411,36.7673752522233,38.6671062787693));
#25970=CARTESIAN_POINT('Ctrl Pts',(-40.2410792755046,36.8096484829327,38.7206472397791));
#25971=CARTESIAN_POINT('Ctrl Pts',(-40.2842610178336,36.8536050098406,38.7734350210174));
#25972=CARTESIAN_POINT('Ctrl Pts',(-40.3266888998378,36.8991928448641,38.8254072016798));
#25973=CARTESIAN_POINT('Ctrl Pts',(-40.369116781842,36.9447806798878,38.8773793823421));
#25974=CARTESIAN_POINT('Ctrl Pts',(-40.410790795619,36.9919998145336,38.9285359527485));
#25975=CARTESIAN_POINT('Ctrl Pts',(-40.451661663113,37.0407944058147,38.9788164197751));
#25976=CARTESIAN_POINT('Ctrl Pts',(-40.4925325306069,37.0895889970958,39.0290968868015));
#25977=CARTESIAN_POINT('Ctrl Pts',(-40.5326002442068,37.1399590359233,39.078501241083));
#25978=CARTESIAN_POINT('Ctrl Pts',(-40.5718174239661,37.1918449563019,39.1269710600356));
#25979=CARTESIAN_POINT('Ctrl Pts',(-38.1617009122515,36.0575623125548,36.3251892428041));
#25980=CARTESIAN_POINT('Ctrl Pts',(-38.2151985657498,36.0493560734031,36.387790684347));
#25981=CARTESIAN_POINT('Ctrl Pts',(-38.2687839975976,36.0431937832001,36.4505850367912));
#25982=CARTESIAN_POINT('Ctrl Pts',(-38.3223911778814,36.039083033096,36.5134949225584));
#25983=CARTESIAN_POINT('Ctrl Pts',(-38.3759507574777,36.0349759331473,36.5763489472675));
#25984=CARTESIAN_POINT('Ctrl Pts',(-38.4295320360924,36.0329167323991,36.6393182875267));
#25985=CARTESIAN_POINT('Ctrl Pts',(-38.4830691061556,36.0329079637685,36.702325487995));
#25986=CARTESIAN_POINT('Ctrl Pts',(-38.5366061762187,36.0328991951379,36.7653326884632));
#25987=CARTESIAN_POINT('Ctrl Pts',(-38.5900990269231,36.0349408586266,36.8283777364218));
#25988=CARTESIAN_POINT('Ctrl Pts',(-38.6434818594694,36.0390304428894,36.8913830834058));
#25989=CARTESIAN_POINT('Ctrl Pts',(-38.6968646920157,36.0431200271523,36.9543884303896));
#25990=CARTESIAN_POINT('Ctrl Pts',(-38.750137495628,36.0492575313638,37.0173540636806));
#25991=CARTESIAN_POINT('Ctrl Pts',(-38.8032347421755,36.0574354060963,37.0802025324973));
#25992=CARTESIAN_POINT('Ctrl Pts',(-38.856331988723,36.0656132808288,37.143051001314));
#25993=CARTESIAN_POINT('Ctrl Pts',(-38.9092536674875,36.0758315244315,37.2057822929699));
#25994=CARTESIAN_POINT('Ctrl Pts',(-38.9619346822386,36.0880775679694,37.2683192449354));
#25995=CARTESIAN_POINT('Ctrl Pts',(-39.0146156969898,36.1003236115073,37.3308561969009));
#25996=CARTESIAN_POINT('Ctrl Pts',(-39.0670560370872,36.1145974525074,37.3931987965509));
#25997=CARTESIAN_POINT('Ctrl Pts',(-39.1191911983832,36.1308815334554,37.4552703594684));
#25998=CARTESIAN_POINT('Ctrl Pts',(-39.1713263596792,36.1471656144034,37.517341922386));
#25999=CARTESIAN_POINT('Ctrl Pts',(-39.2231563316488,36.1654599320122,37.579142436041));
#26000=CARTESIAN_POINT('Ctrl Pts',(-39.2746173609027,36.1857419833824,37.6405958828037));
#26001=CARTESIAN_POINT('Ctrl Pts',(-39.3260783901567,36.2060240347524,37.7020493295664));
#26002=CARTESIAN_POINT('Ctrl Pts',(-39.3771704663128,36.2282938157907,37.7631556970329));
#26003=CARTESIAN_POINT('Ctrl Pts',(-39.4278307436407,36.2525239335868,37.8238398214092));
#26004=CARTESIAN_POINT('Ctrl Pts',(-39.4784910209687,36.276754051383,37.8845239457855));
#26005=CARTESIAN_POINT('Ctrl Pts',(-39.5287194892421,36.302944501046,37.9447858148217));
#26006=CARTESIAN_POINT('Ctrl Pts',(-39.5784543650103,36.3310630670532,38.0045513034978));
#26007=CARTESIAN_POINT('Ctrl Pts',(-39.6281892407785,36.3591816330604,38.0643167921739));
#26008=CARTESIAN_POINT('Ctrl Pts',(-39.6774305139982,36.3892283097345,38.1235858884251));
#26009=CARTESIAN_POINT('Ctrl Pts',(-39.726117615524,36.4211661382093,38.182285688391));
#26010=CARTESIAN_POINT('Ctrl Pts',(-39.7748047170498,36.453103966684,38.2409854883569));
#26011=CARTESIAN_POINT('Ctrl Pts',(-39.8229376370528,36.4869329405122,38.2991159801882));
#26012=CARTESIAN_POINT('Ctrl Pts',(-39.870457169702,36.5226114484139,38.3566056605612));
#26013=CARTESIAN_POINT('Ctrl Pts',(-39.9179767023511,36.5582899563156,38.4140953409343));
#26014=CARTESIAN_POINT('Ctrl Pts',(-39.9648828380547,36.595817991089,38.4709441982441));
#26015=CARTESIAN_POINT('Ctrl Pts',(-40.0111178799974,36.6351493914341,38.5270823056415));
#26016=CARTESIAN_POINT('Ctrl Pts',(-40.0573529219401,36.6744807917791,38.5832204130388));
#26017=CARTESIAN_POINT('Ctrl Pts',(-40.102916860788,36.7156155497563,38.6386477591913));
#26018=CARTESIAN_POINT('Ctrl Pts',(-40.1477536506837,36.7585030676174,38.6932961657759));
#26019=CARTESIAN_POINT('Ctrl Pts',(-40.1925904405793,36.8013905854786,38.7479445723606));
#26020=CARTESIAN_POINT('Ctrl Pts',(-40.2367000724727,36.8460308545666,38.8018140283461));
#26021=CARTESIAN_POINT('Ctrl Pts',(-40.2800282893812,36.8923689651881,38.8548382716906));
#26022=CARTESIAN_POINT('Ctrl Pts',(-40.3233565062898,36.9387070758096,38.9078625150351));
#26023=CARTESIAN_POINT('Ctrl Pts',(-40.3659032994663,36.9867430186105,38.960041535035));
#26024=CARTESIAN_POINT('Ctrl Pts',(-40.4076163342913,37.0364177070515,39.0113111489662));
#26025=CARTESIAN_POINT('Ctrl Pts',(-40.4493293691164,37.0860923954925,39.0625807628974));
#26026=CARTESIAN_POINT('Ctrl Pts',(-40.4902086371704,37.1374058195468,39.1129409604106));
#26027=CARTESIAN_POINT('Ctrl Pts',(-40.5302038549723,37.1902948612154,39.1623297960218));
#26028=CARTESIAN_POINT('Ctrl Pts',(-38.0705964434674,36.0634391745925,36.3043797741951));
#26029=CARTESIAN_POINT('Ctrl Pts',(-38.125068881183,36.053839610039,36.3680388407926));
#26030=CARTESIAN_POINT('Ctrl Pts',(-38.1796527647013,36.0463584337675,36.4319212158031));
#26031=CARTESIAN_POINT('Ctrl Pts',(-38.2342783318298,36.0410051496582,36.4959452490178));
#26032=CARTESIAN_POINT('Ctrl Pts',(-38.2888553939909,36.0356566190167,36.5599124318634));
#26033=CARTESIAN_POINT('Ctrl Pts',(-38.3434740539323,36.0324322044189,36.6240210075788));
#26034=CARTESIAN_POINT('Ctrl Pts',(-38.3980646307614,36.0313359680253,36.6881891846602));
#26035=CARTESIAN_POINT('Ctrl Pts',(-38.4526552075906,36.0302397316317,36.7523573617416));
#26036=CARTESIAN_POINT('Ctrl Pts',(-38.5072176894685,36.0312716736637,36.8165851262716));
#26037=CARTESIAN_POINT('Ctrl Pts',(-38.5616824687255,36.0344304296258,36.8807905366098));
#26038=CARTESIAN_POINT('Ctrl Pts',(-38.6161472479825,36.0375891855878,36.944995946948));
#26039=CARTESIAN_POINT('Ctrl Pts',(-38.6705143128074,36.0428747547796,37.0091789891697));
#26040=CARTESIAN_POINT('Ctrl Pts',(-38.724714306159,36.0502803496406,37.0732577803462));
#26041=CARTESIAN_POINT('Ctrl Pts',(-38.7789142995106,36.0576859445016,37.1373365715227));
#26042=CARTESIAN_POINT('Ctrl Pts',(-38.8329472096354,36.0672115634119,37.2013110977573));
#26043=CARTESIAN_POINT('Ctrl Pts',(-38.8867441068837,36.0788450131507,37.2650997435283));
#26044=CARTESIAN_POINT('Ctrl Pts',(-38.940541004132,36.0904784628896,37.3288883892993));
#26045=CARTESIAN_POINT('Ctrl Pts',(-38.9941018768322,36.1042197409205,37.3924911407721));
#26046=CARTESIAN_POINT('Ctrl Pts',(-39.0473583984096,36.120051279538,37.4558268578443));
#26047=CARTESIAN_POINT('Ctrl Pts',(-39.100614919987,36.1358828181555,37.5191625749165));
#26048=CARTESIAN_POINT('Ctrl Pts',(-39.1535670788927,36.1538046139148,37.582231243853));
#26049=CARTESIAN_POINT('Ctrl Pts',(-39.206147325724,36.1737937694826,37.6449524067597));
#26050=CARTESIAN_POINT('Ctrl Pts',(-39.2587275725553,36.1937829250503,37.7076735696665));
#26051=CARTESIAN_POINT('Ctrl Pts',(-39.3109358959166,36.2158394360822,37.7700472129432));
#26052=CARTESIAN_POINT('Ctrl Pts',(-39.3627056957615,36.2399351340599,37.8319937659655));
#26053=CARTESIAN_POINT('Ctrl Pts',(-39.4144754956064,36.2640308320376,37.8939403189879));
#26054=CARTESIAN_POINT('Ctrl Pts',(-39.4658067607094,36.2901657117264,37.9554597683227));
#26055=CARTESIAN_POINT('Ctrl Pts',(-39.5166340100992,36.3183064052841,38.0164736334055));
#26056=CARTESIAN_POINT('Ctrl Pts',(-39.567461259489,36.3464470988418,38.0774874984883));
#26057=CARTESIAN_POINT('Ctrl Pts',(-39.6177844821409,36.3765936001565,38.1379957660878));
#26058=CARTESIAN_POINT('Ctrl Pts',(-39.6675394830426,36.4087074271696,38.1979212457141));
#26059=CARTESIAN_POINT('Ctrl Pts',(-39.7172944839443,36.4408212541828,38.2578467253403));
#26060=CARTESIAN_POINT('Ctrl Pts',(-39.7664812523064,36.4749023999232,38.3171894039982));
#26061=CARTESIAN_POINT('Ctrl Pts',(-39.8150370426548,36.510907366241,38.3758735779943));
#26062=CARTESIAN_POINT('Ctrl Pts',(-39.8635928330032,36.5469123325587,38.4345577519904));
#26063=CARTESIAN_POINT('Ctrl Pts',(-39.9115176348099,36.58484111164,38.4925834085993));
#26064=CARTESIAN_POINT('Ctrl Pts',(-39.9587503120694,36.6246453001592,38.5498765238635));
#26065=CARTESIAN_POINT('Ctrl Pts',(-40.0059829893289,36.6644494886784,38.6071696391278));
#26066=CARTESIAN_POINT('Ctrl Pts',(-40.0525235317984,36.7061290779986,38.6637302006231));
#26067=CARTESIAN_POINT('Ctrl Pts',(-40.0983125687262,36.7496308830115,38.7194860527826));
#26068=CARTESIAN_POINT('Ctrl Pts',(-40.1441016056541,36.7931326880244,38.7752419049421));
#26069=CARTESIAN_POINT('Ctrl Pts',(-40.1891391271119,36.8384566992927,38.8301930356747));
#26070=CARTESIAN_POINT('Ctrl Pts',(-40.2333676789247,36.8855450855121,38.8842693417014));
#26071=CARTESIAN_POINT('Ctrl Pts',(-40.2775962307375,36.9326334717315,38.938345647728));
#26072=CARTESIAN_POINT('Ctrl Pts',(-40.3210158033137,36.9814862226874,38.9915471173214));
#26073=CARTESIAN_POINT('Ctrl Pts',(-40.3635710054698,37.0320410082882,39.0438058781573));
#26074=CARTESIAN_POINT('Ctrl Pts',(-40.4061262076258,37.0825957938891,39.0960646389932));
#26075=CARTESIAN_POINT('Ctrl Pts',(-40.4478170301341,37.1348526031702,39.1473806797382));
#26076=CARTESIAN_POINT('Ctrl Pts',(-40.4885902859785,37.1887447661289,39.197688532008));
#26077=CARTESIAN_POINT('Ctrl Pts',(-37.9807359148445,36.0708539957089,36.2849451673821));
#26078=CARTESIAN_POINT('Ctrl Pts',(-38.0361388636876,36.0598245864939,36.349611657568));
#26079=CARTESIAN_POINT('Ctrl Pts',(-38.0916787515611,36.0509875068319,36.4145339633157));
#26080=CARTESIAN_POINT('Ctrl Pts',(-38.1472819813364,36.044354405607,36.4796260509332));
#26081=CARTESIAN_POINT('Ctrl Pts',(-38.202835838025,36.0377271942682,36.5446603397988));
#26082=CARTESIAN_POINT('Ctrl Pts',(-38.2584529112245,36.0333000505676,36.609864093988));
#26083=CARTESIAN_POINT('Ctrl Pts',(-38.314059634525,36.0310787757327,36.675151063009));
#26084=CARTESIAN_POINT('Ctrl Pts',(-38.3696663578256,36.0288575008977,36.74043803203));
#26085=CARTESIAN_POINT('Ctrl Pts',(-38.4252627182639,36.0288420954269,36.8058082006614));
#26086=CARTESIAN_POINT('Ctrl Pts',(-38.4807751786657,36.0310325287199,36.8711751005551));
#26087=CARTESIAN_POINT('Ctrl Pts',(-38.5362876390675,36.033222962013,36.9365420004487));
#26088=CARTESIAN_POINT('Ctrl Pts',(-38.5917161864921,36.0376192335413,37.0019056163654));
#26089=CARTESIAN_POINT('Ctrl Pts',(-38.646987507313,36.0442154811027,37.0671794905916));
#26090=CARTESIAN_POINT('Ctrl Pts',(-38.7022588281338,36.0508117286641,37.1324533648177));
#26091=CARTESIAN_POINT('Ctrl Pts',(-38.7573729094671,36.0596079507043,37.1976374821365));
#26092=CARTESIAN_POINT('Ctrl Pts',(-38.8122568549514,36.0705924690439,37.2626456239265));
#26093=CARTESIAN_POINT('Ctrl Pts',(-38.8671408004357,36.0815769873834,37.3276537657165));
#26094=CARTESIAN_POINT('Ctrl Pts',(-38.9217945972781,36.0947497994464,37.3924859168235));
#26095=CARTESIAN_POINT('Ctrl Pts',(-38.9761459589933,36.1100934420574,37.4570563255389));
#26096=CARTESIAN_POINT('Ctrl Pts',(-39.0304973207086,36.1254370846684,37.5216267342543));
#26097=CARTESIAN_POINT('Ctrl Pts',(-39.0845462346282,36.1429515542368,37.5859353855265));
#26098=CARTESIAN_POINT('Ctrl Pts',(-39.1382212151398,36.1626136488479,37.6498972211433));
#26099=CARTESIAN_POINT('Ctrl Pts',(-39.1918961956515,36.182275743459,37.7138590567601));
#26100=CARTESIAN_POINT('Ctrl Pts',(-39.2451972302446,36.2040854585169,37.777474061812));
#26101=CARTESIAN_POINT('Ctrl Pts',(-39.2980538230577,36.2280139147768,37.840658096331));
#26102=CARTESIAN_POINT('Ctrl Pts',(-39.3509104158708,36.2519423710367,37.9038421308499));
#26103=CARTESIAN_POINT('Ctrl Pts',(-39.403322554584,36.2779895629094,37.966595180108));
#26104=CARTESIAN_POINT('Ctrl Pts',(-39.4552209193481,36.3061210102197,38.0288342447005));
#26105=CARTESIAN_POINT('Ctrl Pts',(-39.5071192841123,36.3342524575298,38.091073309293));
#26106=CARTESIAN_POINT('Ctrl Pts',(-39.558503862831,36.3644681537101,38.1527983747124));
#26107=CARTESIAN_POINT('Ctrl Pts',(-39.6093066948198,36.3967281088421,38.2139278014215));
#26108=CARTESIAN_POINT('Ctrl Pts',(-39.6601095268087,36.4289880639741,38.2750572281306));
#26109=CARTESIAN_POINT('Ctrl Pts',(-39.7103306002267,36.4632922705294,38.3355910018807));
#26110=CARTESIAN_POINT('Ctrl Pts',(-39.7599034931162,36.4995953345826,38.3954490587125));
#26111=CARTESIAN_POINT('Ctrl Pts',(-39.8094763860058,36.5358983986359,38.4553071155443));
#26112=CARTESIAN_POINT('Ctrl Pts',(-39.8584010868125,36.5742003117175,38.5144894415054));
#26113=CARTESIAN_POINT('Ctrl Pts',(-39.9066128878016,36.6144503958987,38.5729177597622));
#26114=CARTESIAN_POINT('Ctrl Pts',(-39.9548246887907,36.65470048008,38.631346078019));
#26115=CARTESIAN_POINT('Ctrl Pts',(-40.0023235787247,36.6968987259727,38.689020374952));
#26116=CARTESIAN_POINT('Ctrl Pts',(-40.0490467350601,36.7409893056005,38.7458643676801));
#26117=CARTESIAN_POINT('Ctrl Pts',(-40.0957698913955,36.7850798852282,38.8027083604082));
#26118=CARTESIAN_POINT('Ctrl Pts',(-40.1417173032415,36.8310627883089,38.8587220356807));
#26119=CARTESIAN_POINT('Ctrl Pts',(-40.1868281992345,36.878877184372,38.9138313061286));
#26120=CARTESIAN_POINT('Ctrl Pts',(-40.2319390952273,36.9266915804353,38.9689405765764));
#26121=CARTESIAN_POINT('Ctrl Pts',(-40.2762134648518,36.976337458332,39.0231454293531));
#26122=CARTESIAN_POINT('Ctrl Pts',(-40.3195927484955,37.0277491458603,39.0763741683628));
#26123=CARTESIAN_POINT('Ctrl Pts',(-40.3629720321391,37.0791608333887,39.1296029073724));
#26124=CARTESIAN_POINT('Ctrl Pts',(-40.4054562196899,37.1323383185621,39.1818555202063));
#26125=CARTESIAN_POINT('Ctrl Pts',(-40.4469891180173,37.1872112609937,39.2330628914883));
#26126=CARTESIAN_POINT('Ctrl Pts',(-37.8919774678215,36.0796223244832,36.2667225297271));
#26127=CARTESIAN_POINT('Ctrl Pts',(-37.9482699971579,36.067131319434,36.3323499709714));
#26128=CARTESIAN_POINT('Ctrl Pts',(-38.0047267235371,36.0569059654783,36.3982677820133));
#26129=CARTESIAN_POINT('Ctrl Pts',(-38.0612701224292,36.0489603009388,36.4643854465506));
#26130=CARTESIAN_POINT('Ctrl Pts',(-38.1177633134081,36.0410216917806,36.5304444016712));
#26131=CARTESIAN_POINT('Ctrl Pts',(-38.1743430088834,36.0353587273096,36.596702838963));
#26132=CARTESIAN_POINT('Ctrl Pts',(-38.2309316534887,36.0319791699089,36.6630699361382));
#26133=CARTESIAN_POINT('Ctrl Pts',(-38.2875202980941,36.0285996125084,36.7294370333135));
#26134=CARTESIAN_POINT('Ctrl Pts',(-38.3441178776431,36.0275034630254,36.7959127737345));
#26135=CARTESIAN_POINT('Ctrl Pts',(-38.4006468122553,36.0286922239828,36.8624060372502));
#26136=CARTESIAN_POINT('Ctrl Pts',(-38.4571757468675,36.0298809849402,36.9288993007659));
#26137=CARTESIAN_POINT('Ctrl Pts',(-38.5136360223715,36.03335465604,36.9954100707068));
#26138=CARTESIAN_POINT('Ctrl Pts',(-38.5699502470932,36.0391084758241,37.0618471789059));
#26139=CARTESIAN_POINT('Ctrl Pts',(-38.6262644718148,36.0448622956084,37.128284287105));
#26140=CARTESIAN_POINT('Ctrl Pts',(-38.6824326316366,36.0528962626346,37.194647716907));
#26141=CARTESIAN_POINT('Ctrl Pts',(-38.7383777352955,36.0631993645204,37.260846502108));
#26142=CARTESIAN_POINT('Ctrl Pts',(-38.7943228389544,36.073502466406,37.3270452873091));
#26143=CARTESIAN_POINT('Ctrl Pts',(-38.8500448724255,36.0860747005682,37.3930794113136));
#26144=CARTESIAN_POINT('Ctrl Pts',(-38.9054674559635,36.1008988338949,37.4588583593065));
#26145=CARTESIAN_POINT('Ctrl Pts',(-38.9608900395015,36.1157229672217,37.5246373072994));
#26146=CARTESIAN_POINT('Ctrl Pts',(-39.0160131592125,36.1327989959966,37.5901610627903));
#26147=CARTESIAN_POINT('Ctrl Pts',(-39.0707612562991,36.152103513631,37.6553398105404));
#26148=CARTESIAN_POINT('Ctrl Pts',(-39.1255093533857,36.1714080312654,37.7205185582905));
#26149=CARTESIAN_POINT('Ctrl Pts',(-39.179882414123,36.1929410329197,37.7853522819599));
#26150=CARTESIAN_POINT('Ctrl Pts',(-39.2338059078403,36.2166730027081,37.8497521121557));
#26151=CARTESIAN_POINT('Ctrl Pts',(-39.2877294015577,36.2404049724964,37.9141519423515));
#26152=CARTESIAN_POINT('Ctrl Pts',(-39.3412033147369,36.2663359044695,37.9781178629291));
#26153=CARTESIAN_POINT('Ctrl Pts',(-39.394154349194,36.2944302543756,38.0415621940174));
#26154=CARTESIAN_POINT('Ctrl Pts',(-39.447105383651,36.3225246042818,38.1050065251057));
#26155=CARTESIAN_POINT('Ctrl Pts',(-39.4995335261116,36.352782365078,38.1679292507998));
#26156=CARTESIAN_POINT('Ctrl Pts',(-39.5513669118587,36.3851620616078,38.2302441211647));
#26157=CARTESIAN_POINT('Ctrl Pts',(-39.6032002976058,36.4175417581375,38.2925589915297));
#26158=CARTESIAN_POINT('Ctrl Pts',(-39.6544389136452,36.4520433822834,38.3542659909437));
#26159=CARTESIAN_POINT('Ctrl Pts',(-39.7050125257772,36.4886196417072,38.4152805359019));
#26160=CARTESIAN_POINT('Ctrl Pts',(-39.7555861379091,36.5251959011311,38.4762950808601));
#26161=CARTESIAN_POINT('Ctrl Pts',(-39.8054947334551,36.5638467866634,38.5366171560666));
#26162=CARTESIAN_POINT('Ctrl Pts',(-39.8546699013115,36.6045193184576,38.5961640763708));
#26163=CARTESIAN_POINT('Ctrl Pts',(-39.9038450691679,36.6451918502518,38.655710996675));
#26164=CARTESIAN_POINT('Ctrl Pts',(-39.9522867970068,36.6878860181116,38.7144827471489));
#26165=CARTESIAN_POINT('Ctrl Pts',(-39.9999286844011,36.7325432999504,38.7723987677153));
#26166=CARTESIAN_POINT('Ctrl Pts',(-40.0475705717954,36.7772005817894,38.8303147882816));
#26167=CARTESIAN_POINT('Ctrl Pts',(-40.0944126068016,36.8238209664121,38.8873750644213));
#26168=CARTESIAN_POINT('Ctrl Pts',(-40.140390581736,36.8723405499575,38.9435013820225));
#26169=CARTESIAN_POINT('Ctrl Pts',(-40.1863685566705,36.9208601335028,38.9996276996238));
#26170=CARTESIAN_POINT('Ctrl Pts',(-40.2314824600069,36.9712789038072,39.0548200446163));
#26171=CARTESIAN_POINT('Ctrl Pts',(-40.2756704528598,37.0235277504564,39.1090027633136));
#26172=CARTESIAN_POINT('Ctrl Pts',(-40.3198584457128,37.0757765971056,39.1631854820109));
#26173=CARTESIAN_POINT('Ctrl Pts',(-40.3631205170047,37.129855507001,39.2163585608298));
#26174=CARTESIAN_POINT('Ctrl Pts',(-40.4053973662082,37.1856903526729,39.2684491139483));
#26175=CARTESIAN_POINT('Ctrl Pts',(-37.8032190207985,36.0883906532575,36.248499892072));
#26176=CARTESIAN_POINT('Ctrl Pts',(-37.8604011306282,36.0744380523741,36.3150882843748));
#26177=CARTESIAN_POINT('Ctrl Pts',(-37.9177746955132,36.0628244241247,36.382001600711));
#26178=CARTESIAN_POINT('Ctrl Pts',(-37.975258263522,36.0535661962707,36.4491448421679));
#26179=CARTESIAN_POINT('Ctrl Pts',(-38.0326907887911,36.0443161892931,36.5162284635436));
#26180=CARTESIAN_POINT('Ctrl Pts',(-38.0902331065422,36.0374174040515,36.5835415839379));
#26181=CARTESIAN_POINT('Ctrl Pts',(-38.1478036724524,36.0328795640852,36.6509888092675));
#26182=CARTESIAN_POINT('Ctrl Pts',(-38.2053742383626,36.028341724119,36.7184360345971));
#26183=CARTESIAN_POINT('Ctrl Pts',(-38.2629730370223,36.0261648306239,36.7860173468077));
#26184=CARTESIAN_POINT('Ctrl Pts',(-38.3205184458449,36.0263519192456,36.8536369739454));
#26185=CARTESIAN_POINT('Ctrl Pts',(-38.3780638546675,36.0265390078675,36.921256601083));
#26186=CARTESIAN_POINT('Ctrl Pts',(-38.4355558582509,36.0290900785386,36.9889145250481));
#26187=CARTESIAN_POINT('Ctrl Pts',(-38.4929129868733,36.0340014705456,37.0565148672202));
#26188=CARTESIAN_POINT('Ctrl Pts',(-38.5502701154958,36.0389128625527,37.1241152093923));
#26189=CARTESIAN_POINT('Ctrl Pts',(-38.6074923538061,36.046184574565,37.1916579516774));
#26190=CARTESIAN_POINT('Ctrl Pts',(-38.6644986156396,36.0558062599968,37.2590473802896));
#26191=CARTESIAN_POINT('Ctrl Pts',(-38.7215048774731,36.0654279454286,37.3264368089017));
#26192=CARTESIAN_POINT('Ctrl Pts',(-38.7782951475729,36.07739960169,37.3936729058038));
#26193=CARTESIAN_POINT('Ctrl Pts',(-38.8347889529337,36.0917042257324,37.4606603930742));
#26194=CARTESIAN_POINT('Ctrl Pts',(-38.8912827582945,36.1060088497749,37.5276478803445));
#26195=CARTESIAN_POINT('Ctrl Pts',(-38.9474800837969,36.1226464377564,37.5943867400541));
#26196=CARTESIAN_POINT('Ctrl Pts',(-39.0033012974584,36.141593378414,37.6607823999375));
#26197=CARTESIAN_POINT('Ctrl Pts',(-39.0591225111199,36.1605403190717,37.7271780598209));
#26198=CARTESIAN_POINT('Ctrl Pts',(-39.1145675980014,36.1817966073224,37.7932305021078));
#26199=CARTESIAN_POINT('Ctrl Pts',(-39.1695579926229,36.2053320906394,37.8588461279804));
#26200=CARTESIAN_POINT('Ctrl Pts',(-39.2245483872446,36.2288675739563,37.924461753853));
#26201=CARTESIAN_POINT('Ctrl Pts',(-39.2790840748897,36.2546822460295,37.9896405457502));
#26202=CARTESIAN_POINT('Ctrl Pts',(-39.3330877790397,36.2827394985316,38.0542901433343));
#26203=CARTESIAN_POINT('Ctrl Pts',(-39.3870914831897,36.3107967510337,38.1189397409185));
#26204=CARTESIAN_POINT('Ctrl Pts',(-39.4405631893923,36.3410965764458,38.1830601268872));
#26205=CARTESIAN_POINT('Ctrl Pts',(-39.4934271288977,36.3735960143734,38.246560440908));
#26206=CARTESIAN_POINT('Ctrl Pts',(-39.546291068403,36.4060954523009,38.3100607549287));
#26207=CARTESIAN_POINT('Ctrl Pts',(-39.5985472270638,36.4407944940374,38.3729409800067));
#26208=CARTESIAN_POINT('Ctrl Pts',(-39.6501215584381,36.4776439488319,38.4351120130913));
#26209=CARTESIAN_POINT('Ctrl Pts',(-39.7016958898123,36.5144934036264,38.4972830461759));
#26210=CARTESIAN_POINT('Ctrl Pts',(-39.7525883800977,36.5534932616094,38.5587448706279));
#26211=CARTESIAN_POINT('Ctrl Pts',(-39.8027269148214,36.5945882410166,38.6194103929794));
#26212=CARTESIAN_POINT('Ctrl Pts',(-39.8528654495451,36.6356832204237,38.680075915331));
#26213=CARTESIAN_POINT('Ctrl Pts',(-39.9022500152889,36.6788733102505,38.7399451193458));
#26214=CARTESIAN_POINT('Ctrl Pts',(-39.9508106337421,36.7240972943005,38.7989331677504));
#26215=CARTESIAN_POINT('Ctrl Pts',(-39.9993712521953,36.7693212783505,38.8579212161551));
#26216=CARTESIAN_POINT('Ctrl Pts',(-40.0471079103616,36.8165791445153,38.9160280931619));
#26217=CARTESIAN_POINT('Ctrl Pts',(-40.0939529642376,36.8658039155428,38.9731714579166));
#26218=CARTESIAN_POINT('Ctrl Pts',(-40.1407980181136,36.9150286865703,39.0303148226713));
#26219=CARTESIAN_POINT('Ctrl Pts',(-40.1867514551618,36.9662203492825,39.0864946598795));
#26220=CARTESIAN_POINT('Ctrl Pts',(-40.2317481572241,37.0193063550525,39.1416313582644));
#26221=CARTESIAN_POINT('Ctrl Pts',(-40.2767448592865,37.0723923608224,39.1967680566494));
#26222=CARTESIAN_POINT('Ctrl Pts',(-40.3207848143196,37.1273726954398,39.2508616014532));
#26223=CARTESIAN_POINT('Ctrl Pts',(-40.363805614399,37.184169444352,39.3038353364083));
#26224=CARTESIAN_POINT('Ctrl Pts',(-37.7155633104343,36.0985133588211,36.2314899874893));
#26225=CARTESIAN_POINT('Ctrl Pts',(-37.7735940555694,36.0830673910403,36.2989928414705));
#26226=CARTESIAN_POINT('Ctrl Pts',(-37.8318452786789,36.0700330978996,36.3668572209427));
#26227=CARTESIAN_POINT('Ctrl Pts',(-37.8902315079545,36.0594295410209,36.4349835452439));
#26228=CARTESIAN_POINT('Ctrl Pts',(-37.948565892969,36.0488353996083,36.5030493765319));
#26229=CARTESIAN_POINT('Ctrl Pts',(-38.0070350278182,36.0406676826179,36.5713766682024));
#26230=CARTESIAN_POINT('Ctrl Pts',(-38.0655532757724,36.0349382968221,36.6398653415568));
#26231=CARTESIAN_POINT('Ctrl Pts',(-38.1240715237266,36.0292089110264,36.7083540149113));
#26232=CARTESIAN_POINT('Ctrl Pts',(-38.1826388680546,36.0259178580415,36.7770040503664));
#26233=CARTESIAN_POINT('Ctrl Pts',(-38.2411695302526,36.0250699058513,36.8457148990595));
#26234=CARTESIAN_POINT('Ctrl Pts',(-38.2997001924505,36.0242219536612,36.9144257477526));
#26235=CARTESIAN_POINT('Ctrl Pts',(-38.3581941557842,36.025817102488,36.9831973900379));
#26236=CARTESIAN_POINT('Ctrl Pts',(-38.4165657510128,36.0298529677364,37.0519291011623));
#26237=CARTESIAN_POINT('Ctrl Pts',(-38.4749373462413,36.0338888329847,37.1206608122868));
#26238=CARTESIAN_POINT('Ctrl Pts',(-38.5331865566767,36.0403654134821,37.1893525725995));
#26239=CARTESIAN_POINT('Ctrl Pts',(-38.5912280730533,36.0492731791837,37.2579037762394));
#26240=CARTESIAN_POINT('Ctrl Pts',(-38.6492695894299,36.0581809448852,37.3264549798792));
#26241=CARTESIAN_POINT('Ctrl Pts',(-38.7071033951548,36.069519893227,37.3948656072474));
#26242=CARTESIAN_POINT('Ctrl Pts',(-38.7646447905916,36.0832733767442,37.4630354658025));
#26243=CARTESIAN_POINT('Ctrl Pts',(-38.8221861860284,36.0970268602613,37.5312053243577));
#26244=CARTESIAN_POINT('Ctrl Pts',(-38.8794351547276,36.1131948750061,37.5991343946107));
#26245=CARTESIAN_POINT('Ctrl Pts',(-38.9363078545486,36.1317537049394,37.6667231905533));
#26246=CARTESIAN_POINT('Ctrl Pts',(-38.9931805543695,36.1503125348727,37.7343119864959));
#26247=CARTESIAN_POINT('Ctrl Pts',(-39.0496769690542,36.1712621746747,37.8015604888055));
#26248=CARTESIAN_POINT('Ctrl Pts',(-39.1057143593112,36.194571909252,37.8683702091491));
#26249=CARTESIAN_POINT('Ctrl Pts',(-39.1617517495681,36.2178816438295,37.9351799294927));
#26250=CARTESIAN_POINT('Ctrl Pts',(-39.2173300993782,36.2435514665059,38.0015508487707));
#26251=CARTESIAN_POINT('Ctrl Pts',(-39.2723680144236,36.2715437531241,38.0673857645443));
#26252=CARTESIAN_POINT('Ctrl Pts',(-39.3274059294689,36.2995360397424,38.1332206803179));
#26253=CARTESIAN_POINT('Ctrl Pts',(-39.3819033940163,36.3298507822888,38.1985195737665));
#26254=CARTESIAN_POINT('Ctrl Pts',(-39.4357805969077,36.3624435577397,38.2631868128));
#26255=CARTESIAN_POINT('Ctrl Pts',(-39.4896577997992,36.3950363331905,38.3278540518334));
#26256=CARTESIAN_POINT('Ctrl Pts',(-39.5429147256334,36.4299071322184,38.3918896179649));
#26257=CARTESIAN_POINT('Ctrl Pts',(-39.5954733799659,36.4670048630141,38.4551997293104));
#26258=CARTESIAN_POINT('Ctrl Pts',(-39.6480320342983,36.5041025938097,38.5185098406561));
#26259=CARTESIAN_POINT('Ctrl Pts',(-39.6998924021046,36.5434272457595,38.5810944791169));
#26260=CARTESIAN_POINT('Ctrl Pts',(-39.7509785338906,36.5849212078543,38.6428619874586));
#26261=CARTESIAN_POINT('Ctrl Pts',(-39.8020646656766,36.6264151699492,38.7046294958002));
#26262=CARTESIAN_POINT('Ctrl Pts',(-39.8523765468386,36.67007843032,38.7655798563646));
#26263=CARTESIAN_POINT('Ctrl Pts',(-39.9018404950872,36.7158470274101,38.8256238047931));
#26264=CARTESIAN_POINT('Ctrl Pts',(-39.9513044433358,36.7616156245003,38.8856677532216));
#26265=CARTESIAN_POINT('Ctrl Pts',(-39.9999204445307,36.80948954522,38.9448052723487));
#26266=CARTESIAN_POINT('Ctrl Pts',(-40.0476172992077,36.8593986646901,39.0029497519172));
#26267=CARTESIAN_POINT('Ctrl Pts',(-40.0953141538847,36.9093077841602,39.0610942314857));
#26268=CARTESIAN_POINT('Ctrl Pts',(-40.1420918484084,36.9612520881088,39.1182456548728));
#26269=CARTESIAN_POINT('Ctrl Pts',(-40.1878818744981,37.0151554935858,39.1743203193843));
#26270=CARTESIAN_POINT('Ctrl Pts',(-40.2336719005877,37.0690588990627,39.2303949838959));
#26271=CARTESIAN_POINT('Ctrl Pts',(-40.2784742451523,37.1249213906555,39.2853928735001));
#26272=CARTESIAN_POINT('Ctrl Pts',(-40.3222232915804,37.1826611500204,39.3392334380224));
#26273=CARTESIAN_POINT('Ctrl Pts',(-37.6288986882551,36.1098451974354,36.2155645638857));
#26274=CARTESIAN_POINT('Ctrl Pts',(-37.6877397713873,36.092877953765,36.2839383179962));
#26275=CARTESIAN_POINT('Ctrl Pts',(-37.7468320665581,36.078394354814,36.3527121922699));
#26276=CARTESIAN_POINT('Ctrl Pts',(-37.8060859993744,36.0664163519574,36.4217819364555));
#26277=CARTESIAN_POINT('Ctrl Pts',(-37.8652873174493,36.0544489850114,36.4907903499148));
#26278=CARTESIAN_POINT('Ctrl Pts',(-37.9246499681569,36.0449827700856,36.5600940869988));
#26279=CARTESIAN_POINT('Ctrl Pts',(-37.9840841272394,36.0380320309295,36.6295882811515));
#26280=CARTESIAN_POINT('Ctrl Pts',(-38.043518286322,36.0310812917733,36.6990824753041));
#26281=CARTESIAN_POINT('Ctrl Pts',(-38.1030239356216,36.0266460305104,36.7687671052939));
#26282=CARTESIAN_POINT('Ctrl Pts',(-38.1625110345032,36.0247329583309,36.8385367282189));
#26283=CARTESIAN_POINT('Ctrl Pts',(-38.2219981333846,36.0228198861515,36.9083063511438));
#26284=CARTESIAN_POINT('Ctrl Pts',(-38.2814666636739,36.02342900364,36.9781609456884));
#26285=CARTESIAN_POINT('Ctrl Pts',(-38.340826640902,36.026559389114,37.0479948117696));
#26286=CARTESIAN_POINT('Ctrl Pts',(-38.4001866181302,36.0296897745879,37.1178286778509));
#26287=CARTESIAN_POINT('Ctrl Pts',(-38.459438024162,36.0353414270909,37.1876417941335));
#26288=CARTESIAN_POINT('Ctrl Pts',(-38.518491203069,36.0435057948568,37.2573285232974));
#26289=CARTESIAN_POINT('Ctrl Pts',(-38.577544381976,36.0516701626229,37.3270152524612));
#26290=CARTESIAN_POINT('Ctrl Pts',(-38.6363993157166,36.0623472431577,37.3965755732159));
#26291=CARTESIAN_POINT('Ctrl Pts',(-38.6949669482823,36.0755208804975,37.4659042307574));
#26292=CARTESIAN_POINT('Ctrl Pts',(-38.7535345808479,36.0886945178373,37.5352328882988));
#26293=CARTESIAN_POINT('Ctrl Pts',(-38.8118148943452,36.1043647079574,37.604329861446));
#26294=CARTESIAN_POINT('Ctrl Pts',(-38.869719702249,36.1225077395987,37.6730905965066));
#26295=CARTESIAN_POINT('Ctrl Pts',(-38.9276245101529,36.1406507712399,37.7418513315672));
#26296=CARTESIAN_POINT('Ctrl Pts',(-38.9851537947725,36.1612666388593,37.810275807534));
#26297=CARTESIAN_POINT('Ctrl Pts',(-39.0422205059976,36.1843241476738,37.8782604882997));
#26298=CARTESIAN_POINT('Ctrl Pts',(-39.0992872172227,36.2073816564885,37.9462451690653));
#26299=CARTESIAN_POINT('Ctrl Pts',(-39.1558913376187,36.2328807994539,38.0137900338597));
#26300=CARTESIAN_POINT('Ctrl Pts',(-39.2119472169822,36.2607829926868,38.0807928775543));
#26301=CARTESIAN_POINT('Ctrl Pts',(-39.2680030963459,36.2886851859197,38.1477957212488));
#26302=CARTESIAN_POINT('Ctrl Pts',(-39.3235107175512,36.3189904208956,38.2142565233733));
#26303=CARTESIAN_POINT('Ctrl Pts',(-39.3783860895567,36.3516528414203,38.2800747191427));
#26304=CARTESIAN_POINT('Ctrl Pts',(-39.4332614615622,36.384315261945,38.3458929149119));
#26305=CARTESIAN_POINT('Ctrl Pts',(-39.4875045676025,36.4193348580397,38.4110684842176));
#26306=CARTESIAN_POINT('Ctrl Pts',(-39.54103333003,36.4566586400015,38.4755028070172));
#26307=CARTESIAN_POINT('Ctrl Pts',(-39.5945620924575,36.4939824219634,38.5399371298167));
#26308=CARTESIAN_POINT('Ctrl Pts',(-39.6473764949183,36.5336103783894,38.6036301864247));
#26309=CARTESIAN_POINT('Ctrl Pts',(-39.6993966215995,36.5754825464625,38.6664856000542));
#26310=CARTESIAN_POINT('Ctrl Pts',(-39.7514167482806,36.6173547145356,38.7293410136837));
#26311=CARTESIAN_POINT('Ctrl Pts',(-39.8026425832891,36.6614710814631,38.7913587651315));
#26312=CARTESIAN_POINT('Ctrl Pts',(-39.8529966145439,36.7077648928152,38.8524450125895));
#26313=CARTESIAN_POINT('Ctrl Pts',(-39.9033506457986,36.7540587041673,38.9135312600474));
#26314=CARTESIAN_POINT('Ctrl Pts',(-39.9528328579157,36.8025299458004,38.9736859848527));
#26315=CARTESIAN_POINT('Ctrl Pts',(-40.0013683771669,36.8531052737307,39.0328181642253));
#26316=CARTESIAN_POINT('Ctrl Pts',(-40.0499038964181,36.9036806016611,39.0919503435978));
#26317=CARTESIAN_POINT('Ctrl Pts',(-40.0974927079752,36.9563600004371,39.1500599594719));
#26318=CARTESIAN_POINT('Ctrl Pts',(-40.1440628030983,37.0110637585259,39.2070590836124));
#26319=CARTESIAN_POINT('Ctrl Pts',(-40.1906328982213,37.0657675166147,39.2640582077529));
#26320=CARTESIAN_POINT('Ctrl Pts',(-40.2361842626827,37.1224956173034,39.3199468227458));
#26321=CARTESIAN_POINT('Ctrl Pts',(-40.2806479706938,37.1811622227888,39.3746403610508));
#26322=CARTESIAN_POINT('Ctrl Pts',(-37.4555694438967,36.1325088746638,36.1837137166787));
#26323=CARTESIAN_POINT('Ctrl Pts',(-37.516031203023,36.1124990792145,36.2538292710476));
#26324=CARTESIAN_POINT('Ctrl Pts',(-37.5768056423164,36.0951168686426,36.3244221349243));
#26325=CARTESIAN_POINT('Ctrl Pts',(-37.6377949822143,36.0803899738306,36.3953787188787));
#26326=CARTESIAN_POINT('Ctrl Pts',(-37.6987301664097,36.0656761558176,36.4662722966806));
#26327=CARTESIAN_POINT('Ctrl Pts',(-37.7598798488343,36.053612945021,36.5375289245917));
#26328=CARTESIAN_POINT('Ctrl Pts',(-37.8211458301736,36.0442194991441,36.6090341603408));
#26329=CARTESIAN_POINT('Ctrl Pts',(-37.882411811513,36.0348260532672,36.6805393960898));
#26330=CARTESIAN_POINT('Ctrl Pts',(-37.9437940707557,36.028102375448,36.7522932151489));
#26331=CARTESIAN_POINT('Ctrl Pts',(-38.0051940430043,36.02405906329,36.8241803865376));
#26332=CARTESIAN_POINT('Ctrl Pts',(-38.066594015253,36.020015751132,36.8960675579264));
#26333=CARTESIAN_POINT('Ctrl Pts',(-38.1280116794532,36.0186528059442,36.9680880569896));
#26334=CARTESIAN_POINT('Ctrl Pts',(-38.1893484206806,36.0199722318693,37.0401262329843));
#26335=CARTESIAN_POINT('Ctrl Pts',(-38.2506851619081,36.0212916577943,37.112164408979));
#26336=CARTESIAN_POINT('Ctrl Pts',(-38.3119409591326,36.0252934543084,37.1842202372016));
#26337=CARTESIAN_POINT('Ctrl Pts',(-38.3730174631004,36.0319710262034,37.2561780174135));
#26338=CARTESIAN_POINT('Ctrl Pts',(-38.4340939670681,36.0386485980984,37.3281357976253));
#26339=CARTESIAN_POINT('Ctrl Pts',(-38.4949911568403,36.0480019430191,37.399995505153));
#26340=CARTESIAN_POINT('Ctrl Pts',(-38.5556112636636,36.0600158880042,37.471641760667));
#26341=CARTESIAN_POINT('Ctrl Pts',(-38.6162313704868,36.0720298329893,37.5432880161809));
#26342=CARTESIAN_POINT('Ctrl Pts',(-38.6765743735804,36.0867043738602,37.6147207951165));
#26343=CARTESIAN_POINT('Ctrl Pts',(-38.73654339765,36.1040158089172,37.6858254084132));
#26344=CARTESIAN_POINT('Ctrl Pts',(-38.7965124217196,36.1213272439742,37.75693002171));
#26345=CARTESIAN_POINT('Ctrl Pts',(-38.856107446209,36.1412755672286,37.8277064449908));
#26346=CARTESIAN_POINT('Ctrl Pts',(-38.9152327993705,36.1638286245175,37.8980410466006));
#26347=CARTESIAN_POINT('Ctrl Pts',(-38.974358152532,36.1863816818065,37.9683756482105));
#26348=CARTESIAN_POINT('Ctrl Pts',(-39.0330138140995,36.2115394653499,38.0382684040376));
#26349=CARTESIAN_POINT('Ctrl Pts',(-39.0911056220996,36.2392614718121,38.1076071035742));
#26350=CARTESIAN_POINT('Ctrl Pts',(-39.1491974300997,36.2669834782743,38.1769458031107));
#26351=CARTESIAN_POINT('Ctrl Pts',(-39.2067253646211,36.297269698109,38.245730422587));
#26352=CARTESIAN_POINT('Ctrl Pts',(-39.2635970748546,36.3300714087814,38.3138505318281));
#26353=CARTESIAN_POINT('Ctrl Pts',(-39.320468785088,36.3628731194539,38.3819706410691));
#26354=CARTESIAN_POINT('Ctrl Pts',(-39.3766842515407,36.3981903096824,38.449426216723));
#26355=CARTESIAN_POINT('Ctrl Pts',(-39.4321532301582,36.4359661939766,38.5161089624306));
#26356=CARTESIAN_POINT('Ctrl Pts',(-39.4876222087758,36.4737420782708,38.5827917081382));
#26357=CARTESIAN_POINT('Ctrl Pts',(-39.5423446805459,36.5139766436494,38.6487016010402));
#26358=CARTESIAN_POINT('Ctrl Pts',(-39.5962327970173,36.5566052236789,38.7137328252454));
#26359=CARTESIAN_POINT('Ctrl Pts',(-39.6501209134886,36.5992338037085,38.7787640494506));
#26360=CARTESIAN_POINT('Ctrl Pts',(-39.7031746561902,36.6442563837493,38.8429165826654));
#26361=CARTESIAN_POINT('Ctrl Pts',(-39.7553088534572,36.6916006236253,38.9060874281821));
#26362=CARTESIAN_POINT('Ctrl Pts',(-39.8074430507241,36.7389448635013,38.9692582736989));
#26363=CARTESIAN_POINT('Ctrl Pts',(-39.8586576846856,36.7886107469615,39.0314474098607));
#26364=CARTESIAN_POINT('Ctrl Pts',(-39.9088705330851,36.8405184918122,39.0925549888413));
#26365=CARTESIAN_POINT('Ctrl Pts',(-39.9590833814847,36.8924262366629,39.153662567822));
#26366=CARTESIAN_POINT('Ctrl Pts',(-40.0082944271086,36.946575825094,39.2136885686702));
#26367=CARTESIAN_POINT('Ctrl Pts',(-40.0564246602987,37.0028802884064,39.2725366120686));
#26368=CARTESIAN_POINT('Ctrl Pts',(-40.1045548934888,37.0591847517187,39.3313846554671));
#26369=CARTESIAN_POINT('Ctrl Pts',(-40.1516042977434,37.1176440705994,39.3890547212372));
#26370=CARTESIAN_POINT('Ctrl Pts',(-40.1974973289207,37.1781643683257,39.4454542071075));
#26371=CARTESIAN_POINT('Ctrl Pts',(-37.2861893607158,36.1599896970836,36.1561835957183));
#26372=CARTESIAN_POINT('Ctrl Pts',(-37.3481189647613,36.1368261638688,36.2278671181891));
#26373=CARTESIAN_POINT('Ctrl Pts',(-37.4104295575346,36.116431223471,36.3001131071893));
#26374=CARTESIAN_POINT('Ctrl Pts',(-37.4730148236326,36.0988394102363,36.3727982828643));
#26375=CARTESIAN_POINT('Ctrl Pts',(-37.5355445169199,36.081263217715,36.4454189174777));
#26376=CARTESIAN_POINT('Ctrl Pts',(-37.598348371835,36.066485183133,36.5184779311402));
#26377=CARTESIAN_POINT('Ctrl Pts',(-37.6613194336917,36.0545302334178,36.5918508930387));
#26378=CARTESIAN_POINT('Ctrl Pts',(-37.7242904955485,36.0425752837025,36.6652238549373));
#26379=CARTESIAN_POINT('Ctrl Pts',(-37.7874287400627,36.0334434233531,36.7389107367709));
#26380=CARTESIAN_POINT('Ctrl Pts',(-37.8506266534105,36.0271499800832,36.8127860511375));
#26381=CARTESIAN_POINT('Ctrl Pts',(-37.9138245667584,36.0208565368133,36.886661365504));
#26382=CARTESIAN_POINT('Ctrl Pts',(-37.9770821245729,36.0174015129466,36.9607250839144));
#26383=CARTESIAN_POINT('Ctrl Pts',(-38.0402916188546,36.0167905858017,37.0348510883942));
#26384=CARTESIAN_POINT('Ctrl Pts',(-38.1035011131364,36.0161796586568,37.1089770928739));
#26385=CARTESIAN_POINT('Ctrl Pts',(-38.166662519518,36.0184128283742,37.1831653548423));
#26386=CARTESIAN_POINT('Ctrl Pts',(-38.2296683014119,36.0234861033926,37.2572895538674));
#26387=CARTESIAN_POINT('Ctrl Pts',(-38.2926740833058,36.028559378411,37.3314137528924));
#26388=CARTESIAN_POINT('Ctrl Pts',(-38.3555242164265,36.0364727566876,37.4054738603985));
#26389=CARTESIAN_POINT('Ctrl Pts',(-38.4181117005737,36.0472125920524,37.4793437822614));
#26390=CARTESIAN_POINT('Ctrl Pts',(-38.480699184721,36.0579524274172,37.5532137041244));
#26391=CARTESIAN_POINT('Ctrl Pts',(-38.5430239957735,36.0715187156511,37.62689341187));
#26392=CARTESIAN_POINT('Ctrl Pts',(-38.6049800330493,36.087888202952,37.7002574656486));
#26393=CARTESIAN_POINT('Ctrl Pts',(-38.6669360703251,36.1042576902527,37.7736215194272));
#26394=CARTESIAN_POINT('Ctrl Pts',(-38.7285233099485,36.1234303702393,37.8466698909623));
#26395=CARTESIAN_POINT('Ctrl Pts',(-38.7896369108142,36.1453734609973,37.9192782203987));
#26396=CARTESIAN_POINT('Ctrl Pts',(-38.8507505116798,36.1673165517552,37.9918865498351));
#26397=CARTESIAN_POINT('Ctrl Pts',(-38.9113904502382,36.1920300447632,38.06405480919));
#26398=CARTESIAN_POINT('Ctrl Pts',(-38.9714535007296,36.2194717417869,38.1356601406378));
#26399=CARTESIAN_POINT('Ctrl Pts',(-39.0315165512211,36.2469134388106,38.2072654720858));
#26400=CARTESIAN_POINT('Ctrl Pts',(-39.0910026905017,36.2770833292175,38.2783078480319));
#26401=CARTESIAN_POINT('Ctrl Pts',(-39.1498106584341,36.3099299421387,38.3486663296049));
#26402=CARTESIAN_POINT('Ctrl Pts',(-39.2086186263666,36.3427765550599,38.4190248111778));
#26403=CARTESIAN_POINT('Ctrl Pts',(-39.2667484002909,36.3782998777878,38.488699371264));
#26404=CARTESIAN_POINT('Ctrl Pts',(-39.3241010292931,36.4164393419089,38.5575714003491));
#26405=CARTESIAN_POINT('Ctrl Pts',(-39.3814536582952,36.45457880603,38.6264434294343));
#26406=CARTESIAN_POINT('Ctrl Pts',(-39.438029120276,36.4953343968044,38.6945129009776));
#26407=CARTESIAN_POINT('Ctrl Pts',(-39.4937311093081,36.5386366541766,38.7616639373173));
#26408=CARTESIAN_POINT('Ctrl Pts',(-39.5494330983402,36.5819389115487,38.8288149736569));
#26409=CARTESIAN_POINT('Ctrl Pts',(-39.6042615929597,36.6277878187964,38.8950475489147));
#26410=CARTESIAN_POINT('Ctrl Pts',(-39.6581232590185,36.6761052602375,38.9602489105081));
#26411=CARTESIAN_POINT('Ctrl Pts',(-39.7119849250771,36.7244227016787,39.0254502721014));
#26412=CARTESIAN_POINT('Ctrl Pts',(-39.7648797418191,36.7752086586655,39.0896203949022));
#26413=CARTESIAN_POINT('Ctrl Pts',(-39.8167176635902,36.8283766252215,39.1526500340368));
#26414=CARTESIAN_POINT('Ctrl Pts',(-39.8685555853612,36.8815445917776,39.2156796731713));
#26415=CARTESIAN_POINT('Ctrl Pts',(-39.9193365921837,36.9370945473924,39.2775688043466));
#26416=CARTESIAN_POINT('Ctrl Pts',(-39.9689742324666,36.9949318895442,39.3382120611364));
#26417=CARTESIAN_POINT('Ctrl Pts',(-40.0186118727495,37.0527692316959,39.3988553179263));
#26418=CARTESIAN_POINT('Ctrl Pts',(-40.0671061273606,37.1128939380812,39.4582526769549));
#26419=CARTESIAN_POINT('Ctrl Pts',(-40.1143744321613,37.1752036308061,39.5163030078388));
#26420=CARTESIAN_POINT('Ctrl Pts',(-37.1201105829165,36.1914413355051,36.1322276221139));
#26421=CARTESIAN_POINT('Ctrl Pts',(-37.1833706680423,36.1650364607197,36.2053221084819));
#26422=CARTESIAN_POINT('Ctrl Pts',(-37.2470865241116,36.1415374300666,36.2790718308968));
#26423=CARTESIAN_POINT('Ctrl Pts',(-37.3111430442604,36.1209866911517,36.3533435554538));
#26424=CARTESIAN_POINT('Ctrl Pts',(-37.3751426851931,36.1004542003389,36.4275493301675));
#26425=CARTESIAN_POINT('Ctrl Pts',(-37.4394823577102,36.0828647766077,36.5022761482019));
#26426=CARTESIAN_POINT('Ctrl Pts',(-37.5040460348623,36.0682501398455,36.5773892509488));
#26427=CARTESIAN_POINT('Ctrl Pts',(-37.5686097120143,36.0536355030834,36.6525023536957));
#26428=CARTESIAN_POINT('Ctrl Pts',(-37.6333973657805,36.0419956596332,36.7280017085557));
#26429=CARTESIAN_POINT('Ctrl Pts',(-37.6982921613446,36.0333516002066,36.8037511637661));
#26430=CARTESIAN_POINT('Ctrl Pts',(-37.7631869569087,36.0247075407801,36.8795006189766));
#26431=CARTESIAN_POINT('Ctrl Pts',(-37.828188866106,36.0190592691289,36.9555001416619));
#26432=CARTESIAN_POINT('Ctrl Pts',(-37.8931806677428,36.0164169710636,37.031612678082));
#26433=CARTESIAN_POINT('Ctrl Pts',(-37.9581724693795,36.0137746729984,37.1077252145021));
#26434=CARTESIAN_POINT('Ctrl Pts',(-38.023154135249,36.014138349666,37.1839507316237));
#26435=CARTESIAN_POINT('Ctrl Pts',(-38.0880084806633,36.0175073452301,37.2601517681595));
#26436=CARTESIAN_POINT('Ctrl Pts',(-38.1528628260775,36.0208763407942,37.3363528046953));
#26437=CARTESIAN_POINT('Ctrl Pts',(-38.2175898228894,36.0272506537927,37.4125293275738));
#26438=CARTESIAN_POINT('Ctrl Pts',(-38.2820727456685,36.036618789108,37.4885439638614));
#26439=CARTESIAN_POINT('Ctrl Pts',(-38.3465556684475,36.0459869244234,37.564558600149));
#26440=CARTESIAN_POINT('Ctrl Pts',(-38.4107944892078,36.0583488779898,37.6404113168551));
#26441=CARTESIAN_POINT('Ctrl Pts',(-38.4746733628712,36.0736823568782,37.7159653249819));
#26442=CARTESIAN_POINT('Ctrl Pts',(-38.5385522365345,36.0890158357666,37.7915193331088));
#26443=CARTESIAN_POINT('Ctrl Pts',(-38.6020711353772,36.1073208333222,37.8667745998657));
#26444=CARTESIAN_POINT('Ctrl Pts',(-38.6651155125921,36.1285643392274,37.9415954136664));
#26445=CARTESIAN_POINT('Ctrl Pts',(-38.728159889807,36.1498078451326,38.016416227467));
#26446=CARTESIAN_POINT('Ctrl Pts',(-38.7907297180327,36.1739898501675,38.0908025558389));
#26447=CARTESIAN_POINT('Ctrl Pts',(-38.8527121619685,36.2010667457132,38.1646202541957));
#26448=CARTESIAN_POINT('Ctrl Pts',(-38.9146946059044,36.228143641259,38.2384379525525));
#26449=CARTESIAN_POINT('Ctrl Pts',(-38.9760896386497,36.2581154155639,38.3116869888571));
#26450=CARTESIAN_POINT('Ctrl Pts',(-39.0367865434716,36.2909280190285,38.384235269459));
#26451=CARTESIAN_POINT('Ctrl Pts',(-39.0974834482934,36.3237406224932,38.4567835500607));
#26452=CARTESIAN_POINT('Ctrl Pts',(-39.157482198849,36.3593940408766,38.5286310434735));
#26453=CARTESIAN_POINT('Ctrl Pts',(-39.2166745963907,36.3978239785864,38.599648183519));
#26454=CARTESIAN_POINT('Ctrl Pts',(-39.2758669939324,36.4362539162962,38.6706653235644));
#26455=CARTESIAN_POINT('Ctrl Pts',(-39.3342530127704,36.4774603566536,38.7408520794209));
#26456=CARTESIAN_POINT('Ctrl Pts',(-39.3917273624771,36.5213689900238,38.8100818798013));
#26457=CARTESIAN_POINT('Ctrl Pts',(-39.4492017121837,36.5652776233941,38.8793116801817));
#26458=CARTESIAN_POINT('Ctrl Pts',(-39.5057643678147,36.6118884307206,38.9475844950401));
#26459=CARTESIAN_POINT('Ctrl Pts',(-39.5613133271045,36.6611173564033,39.0147772045947));
#26460=CARTESIAN_POINT('Ctrl Pts',(-39.6168622863942,36.7103462820862,39.0819699141494));
#26461=CARTESIAN_POINT('Ctrl Pts',(-39.6713975252342,36.7621933047597,39.1480824892385));
#26462=CARTESIAN_POINT('Ctrl Pts',(-39.7248206975006,36.816564926095,39.2129957057488));
#26463=CARTESIAN_POINT('Ctrl Pts',(-39.7782438697671,36.8709365474302,39.2779089222591));
#26464=CARTESIAN_POINT('Ctrl Pts',(-39.8305549522741,36.9278327438297,39.3416227520181));
#26465=CARTESIAN_POINT('Ctrl Pts',(-39.8816596098305,36.9871509115369,39.40402229669));
#26466=CARTESIAN_POINT('Ctrl Pts',(-39.9327642673869,37.0464690792441,39.466421841362));
#26467=CARTESIAN_POINT('Ctrl Pts',(-39.982662477813,37.1082091925145,39.5275070738652));
#26468=CARTESIAN_POINT('Ctrl Pts',(-40.0312642571703,37.1722599123143,39.5871678361448));
#26469=CARTESIAN_POINT('Ctrl Pts',(-36.9540318051171,36.2228929739267,36.1082716485095));
#26470=CARTESIAN_POINT('Ctrl Pts',(-37.0186223713234,36.1932467575705,36.1827770987747));
#26471=CARTESIAN_POINT('Ctrl Pts',(-37.0837434906885,36.1666436366623,36.2580305546043));
#26472=CARTESIAN_POINT('Ctrl Pts',(-37.1492712648881,36.1431339720672,36.3338888280434));
#26473=CARTESIAN_POINT('Ctrl Pts',(-37.2147408534664,36.1196451829629,36.4096797428573));
#26474=CARTESIAN_POINT('Ctrl Pts',(-37.2806163435853,36.0992443700824,36.4860743652637));
#26475=CARTESIAN_POINT('Ctrl Pts',(-37.3467726360328,36.0819700462733,36.5629276088589));
#26476=CARTESIAN_POINT('Ctrl Pts',(-37.4129289284802,36.0646957224643,36.6397808524541));
#26477=CARTESIAN_POINT('Ctrl Pts',(-37.4793659914983,36.0505478959133,36.7170926803403));
#26478=CARTESIAN_POINT('Ctrl Pts',(-37.5459576692786,36.0395532203301,36.7947162763948));
#26479=CARTESIAN_POINT('Ctrl Pts',(-37.612549347059,36.0285585447468,36.8723398724492));
#26480=CARTESIAN_POINT('Ctrl Pts',(-37.6792956076391,36.020717025311,36.9502751994095));
#26481=CARTESIAN_POINT('Ctrl Pts',(-37.7460697166309,36.0160433563256,37.0283742677699));
#26482=CARTESIAN_POINT('Ctrl Pts',(-37.8128438256227,36.01136968734,37.1064733361303));
#26483=CARTESIAN_POINT('Ctrl Pts',(-37.87964575098,36.0098638709579,37.184736108405));
#26484=CARTESIAN_POINT('Ctrl Pts',(-37.9463486599146,36.0115285870677,37.2630139824516));
#26485=CARTESIAN_POINT('Ctrl Pts',(-38.0130515688492,36.0131933031775,37.3412918564982));
#26486=CARTESIAN_POINT('Ctrl Pts',(-38.0796554293524,36.0180285508978,37.4195847947491));
#26487=CARTESIAN_POINT('Ctrl Pts',(-38.1460337907632,36.0260249861637,37.4977441454614));
#26488=CARTESIAN_POINT('Ctrl Pts',(-38.212412152174,36.0340214214295,37.5759034961736));
#26489=CARTESIAN_POINT('Ctrl Pts',(-38.2785649826422,36.0451790403285,37.6539292218401));
#26490=CARTESIAN_POINT('Ctrl Pts',(-38.3443666926931,36.0594765108045,37.7316731843153));
#26491=CARTESIAN_POINT('Ctrl Pts',(-38.4101684027439,36.0737739812805,37.8094171467904));
#26492=CARTESIAN_POINT('Ctrl Pts',(-38.4756189608059,36.091211296405,37.8868793087691));
#26493=CARTESIAN_POINT('Ctrl Pts',(-38.5405941143701,36.1117552174574,37.963912606934));
#26494=CARTESIAN_POINT('Ctrl Pts',(-38.6055692679342,36.1322991385099,38.0409459050989));
#26495=CARTESIAN_POINT('Ctrl Pts',(-38.6700689858271,36.1559496555719,38.1175503024878));
#26496=CARTESIAN_POINT('Ctrl Pts',(-38.7339708232074,36.1826617496396,38.1935803677536));
#26497=CARTESIAN_POINT('Ctrl Pts',(-38.7978726605876,36.2093738437074,38.2696104330193));
#26498=CARTESIAN_POINT('Ctrl Pts',(-38.8611765867978,36.2391475019103,38.3450661296824));
#26499=CARTESIAN_POINT('Ctrl Pts',(-38.923762428509,36.2719260959184,38.419804209313));
#26500=CARTESIAN_POINT('Ctrl Pts',(-38.9863482702203,36.3047046899263,38.4945422889437));
#26501=CARTESIAN_POINT('Ctrl Pts',(-39.048215997407,36.3404882039654,38.5685627156829));
#26502=CARTESIAN_POINT('Ctrl Pts',(-39.1092481634882,36.379208615264,38.6417249666887));
#26503=CARTESIAN_POINT('Ctrl Pts',(-39.1702803295695,36.4179290265625,38.7148872176946));
#26504=CARTESIAN_POINT('Ctrl Pts',(-39.2304769052649,36.4595863165027,38.7871912578642));
#26505=CARTESIAN_POINT('Ctrl Pts',(-39.289723615646,36.5041013258711,38.8584998222854));
#26506=CARTESIAN_POINT('Ctrl Pts',(-39.3489703260272,36.5486163352394,38.9298083867066));
#26507=CARTESIAN_POINT('Ctrl Pts',(-39.4072671426698,36.5959890426447,39.0001214411655));
#26508=CARTESIAN_POINT('Ctrl Pts',(-39.4645033951906,36.6461294525692,39.0693054986814));
#26509=CARTESIAN_POINT('Ctrl Pts',(-39.5217396477114,36.6962698624937,39.1384895561974));
#26510=CARTESIAN_POINT('Ctrl Pts',(-39.5779153086493,36.7491779508538,39.2065445835747));
#26511=CARTESIAN_POINT('Ctrl Pts',(-39.6329237314111,36.8047532269684,39.2733413774608));
#26512=CARTESIAN_POINT('Ctrl Pts',(-39.6879321541729,36.8603285030829,39.3401381713469));
#26513=CARTESIAN_POINT('Ctrl Pts',(-39.7417733123646,36.918570940267,39.4056766996897));
#26514=CARTESIAN_POINT('Ctrl Pts',(-39.7943449871944,36.9793699335296,39.4698325322437));
#26515=CARTESIAN_POINT('Ctrl Pts',(-39.8469166620243,37.0401689267921,39.5339883647977));
#26516=CARTESIAN_POINT('Ctrl Pts',(-39.8982188282653,37.1035244469479,39.5967614707754));
#26517=CARTESIAN_POINT('Ctrl Pts',(-39.9481540821793,37.1693161938226,39.6580326644507));
#26518=CARTESIAN_POINT('Ctrl Pts',(-36.7912613073679,36.2583245548778,36.0878978700413));
#26519=CARTESIAN_POINT('Ctrl Pts',(-36.8570448313337,36.2253491798246,36.1636570993428));
#26520=CARTESIAN_POINT('Ctrl Pts',(-36.9234401661104,36.1955503975034,36.2402647180933));
#26521=CARTESIAN_POINT('Ctrl Pts',(-36.9903143661334,36.1689875916672,36.3175673204643));
#26522=CARTESIAN_POINT('Ctrl Pts',(-37.0571291849714,36.1424483723694,36.394801281713));
#26523=CARTESIAN_POINT('Ctrl Pts',(-37.1244219834839,36.1191393992778,36.472728951828));
#26524=CARTESIAN_POINT('Ctrl Pts',(-37.1920582731525,36.0991070017637,36.5511945771713));
#26525=CARTESIAN_POINT('Ctrl Pts',(-37.259694562821,36.0790746042497,36.6296602025146));
#26526=CARTESIAN_POINT('Ctrl Pts',(-37.327674307687,36.062318792826,36.7086637413645));
#26527=CARTESIAN_POINT('Ctrl Pts',(-37.3958616587387,36.0488728169132,36.7880473051252));
#26528=CARTESIAN_POINT('Ctrl Pts',(-37.4640490097905,36.0354268410005,36.8674308688859));
#26529=CARTESIAN_POINT('Ctrl Pts',(-37.5324439307829,36.0252907076194,36.9471944153556));
#26530=CARTESIAN_POINT('Ctrl Pts',(-37.6009097538766,36.0184844547042,37.0271785505671));
#26531=CARTESIAN_POINT('Ctrl Pts',(-37.6693755769703,36.0116782017889,37.1071626857786));
#26532=CARTESIAN_POINT('Ctrl Pts',(-37.7379122657777,36.0082018328405,37.1873673672181));
#26533=CARTESIAN_POINT('Ctrl Pts',(-37.8063828785137,36.0080620953735,37.2676323310766));
#26534=CARTESIAN_POINT('Ctrl Pts',(-37.8748534912497,36.0079223579063,37.3478972949351));
#26535=CARTESIAN_POINT('Ctrl Pts',(-37.9432579915291,36.0111192518882,37.4282224985554));
#26536=CARTESIAN_POINT('Ctrl Pts',(-38.0114597095541,36.0176462083918,37.5084474472333));
#26537=CARTESIAN_POINT('Ctrl Pts',(-38.079661427579,36.0241731648953,37.5886723959111));
#26538=CARTESIAN_POINT('Ctrl Pts',(-38.1476603271114,36.0340301803553,37.6687970470156));
#26539=CARTESIAN_POINT('Ctrl Pts',(-38.2153205551546,36.0471973963919,37.7486613147697));
#26540=CARTESIAN_POINT('Ctrl Pts',(-38.2829807831979,36.0603646124286,37.8285255825238));
#26541=CARTESIAN_POINT('Ctrl Pts',(-38.3503023038048,36.0768420219581,37.9081294244924));
#26542=CARTESIAN_POINT('Ctrl Pts',(-38.4171506223099,36.0965965570376,37.9873138019821));
#26543=CARTESIAN_POINT('Ctrl Pts',(-38.483998940815,36.1163510921171,38.0664981794718));
#26544=CARTESIAN_POINT('Ctrl Pts',(-38.5503740217048,36.1393827421724,38.1452630504119));
#26545=CARTESIAN_POINT('Ctrl Pts',(-38.6161432647377,36.1656453621667,38.223451057146));
#26546=CARTESIAN_POINT('Ctrl Pts',(-38.6819125077707,36.1919079821609,38.3016390638801));
#26547=CARTESIAN_POINT('Ctrl Pts',(-38.7470758780082,36.2214015580719,38.3792501648692));
#26548=CARTESIAN_POINT('Ctrl Pts',(-38.8115031981583,36.2540670522875,38.4561293107248));
#26549=CARTESIAN_POINT('Ctrl Pts',(-38.8759305183084,36.286732546503,38.5330084565804));
#26550=CARTESIAN_POINT('Ctrl Pts',(-38.9396217541463,36.3225699416089,38.6091556064603));
#26551=CARTESIAN_POINT('Ctrl Pts',(-39.0024496701877,36.361507543251,38.6844186372596));
#26552=CARTESIAN_POINT('Ctrl Pts',(-39.0652775862291,36.400445144893,38.759681668059));
#26553=CARTESIAN_POINT('Ctrl Pts',(-39.1272421490989,36.4424829323341,38.8340605397946));
#26554=CARTESIAN_POINT('Ctrl Pts',(-39.1882195722495,36.4875368406862,38.9074066619901));
#26555=CARTESIAN_POINT('Ctrl Pts',(-39.2491969954,36.5325907490382,38.9807527841855));
#26556=CARTESIAN_POINT('Ctrl Pts',(-39.3091872464385,36.5806607543238,39.0530661178757));
#26557=CARTESIAN_POINT('Ctrl Pts',(-39.3680704811376,36.6316507565641,39.1242021974759));
#26558=CARTESIAN_POINT('Ctrl Pts',(-39.4269537158367,36.6826407588044,39.1953382770762));
#26559=CARTESIAN_POINT('Ctrl Pts',(-39.4847299029149,36.736550730877,39.2652970647943));
#26560=CARTESIAN_POINT('Ctrl Pts',(-39.5412836181438,36.7932729210564,39.3339387957669));
#26561=CARTESIAN_POINT('Ctrl Pts',(-39.5978373333727,36.8499951112357,39.4025805267396));
#26562=CARTESIAN_POINT('Ctrl Pts',(-39.6531685467061,36.9095294893625,39.4699051644974));
#26563=CARTESIAN_POINT('Ctrl Pts',(-39.7071667139898,36.9717570816839,39.5357782020048));
#26564=CARTESIAN_POINT('Ctrl Pts',(-39.7611648812735,37.0339846740053,39.6016512395122));
#26565=CARTESIAN_POINT('Ctrl Pts',(-39.8138299738162,37.098905447445,39.6660726417677));
#26566=CARTESIAN_POINT('Ctrl Pts',(-39.8650567681803,37.1663896806103,39.7289136957327));
#26567=CARTESIAN_POINT('Ctrl Pts',(-36.6313596335673,36.2971547767807,36.0705950037057));
#26568=CARTESIAN_POINT('Ctrl Pts',(-36.6982091283211,36.260779871097,36.1474619304646));
#26569=CARTESIAN_POINT('Ctrl Pts',(-36.7657578569626,36.2277105354781,36.2252849626787));
#26570=CARTESIAN_POINT('Ctrl Pts',(-36.8338636442589,36.1980163667922,36.3039002996823));
#26571=CARTESIAN_POINT('Ctrl Pts',(-36.9019089567779,36.1683485651496,36.3824458299163));
#26572=CARTESIAN_POINT('Ctrl Pts',(-36.9705102990142,36.1420499565984,36.4617822122257));
#26573=CARTESIAN_POINT('Ctrl Pts',(-37.0395235375808,36.1191757952692,36.5417427585964));
#26574=CARTESIAN_POINT('Ctrl Pts',(-37.1085367761474,36.09630163394,36.6217033049671));
#26575=CARTESIAN_POINT('Ctrl Pts',(-37.1779618703816,36.0768519333104,36.7022879682863));
#26576=CARTESIAN_POINT('Ctrl Pts',(-37.2476529561698,36.0608675577589,36.7833274378659));
#26577=CARTESIAN_POINT('Ctrl Pts',(-37.3173440419582,36.0448831822074,36.8643669074455));
#26578=CARTESIAN_POINT('Ctrl Pts',(-37.3873010782385,36.0323641411522,36.9458611355369));
#26579=CARTESIAN_POINT('Ctrl Pts',(-37.4573770832718,36.0233367374574,37.0276389004303));
#26580=CARTESIAN_POINT('Ctrl Pts',(-37.5274530883051,36.0143093337625,37.1094166653237));
#26581=CARTESIAN_POINT('Ctrl Pts',(-37.5976480208025,36.008773572747,37.1914779188356));
#26582=CARTESIAN_POINT('Ctrl Pts',(-37.6678143991983,36.0067410852035,37.2736502479195));
#26583=CARTESIAN_POINT('Ctrl Pts',(-37.7379807775941,36.00470859766,37.3558225770034));
#26584=CARTESIAN_POINT('Ctrl Pts',(-37.8081185605461,36.0061793847861,37.4381059332432));
#26585=CARTESIAN_POINT('Ctrl Pts',(-37.8780803865613,36.0111503564157,37.5203274369483));
#26586=CARTESIAN_POINT('Ctrl Pts',(-37.9480422125766,36.0161213280453,37.6025489406534));
#26587=CARTESIAN_POINT('Ctrl Pts',(-38.0178280404336,36.0245924812496,37.6847085433788));
#26588=CARTESIAN_POINT('Ctrl Pts',(-38.087291248107,36.0365460178929,37.7666336254434));
#26589=CARTESIAN_POINT('Ctrl Pts',(-38.1567544557805,36.0484995545361,37.8485587075081));
#26590=CARTESIAN_POINT('Ctrl Pts',(-38.2258950023425,36.0639354675753,37.9302492206416));
#26591=CARTESIAN_POINT('Ctrl Pts',(-38.2945676215226,36.0828213257145,38.0115335307338));
#26592=CARTESIAN_POINT('Ctrl Pts',(-38.3632402407026,36.1017071838536,38.092817840826));
#26593=CARTESIAN_POINT('Ctrl Pts',(-38.4314448920386,36.1240429759653,38.173695899984));
#26594=CARTESIAN_POINT('Ctrl Pts',(-38.4990382756025,36.1497817739097,38.2539977810866));
#26595=CARTESIAN_POINT('Ctrl Pts',(-38.5666316591664,36.1755205718542,38.3342996621892));
#26596=CARTESIAN_POINT('Ctrl Pts',(-38.6336137351323,36.2046623604661,38.4140253179224));
#26597=CARTESIAN_POINT('Ctrl Pts',(-38.6998437722378,36.2371459120121,38.4930072423977));
#26598=CARTESIAN_POINT('Ctrl Pts',(-38.7660738093433,36.2696294635582,38.571989166873));
#26599=CARTESIAN_POINT('Ctrl Pts',(-38.8315517685658,36.3054547588989,38.6502273135541));
#26600=CARTESIAN_POINT('Ctrl Pts',(-38.8961400788355,36.3445465280617,38.7275573018515));
#26601=CARTESIAN_POINT('Ctrl Pts',(-38.9607283891053,36.3836382972244,38.8048872901491));
#26602=CARTESIAN_POINT('Ctrl Pts',(-39.0244270123667,36.4259965171763,38.8813090745));
#26603=CARTESIAN_POINT('Ctrl Pts',(-39.087102115986,36.4715321920828,38.9566620905444));
#26604=CARTESIAN_POINT('Ctrl Pts',(-39.1497772196053,36.5170678669892,39.0320151065888));
#26605=CARTESIAN_POINT('Ctrl Pts',(-39.2114287666543,36.5657809700204,39.1062993099285));
#26606=CARTESIAN_POINT('Ctrl Pts',(-39.2719272254649,36.6175691535503,39.1793586273225));
#26607=CARTESIAN_POINT('Ctrl Pts',(-39.3324256842755,36.6693573370803,39.2524179447164));
#26608=CARTESIAN_POINT('Ctrl Pts',(-39.3917710192021,36.7242205705952,39.324252333118));
#26609=CARTESIAN_POINT('Ctrl Pts',(-39.4498385439942,36.7820435848685,39.3947108664176));
#26610=CARTESIAN_POINT('Ctrl Pts',(-39.5079060687864,36.8398665991418,39.4651693997171));
#26611=CARTESIAN_POINT('Ctrl Pts',(-39.5646957492308,36.9006493601041,39.5342520364003));
#26612=CARTESIAN_POINT('Ctrl Pts',(-39.6200882685805,36.9642641614319,39.6018136318669));
#26613=CARTESIAN_POINT('Ctrl Pts',(-39.6754807879302,37.0278789627596,39.6693752273335));
#26614=CARTESIAN_POINT('Ctrl Pts',(-39.7294761135479,37.0943257669709,39.7354157417759));
#26615=CARTESIAN_POINT('Ctrl Pts',(-39.7819607997063,37.1634649674249,39.79979642218));
#26616=CARTESIAN_POINT('Ctrl Pts',(-36.4714579597666,36.3359849986837,36.0532921373701));
#26617=CARTESIAN_POINT('Ctrl Pts',(-36.5393734253084,36.2962105623695,36.1312667615863));
#26618=CARTESIAN_POINT('Ctrl Pts',(-36.6080755478147,36.2598706734529,36.2103052072641));
#26619=CARTESIAN_POINT('Ctrl Pts',(-36.6774129223844,36.2270451419173,36.2902332789004));
#26620=CARTESIAN_POINT('Ctrl Pts',(-36.7466887285845,36.1942487579297,36.3700903781196));
#26621=CARTESIAN_POINT('Ctrl Pts',(-36.8165986145445,36.1649605139189,36.4508354726234));
#26622=CARTESIAN_POINT('Ctrl Pts',(-36.8869888020091,36.1392445887747,36.5322909400215));
#26623=CARTESIAN_POINT('Ctrl Pts',(-36.9573789894737,36.1135286636304,36.6137464074195));
#26624=CARTESIAN_POINT('Ctrl Pts',(-37.0282494330761,36.0913850737948,36.6959121952081));
#26625=CARTESIAN_POINT('Ctrl Pts',(-37.099444253601,36.0728622986046,36.7786075706066));
#26626=CARTESIAN_POINT('Ctrl Pts',(-37.1706390741258,36.0543395234144,36.8613029460051));
#26627=CARTESIAN_POINT('Ctrl Pts',(-37.242158225694,36.0394375746849,36.9445278557182));
#26628=CARTESIAN_POINT('Ctrl Pts',(-37.3138444126669,36.0281890202105,37.0280992502935));
#26629=CARTESIAN_POINT('Ctrl Pts',(-37.3855305996398,36.0169404657361,37.1116706448688));
#26630=CARTESIAN_POINT('Ctrl Pts',(-37.4573837758273,36.0093453126535,37.1955884704532));
#26631=CARTESIAN_POINT('Ctrl Pts',(-37.5292459198829,36.0054200750336,37.2796681647624));
#26632=CARTESIAN_POINT('Ctrl Pts',(-37.6011080639385,36.0014948374137,37.3637478590717));
#26633=CARTESIAN_POINT('Ctrl Pts',(-37.6729791295631,36.001239517684,37.4479893679309));
#26634=CARTESIAN_POINT('Ctrl Pts',(-37.7447010635687,36.0046545044396,37.5322074266633));
#26635=CARTESIAN_POINT('Ctrl Pts',(-37.8164229975742,36.0080694911953,37.6164254853956));
#26636=CARTESIAN_POINT('Ctrl Pts',(-37.8879957537558,36.015154782144,37.7006200397419));
#26637=CARTESIAN_POINT('Ctrl Pts',(-37.9592619410594,36.0258946393938,37.7846059361171));
#26638=CARTESIAN_POINT('Ctrl Pts',(-38.030528128363,36.0366344966437,37.8685918324923));
#26639=CARTESIAN_POINT('Ctrl Pts',(-38.1014877008803,36.0510289131925,37.9523690167908));
#26640=CARTESIAN_POINT('Ctrl Pts',(-38.1719846207352,36.0690460943914,38.0357532594855));
#26641=CARTESIAN_POINT('Ctrl Pts',(-38.2424815405902,36.0870632755903,38.1191375021802));
#26642=CARTESIAN_POINT('Ctrl Pts',(-38.3125157623724,36.1087032097581,38.2021287495561));
#26643=CARTESIAN_POINT('Ctrl Pts',(-38.3819332864673,36.1339181856529,38.2845445050272));
#26644=CARTESIAN_POINT('Ctrl Pts',(-38.4513508105622,36.1591331615475,38.3669602604983));
#26645=CARTESIAN_POINT('Ctrl Pts',(-38.5201515922563,36.1879231628604,38.4488004709756));
#26646=CARTESIAN_POINT('Ctrl Pts',(-38.5881843463173,36.2202247717368,38.5298851740706));
#26647=CARTESIAN_POINT('Ctrl Pts',(-38.6562171003783,36.2525263806133,38.6109698771655));
#26648=CARTESIAN_POINT('Ctrl Pts',(-38.7234817829854,36.2883395761889,38.6912990206478));
#26649=CARTESIAN_POINT('Ctrl Pts',(-38.7898304874834,36.3275855128724,38.7706959664435));
#26650=CARTESIAN_POINT('Ctrl Pts',(-38.8561791919814,36.3668314495559,38.8500929122391));
#26651=CARTESIAN_POINT('Ctrl Pts',(-38.9216118756344,36.4095101020185,38.9285576092055));
#26652=CARTESIAN_POINT('Ctrl Pts',(-38.9859846597225,36.4555275434794,39.0059175190987));
#26653=CARTESIAN_POINT('Ctrl Pts',(-39.0503574438107,36.5015449849401,39.083277428992));
#26654=CARTESIAN_POINT('Ctrl Pts',(-39.1136702868701,36.550901185717,39.1595325019814));
#26655=CARTESIAN_POINT('Ctrl Pts',(-39.1757839697923,36.6034875505365,39.234515057169));
#26656=CARTESIAN_POINT('Ctrl Pts',(-39.2378976527144,36.6560739153561,39.3094976123567));
#26657=CARTESIAN_POINT('Ctrl Pts',(-39.2988121354892,36.7118904103133,39.3832076014418));
#26658=CARTESIAN_POINT('Ctrl Pts',(-39.3583934698447,36.7708142486806,39.4554829370682));
#26659=CARTESIAN_POINT('Ctrl Pts',(-39.4179748042001,36.829738087048,39.5277582726946));
#26660=CARTESIAN_POINT('Ctrl Pts',(-39.4762229517554,36.8917692308458,39.5985989083033));
#26661=CARTESIAN_POINT('Ctrl Pts',(-39.5330098231711,36.9567712411799,39.6678490617289));
#26662=CARTESIAN_POINT('Ctrl Pts',(-39.5897966945868,37.021773251514,39.7370992151546));
#26663=CARTESIAN_POINT('Ctrl Pts',(-39.6451222532796,37.0897460864968,39.8047588417841));
#26664=CARTESIAN_POINT('Ctrl Pts',(-39.6988648312323,37.1605402542396,39.8706791486274));
#26665=CARTESIAN_POINT('Ctrl Pts',(-36.3144288446909,36.3782187397976,36.0390644866415));
#26666=CARTESIAN_POINT('Ctrl Pts',(-36.3832832065462,36.3349742844667,36.1180006296823));
#26667=CARTESIAN_POINT('Ctrl Pts',(-36.4530178150635,36.2952888355839,36.1981156434926));
#26668=CARTESIAN_POINT('Ctrl Pts',(-36.523471853133,36.2592536063736,36.2792247606169));
#26669=CARTESIAN_POINT('Ctrl Pts',(-36.5938633312875,36.2232503747738,36.3602618566107));
#26670=CARTESIAN_POINT('Ctrl Pts',(-36.6649729122354,36.1908909085033,36.4422912340599));
#26671=CARTESIAN_POINT('Ctrl Pts',(-36.7366369171835,36.1622494193356,36.5251240689158));
#26672=CARTESIAN_POINT('Ctrl Pts',(-36.8083009221317,36.1336079301679,36.6079569037717));
#26673=CARTESIAN_POINT('Ctrl Pts',(-36.8805193005059,36.108684438148,36.6915931375718));
#26674=CARTESIAN_POINT('Ctrl Pts',(-36.9531258359889,36.0875360567009,36.7758402656948));
#26675=CARTESIAN_POINT('Ctrl Pts',(-37.025732371472,36.0663876752538,36.8600873938177));
#26676=CARTESIAN_POINT('Ctrl Pts',(-37.0987270128334,36.0490144191481,36.9449453568138));
#26677=CARTESIAN_POINT('Ctrl Pts',(-37.171941769992,36.0354560422844,37.0302188540894));
#26678=CARTESIAN_POINT('Ctrl Pts',(-37.2451565271507,36.0218976654207,37.1154923513651));
#26679=CARTESIAN_POINT('Ctrl Pts',(-37.3185913484547,36.0121541772235,37.2011813227561));
#26680=CARTESIAN_POINT('Ctrl Pts',(-37.392077241905,36.0062477905694,37.2870885690652));
#26681=CARTESIAN_POINT('Ctrl Pts',(-37.4655631353554,36.0003414039153,37.3729958153742));
#26682=CARTESIAN_POINT('Ctrl Pts',(-37.5391000491155,35.998272122842,37.4591212759982));
#26683=CARTESIAN_POINT('Ctrl Pts',(-37.612518765662,36.0000445182044,37.5452667591572));
#26684=CARTESIAN_POINT('Ctrl Pts',(-37.6859374822086,36.0018169135668,37.6314122423163));
#26685=CARTESIAN_POINT('Ctrl Pts',(-37.7592379497577,36.0074309839979,37.7175776872464));
#26686=CARTESIAN_POINT('Ctrl Pts',(-37.8322515026438,36.0168736382935,37.8035648201072));
#26687=CARTESIAN_POINT('Ctrl Pts',(-37.9052650555298,36.0263162925892,37.8895519529678));
#26688=CARTESIAN_POINT('Ctrl Pts',(-37.9779916422593,36.0395875239842,37.9753607131126));
#26689=CARTESIAN_POINT('Ctrl Pts',(-38.0502639238318,36.0566566402252,38.0607936554889));
#26690=CARTESIAN_POINT('Ctrl Pts',(-38.1225362054044,36.0737257564662,38.1462265978652));
#26691=CARTESIAN_POINT('Ctrl Pts',(-38.1943541308527,36.0945927454211,38.2312836622219));
#26692=CARTESIAN_POINT('Ctrl Pts',(-38.2655524565242,36.1192094555603,38.3157691392955));
#26693=CARTESIAN_POINT('Ctrl Pts',(-38.3367507821957,36.1438261656996,38.4002546163691));
#26694=CARTESIAN_POINT('Ctrl Pts',(-38.4073294578828,36.1721925795798,38.4841684465799));
#26695=CARTESIAN_POINT('Ctrl Pts',(-38.4771260943151,36.2042433082775,38.5673175554497));
#26696=CARTESIAN_POINT('Ctrl Pts',(-38.5469227307473,36.2362940369752,38.6504666643194));
#26697=CARTESIAN_POINT('Ctrl Pts',(-38.615937278707,36.2720290578162,38.732850993213));
#26698=CARTESIAN_POINT('Ctrl Pts',(-38.6840109492129,36.3113660454538,38.8142809893088));
#26699=CARTESIAN_POINT('Ctrl Pts',(-38.7520846197189,36.3507030330916,38.8957109854046));
#26700=CARTESIAN_POINT('Ctrl Pts',(-38.819217364769,36.3936419597249,38.9761865912809));
#26701=CARTESIAN_POINT('Ctrl Pts',(-38.8852547250341,36.4400839422626,39.0555226464555));
#26702=CARTESIAN_POINT('Ctrl Pts',(-38.9512920852992,36.4865259248002,39.1348587016301));
#26703=CARTESIAN_POINT('Ctrl Pts',(-39.0162340142127,36.5364709304417,39.2130551501577));
#26704=CARTESIAN_POINT('Ctrl Pts',(-39.0799310915729,36.5898039729972,39.2899320743992));
#26705=CARTESIAN_POINT('Ctrl Pts',(-39.1436281689332,36.6431370155525,39.3668089986409));
#26706=CARTESIAN_POINT('Ctrl Pts',(-39.2060803498222,36.6998580573726,39.442366344384));
#26707=CARTESIAN_POINT('Ctrl Pts',(-39.2671439395029,36.7598365376979,39.5164302632599));
#26708=CARTESIAN_POINT('Ctrl Pts',(-39.3282075291836,36.8198150180233,39.5904941821358));
#26709=CARTESIAN_POINT('Ctrl Pts',(-39.3878824845926,36.8830508945285,39.6630646219134));
#26710=CARTESIAN_POINT('Ctrl Pts',(-39.4460314965102,36.9493986318733,39.7339746020575));
#26711=CARTESIAN_POINT('Ctrl Pts',(-39.5041805084277,37.0157463692181,39.8048845822015));
#26712=CARTESIAN_POINT('Ctrl Pts',(-39.5608035358426,37.0852059205947,39.8741340527016));
#26713=CARTESIAN_POINT('Ctrl Pts',(-39.6157702857969,37.1576174447781,39.941563667896));
#26714=CARTESIAN_POINT('Ctrl Pts',(-36.1599632550759,36.423437812919,36.0275461720274));
#26715=CARTESIAN_POINT('Ctrl Pts',(-36.229636845075,36.376666560942,36.1073050568148));
#26716=CARTESIAN_POINT('Ctrl Pts',(-36.3002901628524,36.3335735174028,36.1883649632048));
#26717=CARTESIAN_POINT('Ctrl Pts',(-36.3717528702068,36.2942625662383,36.2705304633556));
#26718=CARTESIAN_POINT('Ctrl Pts',(-36.4431521219947,36.2549865213736,36.3526230043567));
#26719=CARTESIAN_POINT('Ctrl Pts',(-36.5153592713935,36.2194858855877,36.4358191130872));
#26720=CARTESIAN_POINT('Ctrl Pts',(-36.5882005448549,36.1878460946234,36.5199185699963));
#26721=CARTESIAN_POINT('Ctrl Pts',(-36.6610418183162,36.1562063036593,36.6040180269053));
#26722=CARTESIAN_POINT('Ctrl Pts',(-36.7345171595216,36.1284273819797,36.6890207669698));
#26723=CARTESIAN_POINT('Ctrl Pts',(-36.8084497428955,36.1045761822694,36.7747222228044));
#26724=CARTESIAN_POINT('Ctrl Pts',(-36.8823823262693,36.0807249825591,36.860423678639));
#26725=CARTESIAN_POINT('Ctrl Pts',(-36.9567720946492,36.060801523259,36.9468237839821));
#26726=CARTESIAN_POINT('Ctrl Pts',(-37.0314400218015,36.0448537521174,37.0337146085525));
#26727=CARTESIAN_POINT('Ctrl Pts',(-37.1061079489537,36.0289059809758,37.1206054331229));
#26728=CARTESIAN_POINT('Ctrl Pts',(-37.1810539771475,36.0169339103229,37.2079869097394));
#26729=CARTESIAN_POINT('Ctrl Pts',(-37.2560977414554,36.0089663521146,37.295648746355));
#26730=CARTESIAN_POINT('Ctrl Pts',(-37.3311415057632,36.0009987939063,37.3833105829706));
#26731=CARTESIAN_POINT('Ctrl Pts',(-37.4062829481639,35.9970357543028,37.471252711808));
#26732=CARTESIAN_POINT('Ctrl Pts',(-37.4813412334466,35.9970867707455,37.5592634915561));
#26733=CARTESIAN_POINT('Ctrl Pts',(-37.5563995187293,35.9971377871883,37.6472742713042));
#26734=CARTESIAN_POINT('Ctrl Pts',(-37.6313745888614,36.0012028596377,37.7353536339158));
#26735=CARTESIAN_POINT('Ctrl Pts',(-37.7060860090234,36.0092722051006,37.8232896078133));
#26736=CARTESIAN_POINT('Ctrl Pts',(-37.7807974291853,36.0173415505635,37.9112255817108));
#26737=CARTESIAN_POINT('Ctrl Pts',(-37.8552451416127,36.0294151628007,37.9990180989049));
#26738=CARTESIAN_POINT('Ctrl Pts',(-37.9292499806237,36.0454639854869,38.0864558781395));
#26739=CARTESIAN_POINT('Ctrl Pts',(-38.0032548196346,36.0615128081731,38.173893657374));
#26740=CARTESIAN_POINT('Ctrl Pts',(-38.076816728011,36.0815368288997,38.260976631045));
#26741=CARTESIAN_POINT('Ctrl Pts',(-38.1497586718448,36.1054878579077,38.3474952254818));
#26742=CARTESIAN_POINT('Ctrl Pts',(-38.2227006156786,36.1294388869157,38.4340138199186));
#26743=CARTESIAN_POINT('Ctrl Pts',(-38.2950225385736,36.1573169056868,38.519967968228));
#26744=CARTESIAN_POINT('Ctrl Pts',(-38.3665503907676,36.1890548230498,38.6051508133676));
#26745=CARTESIAN_POINT('Ctrl Pts',(-38.4380782429617,36.2207927404126,38.6903336585073));
#26746=CARTESIAN_POINT('Ctrl Pts',(-38.5088119691518,36.2563905318285,38.7747451346167));
#26747=CARTESIAN_POINT('Ctrl Pts',(-38.5785813417265,36.29576252774,38.8581820972448));
#26748=CARTESIAN_POINT('Ctrl Pts',(-38.6483507143011,36.3351345236515,38.941619059873));
#26749=CARTESIAN_POINT('Ctrl Pts',(-38.7171556793168,36.3782806936176,39.024081444509));
#26750=CARTESIAN_POINT('Ctrl Pts',(-38.7848306509137,36.4250972021714,39.1053707973808));
#26751=CARTESIAN_POINT('Ctrl Pts',(-38.8525056225106,36.4719137107252,39.1866601502525));
#26752=CARTESIAN_POINT('Ctrl Pts',(-38.9190505483647,36.5224005216697,39.2667764085097));
#26753=CARTESIAN_POINT('Ctrl Pts',(-38.9843052816209,36.57643613357,39.3455267645619));
#26754=CARTESIAN_POINT('Ctrl Pts',(-39.049560014877,36.6304717454703,39.4242771206141));
#26755=CARTESIAN_POINT('Ctrl Pts',(-39.1135245050824,36.6880561165477,39.5016615135742));
#26756=CARTESIAN_POINT('Ctrl Pts',(-39.1760448154521,36.749050664396,39.5774937103522));
#26757=CARTESIAN_POINT('Ctrl Pts',(-39.2385651258217,36.8100452122444,39.6533259071301));
#26758=CARTESIAN_POINT('Ctrl Pts',(-39.299641208017,36.8744498897049,39.727605849095));
#26759=CARTESIAN_POINT('Ctrl Pts',(-39.3591260764884,36.9421097006389,39.8001547743209));
#26760=CARTESIAN_POINT('Ctrl Pts',(-39.4186109449598,37.0097695115729,39.8727036995467));
#26761=CARTESIAN_POINT('Ctrl Pts',(-39.4765045537157,37.0806844036681,39.9435215519411));
#26762=CARTESIAN_POINT('Ctrl Pts',(-39.5326675761395,37.1546837133193,40.0124379014345));
#26763=CARTESIAN_POINT('Ctrl Pts',(-36.0054976654609,36.4686568860403,36.0160278574133));
#26764=CARTESIAN_POINT('Ctrl Pts',(-36.0759904836038,36.4183588374172,36.0966094839474));
#26765=CARTESIAN_POINT('Ctrl Pts',(-36.1475625106413,36.3718581992216,36.178614282917));
#26766=CARTESIAN_POINT('Ctrl Pts',(-36.2200338872806,36.3292715261031,36.2618361660942));
#26767=CARTESIAN_POINT('Ctrl Pts',(-36.2924409127019,36.2867226679733,36.3449841521028));
#26768=CARTESIAN_POINT('Ctrl Pts',(-36.3657456305516,36.248080862672,36.4293469921147));
#26769=CARTESIAN_POINT('Ctrl Pts',(-36.4397641725262,36.2134427699113,36.5147130710767));
#26770=CARTESIAN_POINT('Ctrl Pts',(-36.5137827145008,36.1788046771507,36.6000791500389));
#26771=CARTESIAN_POINT('Ctrl Pts',(-36.5885150185374,36.1481703258115,36.6864483963677));
#26772=CARTESIAN_POINT('Ctrl Pts',(-36.663773649802,36.121616307838,36.773604179914));
#26773=CARTESIAN_POINT('Ctrl Pts',(-36.7390322810665,36.0950622898643,36.8607599634603));
#26774=CARTESIAN_POINT('Ctrl Pts',(-36.8148171764651,36.07258862737,36.9487022111505));
#26775=CARTESIAN_POINT('Ctrl Pts',(-36.8909382736109,36.0542514619504,37.0372103630156));
#26776=CARTESIAN_POINT('Ctrl Pts',(-36.9670593707568,36.0359142965309,37.1257185148807));
#26777=CARTESIAN_POINT('Ctrl Pts',(-37.0435166058402,36.0217136434224,37.2147924967226));
#26778=CARTESIAN_POINT('Ctrl Pts',(-37.1201182410057,36.0116849136598,37.3042089236448));
#26779=CARTESIAN_POINT('Ctrl Pts',(-37.196719876171,36.0016561838974,37.3936253505669));
#26780=CARTESIAN_POINT('Ctrl Pts',(-37.2734658472122,35.9957993857637,37.4833841476179));
#26781=CARTESIAN_POINT('Ctrl Pts',(-37.3501637012311,35.9941290232867,37.5732602239549));
#26782=CARTESIAN_POINT('Ctrl Pts',(-37.42686155525,35.9924586608097,37.663136300292));
#26783=CARTESIAN_POINT('Ctrl Pts',(-37.5035112279651,35.9949747352775,37.7531295805852));
#26784=CARTESIAN_POINT('Ctrl Pts',(-37.579920515403,36.0016707719076,37.8430143955194));
#26785=CARTESIAN_POINT('Ctrl Pts',(-37.6563298028409,36.0083668085377,37.9328992104537));
#26786=CARTESIAN_POINT('Ctrl Pts',(-37.7324986409661,36.0192428016173,38.0226754846973));
#26787=CARTESIAN_POINT('Ctrl Pts',(-37.8082360374155,36.0342713307486,38.1121181007901));
#26788=CARTESIAN_POINT('Ctrl Pts',(-37.8839734338648,36.0492998598799,38.2015607168829));
#26789=CARTESIAN_POINT('Ctrl Pts',(-37.9592793251693,36.0684809123782,38.2906695998681));
#26790=CARTESIAN_POINT('Ctrl Pts',(-38.0339648871654,36.091766260255,38.3792213116681));
#26791=CARTESIAN_POINT('Ctrl Pts',(-38.1086504491616,36.1150516081317,38.4677730234682));
#26792=CARTESIAN_POINT('Ctrl Pts',(-38.1827156192643,36.1424412317938,38.555767489876));
#26793=CARTESIAN_POINT('Ctrl Pts',(-38.2559746872202,36.1738663378219,38.6429840712856));
#26794=CARTESIAN_POINT('Ctrl Pts',(-38.3292337551761,36.20529144385,38.7302006526952));
#26795=CARTESIAN_POINT('Ctrl Pts',(-38.4016866595967,36.2407520058409,38.8166392760205));
#26796=CARTESIAN_POINT('Ctrl Pts',(-38.4731517342401,36.2801590100262,38.9020832051809));
#26797=CARTESIAN_POINT('Ctrl Pts',(-38.5446168088833,36.3195660142115,38.9875271343413));
#26798=CARTESIAN_POINT('Ctrl Pts',(-38.6150939938646,36.3629194275101,39.0719762977373));
#26799=CARTESIAN_POINT('Ctrl Pts',(-38.6844065767933,36.4101104620801,39.1552189483062));
#26800=CARTESIAN_POINT('Ctrl Pts',(-38.753719159722,36.45730149665,39.2384615988751));
#26801=CARTESIAN_POINT('Ctrl Pts',(-38.8218670825167,36.5083301128978,39.3204976668618));
#26802=CARTESIAN_POINT('Ctrl Pts',(-38.8886794716687,36.5630682941429,39.4011214547246));
#26803=CARTESIAN_POINT('Ctrl Pts',(-38.9554918608208,36.617806475388,39.4817452425874));
#26804=CARTESIAN_POINT('Ctrl Pts',(-39.0209686603426,36.6762541757227,39.5609566827645));
#26805=CARTESIAN_POINT('Ctrl Pts',(-39.0849456914012,36.7382647910941,39.6385571574444));
#26806=CARTESIAN_POINT('Ctrl Pts',(-39.1489227224598,36.8002754064656,39.7161576321244));
#26807=CARTESIAN_POINT('Ctrl Pts',(-39.2113999314413,36.8658488848813,39.7921470762765));
#26808=CARTESIAN_POINT('Ctrl Pts',(-39.2722206564667,36.9348207694045,39.8663349465842));
#26809=CARTESIAN_POINT('Ctrl Pts',(-39.333041381492,37.0037926539277,39.9405228168919));
#26810=CARTESIAN_POINT('Ctrl Pts',(-39.3922055715889,37.0761628867415,40.0129090511807));
#26811=CARTESIAN_POINT('Ctrl Pts',(-39.4495648664821,37.1517499818605,40.0833121349731));
#26812=CARTESIAN_POINT('Ctrl Pts',(-35.8535977491494,36.5168641145602,36.0072213658969));
#26813=CARTESIAN_POINT('Ctrl Pts',(-35.9247900751538,36.4629824222449,36.088486901381));
#26814=CARTESIAN_POINT('Ctrl Pts',(-35.9971669834831,36.4130120864817,36.1713048624591));
#26815=CARTESIAN_POINT('Ctrl Pts',(-36.0705389847832,36.3670836000417,36.2554584119513));
#26816=CARTESIAN_POINT('Ctrl Pts',(-36.1438458351524,36.3211958959654,36.3395372369984));
#26817=CARTESIAN_POINT('Ctrl Pts',(-36.2181459453587,36.2793429079946,36.4249492030928));
#26818=CARTESIAN_POINT('Ctrl Pts',(-36.293245158042,36.2416337108208,36.5114711057138));
#26819=CARTESIAN_POINT('Ctrl Pts',(-36.3683443707253,36.2039245136471,36.5979930083348));
#26820=CARTESIAN_POINT('Ctrl Pts',(-36.4442426175417,36.170359141384,36.6856247687362));
#26821=CARTESIAN_POINT('Ctrl Pts',(-36.5207415821637,36.1410250303205,36.774137402972));
#26822=CARTESIAN_POINT('Ctrl Pts',(-36.5972405467856,36.111690919257,36.8626500372078));
#26823=CARTESIAN_POINT('Ctrl Pts',(-36.6743401596069,36.0865880958987,36.9520434647347));
#26824=CARTESIAN_POINT('Ctrl Pts',(-36.7518389803048,36.0657819033363,37.0420841172522));
#26825=CARTESIAN_POINT('Ctrl Pts',(-36.8293378010027,36.0449757107739,37.1321247697696));
#26826=CARTESIAN_POINT('Ctrl Pts',(-36.9072357590715,36.0284661677672,37.2228125653567));
#26827=CARTESIAN_POINT('Ctrl Pts',(-36.9853293413838,36.0162961846062,37.3139105702477));
#26828=CARTESIAN_POINT('Ctrl Pts',(-37.0634229236962,36.0041262014452,37.4050085751388));
#26829=CARTESIAN_POINT('Ctrl Pts',(-37.1417120592141,35.9962957890467,37.496516706462));
#26830=CARTESIAN_POINT('Ctrl Pts',(-37.2199922239388,35.9928252022519,37.5881959013455));
#26831=CARTESIAN_POINT('Ctrl Pts',(-37.2982723886635,35.989354615457,37.6798750962289));
#26832=CARTESIAN_POINT('Ctrl Pts',(-37.3765435113947,35.9902438572833,37.7717252712815));
#26833=CARTESIAN_POINT('Ctrl Pts',(-37.4546011244074,35.9954904225816,37.8635064819135));
#26834=CARTESIAN_POINT('Ctrl Pts',(-37.5326587374201,36.0007369878799,37.9552876925455));
#26835=CARTESIAN_POINT('Ctrl Pts',(-37.6105027697224,36.0103408717529,38.0469998552811));
#26836=CARTESIAN_POINT('Ctrl Pts',(-37.6879298766621,36.0242768231652,38.1384033957348));
#26837=CARTESIAN_POINT('Ctrl Pts',(-37.7653569836018,36.0382127745774,38.2298069361886));
#26838=CARTESIAN_POINT('Ctrl Pts',(-37.8423670947653,36.0564807807428,38.3209017712344));
#26839=CARTESIAN_POINT('Ctrl Pts',(-37.9187590494708,36.0790329774082,38.4114499466273));
#26840=CARTESIAN_POINT('Ctrl Pts',(-37.9951510041764,36.1015851740735,38.5019981220201));
#26841=CARTESIAN_POINT('Ctrl Pts',(-38.0709247329551,36.1284215406308,38.5919995554163));
#26842=CARTESIAN_POINT('Ctrl Pts',(-38.1458823085678,36.1594718501479,38.6812191541513));
#26843=CARTESIAN_POINT('Ctrl Pts',(-38.2208398841804,36.1905221596649,38.7704387528863));
#26844=CARTESIAN_POINT('Ctrl Pts',(-38.2949812384645,36.2257863838195,38.8588764358279));
#26845=CARTESIAN_POINT('Ctrl Pts',(-38.3681127102037,36.2651723000987,38.9463011983719));
#26846=CARTESIAN_POINT('Ctrl Pts',(-38.4412441819429,36.3045582163779,39.033725960916));
#26847=CARTESIAN_POINT('Ctrl Pts',(-38.5133657046363,36.348065788893,39.1201377235641));
#26848=CARTESIAN_POINT('Ctrl Pts',(-38.5842888934035,36.3955812812933,39.2053107749063));
#26849=CARTESIAN_POINT('Ctrl Pts',(-38.6552120821707,36.4430967736936,39.2904838262485));
#26850=CARTESIAN_POINT('Ctrl Pts',(-38.7249368725185,36.4946201427111,39.3744180888342));
#26851=CARTESIAN_POINT('Ctrl Pts',(-38.7932811386868,36.5500167320324,39.4568943219588));
#26852=CARTESIAN_POINT('Ctrl Pts',(-38.8616254048551,36.6054133213537,39.5393705550833));
#26853=CARTESIAN_POINT('Ctrl Pts',(-38.9285890846943,36.6646830805569,39.6203886837473));
#26854=CARTESIAN_POINT('Ctrl Pts',(-38.9939972617029,36.7276711362782,39.6997370817098));
#26855=CARTESIAN_POINT('Ctrl Pts',(-39.0594054387115,36.7906591919996,39.7790854796723));
#26856=CARTESIAN_POINT('Ctrl Pts',(-39.1232580534071,36.857365486926,39.8567640747754));
#26857=CARTESIAN_POINT('Ctrl Pts',(-39.1853883110917,36.92761573893,39.932569959291));
#26858=CARTESIAN_POINT('Ctrl Pts',(-39.2475185687763,36.9978659909341,40.0083758438067));
#26859=CARTESIAN_POINT('Ctrl Pts',(-39.3079264129444,37.0716601361098,40.0823089487944));
#26860=CARTESIAN_POINT('Ctrl Pts',(-39.3664540409007,37.1488053930167,40.1541761436298));
#26861=CARTESIAN_POINT('Ctrl Pts',(-35.7040417827465,36.5677479921179,36.0008564624337));
#26862=CARTESIAN_POINT('Ctrl Pts',(-35.7758191971864,36.5102371490812,36.0826718939149));
#26863=CARTESIAN_POINT('Ctrl Pts',(-35.8488922038129,36.4567456200151,36.1661759105181));
#26864=CARTESIAN_POINT('Ctrl Pts',(-35.9230616496862,36.4074191785411,36.2511409301588));
#26865=CARTESIAN_POINT('Ctrl Pts',(-35.9971652365349,36.3581365366571,36.3360305048066));
#26866=CARTESIAN_POINT('Ctrl Pts',(-36.0723632430923,36.3130116375408,36.422378405151));
#26867=CARTESIAN_POINT('Ctrl Pts',(-36.1484510914768,36.2721672445033,36.5099497197717));
#26868=CARTESIAN_POINT('Ctrl Pts',(-36.2245389398613,36.2313228514658,36.5975210343924));
#26869=CARTESIAN_POINT('Ctrl Pts',(-36.3015165548838,36.1947590048691,36.6863156767524));
#26870=CARTESIAN_POINT('Ctrl Pts',(-36.3791745171975,36.1625751774866,36.7760920790142));
#26871=CARTESIAN_POINT('Ctrl Pts',(-36.4568324795112,36.1303913501041,36.8658684812761));
#26872=CARTESIAN_POINT('Ctrl Pts',(-36.5351707123754,36.1025875737396,36.9566265547237));
#26873=CARTESIAN_POINT('Ctrl Pts',(-36.6139760948518,36.0792394891969,37.0481193899609));
#26874=CARTESIAN_POINT('Ctrl Pts',(-36.6927814773281,36.0558914046543,37.139612225198));
#26875=CARTESIAN_POINT('Ctrl Pts',(-36.7720539315419,36.0369990350059,37.2318397318125));
#26876=CARTESIAN_POINT('Ctrl Pts',(-36.8515777949845,36.0226137773715,37.3245510027818));
#26877=CARTESIAN_POINT('Ctrl Pts',(-36.9311016584271,36.0082285197373,37.4172622737511));
#26878=CARTESIAN_POINT('Ctrl Pts',(-37.0108768525138,35.9983503883324,37.510457217459));
#26879=CARTESIAN_POINT('Ctrl Pts',(-37.0906863470207,35.9930062568374,37.6038822949484));
#26880=CARTESIAN_POINT('Ctrl Pts',(-37.1704958415277,35.9876621253424,37.6973073724378));
#26881=CARTESIAN_POINT('Ctrl Pts',(-37.2503395575878,35.9868519990383,37.7909624913871));
#26882=CARTESIAN_POINT('Ctrl Pts',(-37.3300002785618,35.9905780818921,37.8845928609221));
#26883=CARTESIAN_POINT('Ctrl Pts',(-37.4096609995357,35.9943041647459,37.978223230457));
#26884=CARTESIAN_POINT('Ctrl Pts',(-37.4891386467036,36.0025664530755,38.0718287580532));
#26885=CARTESIAN_POINT('Ctrl Pts',(-37.5682169993246,36.0153424691381,38.1651547877508));
#26886=CARTESIAN_POINT('Ctrl Pts',(-37.6472953519455,36.0281184852008,38.2584808174484));
#26887=CARTESIAN_POINT('Ctrl Pts',(-37.7259743318751,36.0454082163714,38.3515272570235));
#26888=CARTESIAN_POINT('Ctrl Pts',(-37.804039891165,36.0671646255444,38.4440409715282));
#26889=CARTESIAN_POINT('Ctrl Pts',(-37.8821054504548,36.0889210347174,38.5365546860328));
#26890=CARTESIAN_POINT('Ctrl Pts',(-37.9595575119613,36.1151441003934,38.6285355840458));
#26891=CARTESIAN_POINT('Ctrl Pts',(-38.0361853655954,36.1457624821276,38.7197334294491));
#26892=CARTESIAN_POINT('Ctrl Pts',(-38.1128132192295,36.1763808638618,38.8109312748524));
#26893=CARTESIAN_POINT('Ctrl Pts',(-38.1886167892683,36.2113945313976,38.9013459775251));
#26894=CARTESIAN_POINT('Ctrl Pts',(-38.2633898503812,36.2507082292586,38.9907315622191));
#26895=CARTESIAN_POINT('Ctrl Pts',(-38.338162911494,36.2900219271197,39.0801171469131));
#26896=CARTESIAN_POINT('Ctrl Pts',(-38.411905389791,36.3336356164567,39.1684735252984));
#26897=CARTESIAN_POINT('Ctrl Pts',(-38.4844166671882,36.381430645239,39.2555603218448));
#26898=CARTESIAN_POINT('Ctrl Pts',(-38.5569279445854,36.4292256740213,39.3426471183912));
#26899=CARTESIAN_POINT('Ctrl Pts',(-38.6282079494279,36.4812019950186,39.4284642470403));
#26900=CARTESIAN_POINT('Ctrl Pts',(-38.6980627628468,36.537218205471,39.5127782403483));
#26901=CARTESIAN_POINT('Ctrl Pts',(-38.7679175762657,36.5932344159235,39.5970922336563));
#26902=CARTESIAN_POINT('Ctrl Pts',(-38.8363471292311,36.6532904604767,39.679903008305));
#26903=CARTESIAN_POINT('Ctrl Pts',(-38.903165257593,36.7172229552999,39.7609852757047));
#26904=CARTESIAN_POINT('Ctrl Pts',(-38.9699833859549,36.7811554501232,39.8420675431044));
#26905=CARTESIAN_POINT('Ctrl Pts',(-39.0351900236842,36.8489643320392,39.9214212231304));
#26906=CARTESIAN_POINT('Ctrl Pts',(-39.098607774645,36.9204651254473,39.9988304322975));
#26907=CARTESIAN_POINT('Ctrl Pts',(-39.1620255256058,36.9919659188554,40.0762396414646));
#26908=CARTESIAN_POINT('Ctrl Pts',(-39.2236543271292,37.0671585530995,40.1517043032776));
#26909=CARTESIAN_POINT('Ctrl Pts',(-39.2833265166636,37.1458384649135,40.2250191144136));
#26910=CARTESIAN_POINT('Ctrl Pts',(-35.5544858163436,36.6186318696757,35.9944915589704));
#26911=CARTESIAN_POINT('Ctrl Pts',(-35.6268483192189,36.5574918759175,36.0768568864488));
#26912=CARTESIAN_POINT('Ctrl Pts',(-35.7006174241427,36.5004791535485,36.1610469585772));
#26913=CARTESIAN_POINT('Ctrl Pts',(-35.7755843145893,36.4477547570404,36.2468234483664));
#26914=CARTESIAN_POINT('Ctrl Pts',(-35.8504846379174,36.3950771773488,36.3325237726148));
#26915=CARTESIAN_POINT('Ctrl Pts',(-35.9265805408259,36.346680367087,36.4198076072092));
#26916=CARTESIAN_POINT('Ctrl Pts',(-36.0036570249117,36.3027007781857,36.5084283338296));
#26917=CARTESIAN_POINT('Ctrl Pts',(-36.0807335089974,36.2587211892845,36.59704906045));
#26918=CARTESIAN_POINT('Ctrl Pts',(-36.1587904922259,36.2191588683541,36.6870065847686));
#26919=CARTESIAN_POINT('Ctrl Pts',(-36.2376074522313,36.1841253246526,36.7780467550565));
#26920=CARTESIAN_POINT('Ctrl Pts',(-36.3164244122368,36.1490917809511,36.8690869253443));
#26921=CARTESIAN_POINT('Ctrl Pts',(-36.396001265144,36.1185870515805,36.9612096447127));
#26922=CARTESIAN_POINT('Ctrl Pts',(-36.4761132093987,36.0926970750576,37.0541546626696));
#26923=CARTESIAN_POINT('Ctrl Pts',(-36.5562251536535,36.0668070985348,37.1470996806264));
#26924=CARTESIAN_POINT('Ctrl Pts',(-36.6368721040124,36.0455319022446,37.2408668982683));
#26925=CARTESIAN_POINT('Ctrl Pts',(-36.7178262485852,36.028931370137,37.3351914353158));
#26926=CARTESIAN_POINT('Ctrl Pts',(-36.798780393158,36.0123308380293,37.4295159723634));
#26927=CARTESIAN_POINT('Ctrl Pts',(-36.8800416458136,36.0004049876181,37.5243977284558));
#26928=CARTESIAN_POINT('Ctrl Pts',(-36.9613804701027,35.9931873114229,37.6195686885513));
#26929=CARTESIAN_POINT('Ctrl Pts',(-37.0427192943918,35.9859696352278,37.7147396486466));
#26930=CARTESIAN_POINT('Ctrl Pts',(-37.124135603781,35.9834601407934,37.8101997114927));
#26931=CARTESIAN_POINT('Ctrl Pts',(-37.2053994327162,35.9856657412027,37.9056792399306));
#26932=CARTESIAN_POINT('Ctrl Pts',(-37.2866632616515,35.9878713416119,38.0011587683686));
#26933=CARTESIAN_POINT('Ctrl Pts',(-37.3677745236849,35.994792034398,38.0966576608254));
#26934=CARTESIAN_POINT('Ctrl Pts',(-37.448504121987,36.0064081151111,38.1919061797668));
#26935=CARTESIAN_POINT('Ctrl Pts',(-37.5292337202892,36.0180241958241,38.2871546987081));
#26936=CARTESIAN_POINT('Ctrl Pts',(-37.609581568985,36.0343356519999,38.3821527428127));
#26937=CARTESIAN_POINT('Ctrl Pts',(-37.6893207328591,36.0552962736806,38.4766319964291));
#26938=CARTESIAN_POINT('Ctrl Pts',(-37.7690598967332,36.0762568953614,38.5711112500455));
#26939=CARTESIAN_POINT('Ctrl Pts',(-37.8481902909676,36.1018666601559,38.6650716126754));
#26940=CARTESIAN_POINT('Ctrl Pts',(-37.9264884226231,36.1320531141073,38.7582477047469));
#26941=CARTESIAN_POINT('Ctrl Pts',(-38.0047865542786,36.1622395680588,38.8514237968184));
#26942=CARTESIAN_POINT('Ctrl Pts',(-38.0822523400722,36.1970026789757,38.9438155192224));
#26943=CARTESIAN_POINT('Ctrl Pts',(-38.1586669905587,36.2362441584186,39.0351619260663));
#26944=CARTESIAN_POINT('Ctrl Pts',(-38.2350816410452,36.2754856378615,39.1265083329102));
#26945=CARTESIAN_POINT('Ctrl Pts',(-38.3104450749457,36.3192054440204,39.2168093270328));
#26946=CARTESIAN_POINT('Ctrl Pts',(-38.384544440973,36.3672800091847,39.3058098687833));
#26947=CARTESIAN_POINT('Ctrl Pts',(-38.4586438070002,36.415354574349,39.3948104105338));
#26948=CARTESIAN_POINT('Ctrl Pts',(-38.5314790263374,36.467783847326,39.4825104052464));
#26949=CARTESIAN_POINT('Ctrl Pts',(-38.6028443870069,36.5244196789096,39.5686621587378));
#26950=CARTESIAN_POINT('Ctrl Pts',(-38.6742097476763,36.5810555104933,39.6548139122292));
#26951=CARTESIAN_POINT('Ctrl Pts',(-38.744105173768,36.6418978403966,39.7394173328626));
#26952=CARTESIAN_POINT('Ctrl Pts',(-38.8123332534831,36.7067747743217,39.8222334696996));
#26953=CARTESIAN_POINT('Ctrl Pts',(-38.8805613331982,36.7716517082468,39.9050496065365));
#26954=CARTESIAN_POINT('Ctrl Pts',(-38.9471219939613,36.8405631771523,39.9860783714854));
#26955=CARTESIAN_POINT('Ctrl Pts',(-39.0118272381983,36.9133145119646,40.065090905304));
#26956=CARTESIAN_POINT('Ctrl Pts',(-39.0765324824353,36.9860658467768,40.1441034391225));
#26957=CARTESIAN_POINT('Ctrl Pts',(-39.139382241314,37.0626569700893,40.2210996577609));
#26958=CARTESIAN_POINT('Ctrl Pts',(-39.2001989924265,37.1428715368103,40.2958620851973));
#26959=CARTESIAN_POINT('Ctrl Pts',(-35.4072750999858,36.6721941387054,35.9905697714741));
#26960=CARTESIAN_POINT('Ctrl Pts',(-35.4801082384467,36.607379442505,36.0733509486624));
#26961=CARTESIAN_POINT('Ctrl Pts',(-35.5544646259996,36.5467939873462,36.1580999369808));
#26962=CARTESIAN_POINT('Ctrl Pts',(-35.6301257489358,36.4906154512438,36.2445676684546));
#26963=CARTESIAN_POINT('Ctrl Pts',(-35.7057196883076,36.4344867990733,36.3309586205972));
#26964=CARTESIAN_POINT('Ctrl Pts',(-35.7826159602713,36.3827573072814,36.4190651657937));
#26965=CARTESIAN_POINT('Ctrl Pts',(-35.8605890143666,36.335578390006,36.5086288612754));
#26966=CARTESIAN_POINT('Ctrl Pts',(-35.9385620684619,36.2883994727305,36.5981925567571));
#26967=CARTESIAN_POINT('Ctrl Pts',(-36.0176118152452,36.2457711838453,36.6892132997768));
#26968=CARTESIAN_POINT('Ctrl Pts',(-36.0975064077398,36.2078182611662,36.7814241245148));
#26969=CARTESIAN_POINT('Ctrl Pts',(-36.1774010002343,36.1698653384872,36.8736349492527));
#26970=CARTESIAN_POINT('Ctrl Pts',(-36.2581403468076,36.1365878253204,36.9670357499442));
#26971=CARTESIAN_POINT('Ctrl Pts',(-36.3394876625489,36.1080830540372,37.0613526021471));
#26972=CARTESIAN_POINT('Ctrl Pts',(-36.4208349782902,36.0795782827539,37.1556694543499));
#26973=CARTESIAN_POINT('Ctrl Pts',(-36.502790169914,36.0558462858404,37.2509022499006));
#26974=CARTESIAN_POINT('Ctrl Pts',(-36.5851129019827,36.0369564215669,37.3467717108003));
#26975=CARTESIAN_POINT('Ctrl Pts',(-36.6674356340514,36.0180665572934,37.4426411717001));
#26976=CARTESIAN_POINT('Ctrl Pts',(-36.7501258121725,36.0040188471366,37.5391471880195));
#26977=CARTESIAN_POINT('Ctrl Pts',(-36.8329409584958,35.9948542703932,37.6360067645168));
#26978=CARTESIAN_POINT('Ctrl Pts',(-36.9157561048191,35.9856896936499,37.732866341014));
#26979=CARTESIAN_POINT('Ctrl Pts',(-36.9986961243973,35.9814082606621,37.8300793666369));
#26980=CARTESIAN_POINT('Ctrl Pts',(-37.0815178175531,35.9820223330219,37.9273607868886));
#26981=CARTESIAN_POINT('Ctrl Pts',(-37.1643395107089,35.9826364053818,38.0246422071404));
#26982=CARTESIAN_POINT('Ctrl Pts',(-37.2470427824952,35.9881459822369,38.1219919104955));
#26983=CARTESIAN_POINT('Ctrl Pts',(-37.3293851361536,35.9985347362742,38.219124453167));
#26984=CARTESIAN_POINT('Ctrl Pts',(-37.411727489812,36.0089234903114,38.3162569958385));
#26985=CARTESIAN_POINT('Ctrl Pts',(-37.4937088309511,36.0241914094893,38.4131722664797));
#26986=CARTESIAN_POINT('Ctrl Pts',(-37.5750887863036,36.0442935743273,38.5095861041859));
#26987=CARTESIAN_POINT('Ctrl Pts',(-37.6564687416562,36.0643957391652,38.6059999418921));
#26988=CARTESIAN_POINT('Ctrl Pts',(-37.7372472179389,36.0893321265037,38.7019122361468));
#26989=CARTESIAN_POINT('Ctrl Pts',(-37.8171873734666,36.1190294887985,38.7970417735272));
#26990=CARTESIAN_POINT('Ctrl Pts',(-37.8971275289942,36.1487268510933,38.8921713109075));
#26991=CARTESIAN_POINT('Ctrl Pts',(-37.9762292721368,36.1831851542028,38.9865179823737));
#26992=CARTESIAN_POINT('Ctrl Pts',(-38.0542606801644,36.2223032524384,39.079805169276));
#26993=CARTESIAN_POINT('Ctrl Pts',(-38.1322920881921,36.261421350674,39.1730923561784));
#26994=CARTESIAN_POINT('Ctrl Pts',(-38.2092530716641,36.3051991991118,39.2653199515914));
#26995=CARTESIAN_POINT('Ctrl Pts',(-38.2849179853468,36.3535083471339,39.3562175519869));
#26996=CARTESIAN_POINT('Ctrl Pts',(-38.3605828990296,36.4018174951558,39.4471151523824));
#26997=CARTESIAN_POINT('Ctrl Pts',(-38.4349516561949,36.4546578873189,39.5366826535746));
#26998=CARTESIAN_POINT('Ctrl Pts',(-38.5078062108692,36.5118745211112,39.6246574510852));
#26999=CARTESIAN_POINT('Ctrl Pts',(-38.5806607655435,36.5690911549036,39.7126322485958));
#27000=CARTESIAN_POINT('Ctrl Pts',(-38.6520010342182,36.6306839646873,39.7990142415882));
#27001=CARTESIAN_POINT('Ctrl Pts',(-38.7216178474355,36.6964723045064,39.8835501628792));
#27002=CARTESIAN_POINT('Ctrl Pts',(-38.7912346606527,36.7622606443254,39.9680860841702));
#27003=CARTESIAN_POINT('Ctrl Pts',(-38.8591279386121,36.8322444387312,40.0507758368621));
#27004=CARTESIAN_POINT('Ctrl Pts',(-38.9250986136492,36.9062184568694,40.1313769746322));
#27005=CARTESIAN_POINT('Ctrl Pts',(-38.9910692886862,36.9801924750076,40.2119781124024));
#27006=CARTESIAN_POINT('Ctrl Pts',(-39.0551172851754,37.0581566320604,40.2904905428586));
#27007=CARTESIAN_POINT('Ctrl Pts',(-39.1170548033789,37.1398823147253,40.366684060748));
#27008=CARTESIAN_POINT('Ctrl Pts',(-35.2622498364415,36.7281963563022,35.9888869492133));
#27009=CARTESIAN_POINT('Ctrl Pts',(-35.3354429836358,36.65967121659,36.0719528236328));
#27010=CARTESIAN_POINT('Ctrl Pts',(-35.410281415356,36.5954705570286,36.1571363122166));
#27011=CARTESIAN_POINT('Ctrl Pts',(-35.4865369655357,36.5357900959079,36.2441777084119));
#27012=CARTESIAN_POINT('Ctrl Pts',(-35.5627248043271,36.476162628266,36.3311418158883));
#27013=CARTESIAN_POINT('Ctrl Pts',(-35.6403271517951,36.4210474089236,36.419960425412));
#27014=CARTESIAN_POINT('Ctrl Pts',(-35.7191078392476,36.3706121710703,36.5103632336284));
#27015=CARTESIAN_POINT('Ctrl Pts',(-35.7978885267002,36.320176933217,36.6007660418448));
#27016=CARTESIAN_POINT('Ctrl Pts',(-35.8778474567011,36.2744217392313,36.6927529369434));
#27017=CARTESIAN_POINT('Ctrl Pts',(-35.9587412887259,36.2334858367607,36.7860439734662));
#27018=CARTESIAN_POINT('Ctrl Pts',(-36.0396351207508,36.1925499342901,36.879335009989));
#27019=CARTESIAN_POINT('Ctrl Pts',(-36.1214637547498,36.1564333739643,36.9739300725531));
#27020=CARTESIAN_POINT('Ctrl Pts',(-36.2039781600931,36.1252460699945,37.0695412782153));
#27021=CARTESIAN_POINT('Ctrl Pts',(-36.2864925654364,36.0940587660247,37.1651524838775));
#27022=CARTESIAN_POINT('Ctrl Pts',(-36.3696926400698,36.0678007569836,37.2617797143853));
#27023=CARTESIAN_POINT('Ctrl Pts',(-36.4533251796323,36.0465519543668,37.3591289022602));
#27024=CARTESIAN_POINT('Ctrl Pts',(-36.5369577191948,36.0253031517499,37.4564780901352));
#27025=CARTESIAN_POINT('Ctrl Pts',(-36.6210226202494,36.0090635818379,37.5545491149753));
#27026=CARTESIAN_POINT('Ctrl Pts',(-36.7052640464922,35.9978826668211,37.6530435153755));
#27027=CARTESIAN_POINT('Ctrl Pts',(-36.789505472735,35.9867017518044,37.7515379157757));
#27028=CARTESIAN_POINT('Ctrl Pts',(-36.873923319976,35.9805795055114,37.8504555699178));
#27029=CARTESIAN_POINT('Ctrl Pts',(-36.9582606777837,35.9795345598903,37.9494954398334));
#27030=CARTESIAN_POINT('Ctrl Pts',(-37.0425980355914,35.9784896142691,38.0485353097491));
#27031=CARTESIAN_POINT('Ctrl Pts',(-37.1268547996569,35.9825219706122,38.1476972729454));
#27032=CARTESIAN_POINT('Ctrl Pts',(-37.2107745497763,35.9916193571731,38.2466795479439));
#27033=CARTESIAN_POINT('Ctrl Pts',(-37.2946942998957,36.0007167437339,38.3456618229425));
#27034=CARTESIAN_POINT('Ctrl Pts',(-37.3782769322767,36.0148791492609,38.4444642873216));
#27035=CARTESIAN_POINT('Ctrl Pts',(-37.461268078313,36.0340634730374,38.5427862536723));
#27036=CARTESIAN_POINT('Ctrl Pts',(-37.5442592243492,36.0532477968139,38.641108220023));
#27037=CARTESIAN_POINT('Ctrl Pts',(-37.6266587813969,36.0774540151126,38.7389495667403));
#27038=CARTESIAN_POINT('Ctrl Pts',(-37.7082159813253,36.1066084606916,38.8360125314027));
#27039=CARTESIAN_POINT('Ctrl Pts',(-37.7897731812537,36.1357629062705,38.9330754960651));
#27040=CARTESIAN_POINT('Ctrl Pts',(-37.8704879231926,36.1698655430712,39.0293599586248));
#27041=CARTESIAN_POINT('Ctrl Pts',(-37.9501145664407,36.2088125858941,39.1245728947555));
#27042=CARTESIAN_POINT('Ctrl Pts',(-38.029741209689,36.2477596287169,39.2197858308861));
#27043=CARTESIAN_POINT('Ctrl Pts',(-38.1082796557639,36.291551029392,39.3139271228279));
#27044=CARTESIAN_POINT('Ctrl Pts',(-38.185490887127,36.3400535167211,39.4067102686062));
#27045=CARTESIAN_POINT('Ctrl Pts',(-38.2627021184901,36.3885560040504,39.4994934143845));
#27046=CARTESIAN_POINT('Ctrl Pts',(-38.338586039646,36.4417695180457,39.5909182992447));
#27047=CARTESIAN_POINT('Ctrl Pts',(-38.4129117116221,36.4995321130133,39.6807066881051));
#27048=CARTESIAN_POINT('Ctrl Pts',(-38.4872373835982,36.5572947079808,39.7704950769655));
#27049=CARTESIAN_POINT('Ctrl Pts',(-38.5600047144681,36.6196063124796,39.8586468587756));
#27050=CARTESIAN_POINT('Ctrl Pts',(-38.6309922500372,36.6862772924249,39.94489375955));
#27051=CARTESIAN_POINT('Ctrl Pts',(-38.7019797856063,36.7529482723702,40.0311406603245));
#27052=CARTESIAN_POINT('Ctrl Pts',(-38.771187438077,36.8239785453029,40.1154825733928));
#27053=CARTESIAN_POINT('Ctrl Pts',(-38.8384045864911,36.89915194345,40.1976628194154));
#27054=CARTESIAN_POINT('Ctrl Pts',(-38.9056217349053,36.974325341597,40.279843065438));
#27055=CARTESIAN_POINT('Ctrl Pts',(-38.9708482961285,37.0536417719834,40.3598615427741));
#27056=CARTESIAN_POINT('Ctrl Pts',(-39.0338857649331,37.1368598494162,40.4374747296777));
#27057=CARTESIAN_POINT('Ctrl Pts',(-35.1172245728972,36.7841985738989,35.9872041269524));
#27058=CARTESIAN_POINT('Ctrl Pts',(-35.1907777288249,36.711962990675,36.0705546986032));
#27059=CARTESIAN_POINT('Ctrl Pts',(-35.2660982047123,36.6441471267109,36.1561726874525));
#27060=CARTESIAN_POINT('Ctrl Pts',(-35.3429481821355,36.580964740572,36.2437877483692));
#27061=CARTESIAN_POINT('Ctrl Pts',(-35.4197299203466,36.5178384574586,36.3313250111794));
#27062=CARTESIAN_POINT('Ctrl Pts',(-35.4980383433188,36.4593375105657,36.4208556850302));
#27063=CARTESIAN_POINT('Ctrl Pts',(-35.5776266641287,36.4056459521345,36.5120976059814));
#27064=CARTESIAN_POINT('Ctrl Pts',(-35.6572149849385,36.3519543937034,36.6033395269325));
#27065=CARTESIAN_POINT('Ctrl Pts',(-35.7380830981569,36.3030722946172,36.6962925741101));
#27066=CARTESIAN_POINT('Ctrl Pts',(-35.8199761697121,36.2591534123552,36.7906638224176));
#27067=CARTESIAN_POINT('Ctrl Pts',(-35.9018692412672,36.2152345300931,36.8850350707252));
#27068=CARTESIAN_POINT('Ctrl Pts',(-35.9847871626919,36.1762789226082,36.980824395162));
#27069=CARTESIAN_POINT('Ctrl Pts',(-36.0684686576372,36.1424090859519,37.0777299542835));
#27070=CARTESIAN_POINT('Ctrl Pts',(-36.1521501525826,36.1085392492955,37.174635513405));
#27071=CARTESIAN_POINT('Ctrl Pts',(-36.2365951102256,36.0797552281268,37.27265717887));
#27072=CARTESIAN_POINT('Ctrl Pts',(-36.321537457282,36.0561474871666,37.3714860937201));
#27073=CARTESIAN_POINT('Ctrl Pts',(-36.4064798043383,36.0325397462063,37.4703150085703));
#27074=CARTESIAN_POINT('Ctrl Pts',(-36.4919194283263,36.0141083165392,37.5699510419312));
#27075=CARTESIAN_POINT('Ctrl Pts',(-36.5775871344886,36.0009110632491,37.6700802662343));
#27076=CARTESIAN_POINT('Ctrl Pts',(-36.6632548406509,35.9877138099589,37.7702094905375));
#27077=CARTESIAN_POINT('Ctrl Pts',(-36.7491505155547,35.9797507503608,37.8708317731987));
#27078=CARTESIAN_POINT('Ctrl Pts',(-36.8350035380143,35.9770467867587,37.9716300927782));
#27079=CARTESIAN_POINT('Ctrl Pts',(-36.9208565604738,35.9743428231565,38.0724284123577));
#27080=CARTESIAN_POINT('Ctrl Pts',(-37.0066668168186,35.9768979589874,38.1734026353953));
#27081=CARTESIAN_POINT('Ctrl Pts',(-37.092163963399,35.9847039780719,38.274234642721));
#27082=CARTESIAN_POINT('Ctrl Pts',(-37.1776611099795,35.9925099971564,38.3750666500466));
#27083=CARTESIAN_POINT('Ctrl Pts',(-37.2628450336024,36.0055668890324,38.4757563081636));
#27084=CARTESIAN_POINT('Ctrl Pts',(-37.3474473703222,36.0238333717476,38.5759864031588));
#27085=CARTESIAN_POINT('Ctrl Pts',(-37.4320497070421,36.0420998544626,38.6762164981539));
#27086=CARTESIAN_POINT('Ctrl Pts',(-37.5160703448549,36.0655759037215,38.7759868973337));
#27087=CARTESIAN_POINT('Ctrl Pts',(-37.5992445891841,36.0941874325846,38.8749832892782));
#27088=CARTESIAN_POINT('Ctrl Pts',(-37.6824188335133,36.1227989614476,38.9739796812228));
#27089=CARTESIAN_POINT('Ctrl Pts',(-37.7647465742484,36.1565459319396,39.072201934876));
#27090=CARTESIAN_POINT('Ctrl Pts',(-37.8459684527171,36.1953219193496,39.169340620235));
#27091=CARTESIAN_POINT('Ctrl Pts',(-37.9271903311858,36.2340979067598,39.2664793055939));
#27092=CARTESIAN_POINT('Ctrl Pts',(-38.0073062398638,36.2779028596721,39.3625342940644));
#27093=CARTESIAN_POINT('Ctrl Pts',(-38.0860637889071,36.3265986863085,39.4572029852256));
#27094=CARTESIAN_POINT('Ctrl Pts',(-38.1648213379505,36.375294512945,39.5518716763867));
#27095=CARTESIAN_POINT('Ctrl Pts',(-38.2422204230971,36.4288811487726,39.6451539449147));
#27096=CARTESIAN_POINT('Ctrl Pts',(-38.318017212375,36.4871897049153,39.736755925125));
#27097=CARTESIAN_POINT('Ctrl Pts',(-38.3938140016529,36.5454982610581,39.8283579053353));
#27098=CARTESIAN_POINT('Ctrl Pts',(-38.468008394718,36.6085286602719,39.9182794759629));
#27099=CARTESIAN_POINT('Ctrl Pts',(-38.540366652639,36.6760822803433,40.0062373562209));
#27100=CARTESIAN_POINT('Ctrl Pts',(-38.61272491056,36.7436359004149,40.0941952364787));
#27101=CARTESIAN_POINT('Ctrl Pts',(-38.6832469375418,36.8157126518747,40.1801893099235));
#27102=CARTESIAN_POINT('Ctrl Pts',(-38.7517105593331,36.8920854300305,40.2639486641986));
#27103=CARTESIAN_POINT('Ctrl Pts',(-38.8201741811244,36.9684582081863,40.3477080184737));
#27104=CARTESIAN_POINT('Ctrl Pts',(-38.8865793070816,37.0491269119063,40.4292325426895));
#27105=CARTESIAN_POINT('Ctrl Pts',(-38.9507167264873,37.133837384107,40.5082653986073));
#27106=CARTESIAN_POINT('Ctrl Pts',(-34.9743855755961,36.8426418770279,35.9877612574109));
#27107=CARTESIAN_POINT('Ctrl Pts',(-35.0481880902205,36.7666600782349,36.0712653535917));
#27108=CARTESIAN_POINT('Ctrl Pts',(-35.123885349332,36.6951865080667,36.1571934070156));
#27109=CARTESIAN_POINT('Ctrl Pts',(-35.2012299269113,36.6284543820813,36.2452645362456));
#27110=CARTESIAN_POINT('Ctrl Pts',(-35.2785058260965,36.5617815111257,36.3332574624016));
#27111=CARTESIAN_POINT('Ctrl Pts',(-35.35742600984,36.4998417620662,36.4233895351976));
#27112=CARTESIAN_POINT('Ctrl Pts',(-35.4377330067502,36.4428368630046,36.5153666938478));
#27113=CARTESIAN_POINT('Ctrl Pts',(-35.5180400036605,36.3858319639429,36.6073438524981));
#27114=CARTESIAN_POINT('Ctrl Pts',(-35.5997336997324,36.3337619955086,36.7011659664208));
#27115=CARTESIAN_POINT('Ctrl Pts',(-35.6825475983504,36.2867965062328,36.7965269652247));
#27116=CARTESIAN_POINT('Ctrl Pts',(-35.7653614969684,36.239831016957,36.8918879640286));
#27117=CARTESIAN_POINT('Ctrl Pts',(-35.8492954805879,36.1979700732353,36.9887877123526));
#27118=CARTESIAN_POINT('Ctrl Pts',(-35.9340757647227,36.1613499408784,37.0869101256075));
#27119=CARTESIAN_POINT('Ctrl Pts',(-36.0188560488575,36.1247298085214,37.1850325388624));
#27120=CARTESIAN_POINT('Ctrl Pts',(-36.1044825131889,36.0933505392597,37.2843774777892));
#27121=CARTESIAN_POINT('Ctrl Pts',(-36.1906758700819,36.0673142298672,37.3846209041141));
#27122=CARTESIAN_POINT('Ctrl Pts',(-36.276869226975,36.0412779204747,37.4848643304389));
#27123=CARTESIAN_POINT('Ctrl Pts',(-36.3636293541202,36.0205846076808,37.5860061019117));
#27124=CARTESIAN_POINT('Ctrl Pts',(-36.4506732812072,36.0053015554969,37.6877163387799));
#27125=CARTESIAN_POINT('Ctrl Pts',(-36.5377172082942,35.9900185033129,37.7894265756482));
#27126=CARTESIAN_POINT('Ctrl Pts',(-36.6250448118189,35.9801457332289,37.8917051335964));
#27127=CARTESIAN_POINT('Ctrl Pts',(-36.7123712831683,35.9757152396661,37.9942184415413));
#27128=CARTESIAN_POINT('Ctrl Pts',(-36.7996977545177,35.9712847461032,38.0967317494861));
#27129=CARTESIAN_POINT('Ctrl Pts',(-36.8870229697971,35.9722965351728,38.199479661986));
#27130=CARTESIAN_POINT('Ctrl Pts',(-36.9740621383579,35.978747124609,38.3021270907198));
#27131=CARTESIAN_POINT('Ctrl Pts',(-37.0611013069187,35.9851977140451,38.4047745194536));
#27132=CARTESIAN_POINT('Ctrl Pts',(-37.147854305282,35.9970870945416,38.5073213188002));
#27133=CARTESIAN_POINT('Ctrl Pts',(-37.2340382168427,36.0143763311173,38.6094330670883));
#27134=CARTESIAN_POINT('Ctrl Pts',(-37.3202221284034,36.0316655676929,38.7115448153763));
#27135=CARTESIAN_POINT('Ctrl Pts',(-37.405836830902,36.054354635685,38.8132213677531));
#27136=CARTESIAN_POINT('Ctrl Pts',(-37.4906031255867,36.0823694022728,38.914131148664));
#27137=CARTESIAN_POINT('Ctrl Pts',(-37.5753694202713,36.1103841688607,39.0150409295749));
#27138=CARTESIAN_POINT('Ctrl Pts',(-37.6592871868977,36.1437245941859,39.1151837958783));
#27139=CARTESIAN_POINT('Ctrl Pts',(-37.7420827641078,36.1822818317011,39.2142331789989));
#27140=CARTESIAN_POINT('Ctrl Pts',(-37.8248783413179,36.2208390692164,39.3132825621194));
#27141=CARTESIAN_POINT('Ctrl Pts',(-37.906551611665,36.2646130641274,39.4112383215582));
#27142=CARTESIAN_POINT('Ctrl Pts',(-37.9868362346136,36.3134609663522,39.5077810239121));
#27143=CARTESIAN_POINT('Ctrl Pts',(-38.0671208575622,36.362308868577,39.604323726266));
#27144=CARTESIAN_POINT('Ctrl Pts',(-38.1460167192277,36.4162306087426,39.6994532345935));
#27145=CARTESIAN_POINT('Ctrl Pts',(-38.2232665356069,36.475050264875,39.7928593323378));
#27146=CARTESIAN_POINT('Ctrl Pts',(-38.300516351986,36.5338699210074,39.886265430082));
#27147=CARTESIAN_POINT('Ctrl Pts',(-38.3761200134976,36.5975874096069,39.9779479847499));
#27148=CARTESIAN_POINT('Ctrl Pts',(-38.4498309693652,36.6659948838339,40.0676080182377));
#27149=CARTESIAN_POINT('Ctrl Pts',(-38.5235419252329,36.7344023580609,40.1572680517256));
#27150=CARTESIAN_POINT('Ctrl Pts',(-38.5953600708919,36.8074997208323,40.2449054368509));
#27151=CARTESIAN_POINT('Ctrl Pts',(-38.6650511955598,36.8850485553831,40.3302343823459));
#27152=CARTESIAN_POINT('Ctrl Pts',(-38.7347423202279,36.9625973899338,40.415563327841));
#27153=CARTESIAN_POINT('Ctrl Pts',(-38.8023063250372,37.0445975862294,40.4985837126617));
#27154=CARTESIAN_POINT('Ctrl Pts',(-38.8675228655817,37.1307817116115,40.5790247948543));
#27155=CARTESIAN_POINT('Ctrl Pts',(-34.8336193643568,36.9033396115506,35.9904016908844));
#27156=CARTESIAN_POINT('Ctrl Pts',(-34.9075633574833,36.8235846665107,36.0739295021119));
#27157=CARTESIAN_POINT('Ctrl Pts',(-34.9835346561969,36.7484189640353,36.1600443950741));
#27158=CARTESIAN_POINT('Ctrl Pts',(-35.0612763540517,36.6780966665432,36.2484551606249));
#27159=CARTESIAN_POINT('Ctrl Pts',(-35.138949020888,36.6078368119867,36.3367874215202));
#27160=CARTESIAN_POINT('Ctrl Pts',(-35.2183888259916,36.542411871719,36.4274113451302));
#27161=CARTESIAN_POINT('Ctrl Pts',(-35.2993276161375,36.4820426910545,36.5200210256517));
#27162=CARTESIAN_POINT('Ctrl Pts',(-35.3802664062833,36.4216735103901,36.6126307061731));
#27163=CARTESIAN_POINT('Ctrl Pts',(-35.4627040582955,36.3663601812011,36.707226002669));
#27164=CARTESIAN_POINT('Ctrl Pts',(-35.5463622995597,36.3162894165289,36.8034876037588));
#27165=CARTESIAN_POINT('Ctrl Pts',(-35.630020540824,36.2662186518567,36.8997492048486));
#27166=CARTESIAN_POINT('Ctrl Pts',(-35.7148992440258,36.2213905279009,36.9976769640377));
#27167=CARTESIAN_POINT('Ctrl Pts',(-35.8007118966545,36.1819563643431,37.096940321043));
#27168=CARTESIAN_POINT('Ctrl Pts',(-35.8865245492833,36.1425222007853,37.1962036780483));
#27169=CARTESIAN_POINT('Ctrl Pts',(-35.9732710207459,36.108482057638,37.2968024818071));
#27170=CARTESIAN_POINT('Ctrl Pts',(-36.0606584937822,36.0799508391881,37.3983971557854));
#27171=CARTESIAN_POINT('Ctrl Pts',(-36.1480459668184,36.0514196207383,37.4999918297637));
#27172=CARTESIAN_POINT('Ctrl Pts',(-36.2360743084386,36.0283973704059,37.6025822193508));
#27173=CARTESIAN_POINT('Ctrl Pts',(-36.3244463743625,36.0109618010034,37.7058220253105));
#27174=CARTESIAN_POINT('Ctrl Pts',(-36.4128184402864,35.9935262316009,37.8090618312702));
#27175=CARTESIAN_POINT('Ctrl Pts',(-36.5015340960261,35.9816773696623,37.9129508964882));
#27176=CARTESIAN_POINT('Ctrl Pts',(-36.5902938772363,35.9754552116421,38.0171385379805));
#27177=CARTESIAN_POINT('Ctrl Pts',(-36.6790536584466,35.9692330536221,38.1213261794728));
#27178=CARTESIAN_POINT('Ctrl Pts',(-36.7678574300494,35.9686376089895,38.2258122386827));
#27179=CARTESIAN_POINT('Ctrl Pts',(-36.8564054302601,35.9736708876989,38.3302440174417));
#27180=CARTESIAN_POINT('Ctrl Pts',(-36.9449534304708,35.9787041664084,38.4346757962008));
#27181=CARTESIAN_POINT('Ctrl Pts',(-37.0332455245334,35.9893661608002,38.5390531355806));
#27182=CARTESIAN_POINT('Ctrl Pts',(-37.1209836778578,36.0056208807534,38.6430237044025));
#27183=CARTESIAN_POINT('Ctrl Pts',(-37.2087218311821,36.0218756007066,38.7469942732243));
#27184=CARTESIAN_POINT('Ctrl Pts',(-37.2959059102448,36.0437230214842,38.8505579132615));
#27185=CARTESIAN_POINT('Ctrl Pts',(-37.382241620618,36.0710893959725,38.9533650400202));
#27186=CARTESIAN_POINT('Ctrl Pts',(-37.4685773309913,36.0984557704607,39.0561721667788));
#27187=CARTESIAN_POINT('Ctrl Pts',(-37.5540645412861,36.1313410570124,39.1582226238029));
#27188=CARTESIAN_POINT('Ctrl Pts',(-37.6384146849442,36.1696342496195,39.2591719344269));
#27189=CARTESIAN_POINT('Ctrl Pts',(-37.7227648286024,36.2079274422265,39.3601212450509));
#27190=CARTESIAN_POINT('Ctrl Pts',(-37.8059777772566,36.2516284826128,39.4599692556463));
#27191=CARTESIAN_POINT('Ctrl Pts',(-37.8877726412378,36.3005898556264,39.5583789240207));
#27192=CARTESIAN_POINT('Ctrl Pts',(-37.969567505219,36.3495512286401,39.6567885923951));
#27193=CARTESIAN_POINT('Ctrl Pts',(-38.0499441600487,36.4037728597698,39.7537597687849));
#27194=CARTESIAN_POINT('Ctrl Pts',(-38.1286312901165,36.4630717210582,39.8489651219026));
#27195=CARTESIAN_POINT('Ctrl Pts',(-38.2073184201842,36.5223705823465,39.9441704750202));
#27196=CARTESIAN_POINT('Ctrl Pts',(-38.2843159057409,36.5867465835503,40.0376098599784));
#27197=CARTESIAN_POINT('Ctrl Pts',(-38.3593638377389,36.6559824201038,40.1289678672367));
#27198=CARTESIAN_POINT('Ctrl Pts',(-38.434411769737,36.7252182566573,40.2203258744951));
#27199=CARTESIAN_POINT('Ctrl Pts',(-38.5075100339655,36.7993138231947,40.3096023650212));
#27200=CARTESIAN_POINT('Ctrl Pts',(-38.5784118834031,36.8780190062483,40.3964959813431));
#27201=CARTESIAN_POINT('Ctrl Pts',(-38.6493137328406,36.9567241893019,40.4833895976649));
#27202=CARTESIAN_POINT('Ctrl Pts',(-38.718019059586,37.0400388690951,40.5679002075443));
#27203=CARTESIAN_POINT('Ctrl Pts',(-38.7842959452082,37.1276818125601,40.6497425409889));
#27204=CARTESIAN_POINT('Ctrl Pts',(-34.6928531531176,36.9640373460733,35.993042124358));
#27205=CARTESIAN_POINT('Ctrl Pts',(-34.7669386247461,36.8805092547864,36.0765936506321));
#27206=CARTESIAN_POINT('Ctrl Pts',(-34.8431839630618,36.8016514200038,36.1628953831327));
#27207=CARTESIAN_POINT('Ctrl Pts',(-34.9213227811921,36.7277389510052,36.2516457850041));
#27208=CARTESIAN_POINT('Ctrl Pts',(-34.9993922156795,36.6538921128476,36.3403173806389));
#27209=CARTESIAN_POINT('Ctrl Pts',(-35.0793516421433,36.5849819813717,36.4314331550628));
#27210=CARTESIAN_POINT('Ctrl Pts',(-35.1609222255247,36.5212485191045,36.5246753574555));
#27211=CARTESIAN_POINT('Ctrl Pts',(-35.242492808906,36.4575150568373,36.6179175598482));
#27212=CARTESIAN_POINT('Ctrl Pts',(-35.3256744168587,36.3989583668936,36.7132860389173));
#27213=CARTESIAN_POINT('Ctrl Pts',(-35.4101770007691,36.345782326825,36.810448242293));
#27214=CARTESIAN_POINT('Ctrl Pts',(-35.4946795846796,36.2926062867564,36.9076104456687));
#27215=CARTESIAN_POINT('Ctrl Pts',(-35.5805030074637,36.2448109825665,37.0065662157227));
#27216=CARTESIAN_POINT('Ctrl Pts',(-35.6673480285863,36.2025627878079,37.1069705164784));
#27217=CARTESIAN_POINT('Ctrl Pts',(-35.7541930497091,36.1603145930492,37.2073748172342));
#27218=CARTESIAN_POINT('Ctrl Pts',(-35.842059528303,36.1236135760163,37.309227485825));
#27219=CARTESIAN_POINT('Ctrl Pts',(-35.9306411174824,36.0925874485091,37.4121734074567));
#27220=CARTESIAN_POINT('Ctrl Pts',(-36.0192227066619,36.0615613210019,37.5151193290884));
#27221=CARTESIAN_POINT('Ctrl Pts',(-36.108519262757,36.036210133131,37.61915833679));
#27222=CARTESIAN_POINT('Ctrl Pts',(-36.1982194675179,36.0166220465098,37.7239277118411));
#27223=CARTESIAN_POINT('Ctrl Pts',(-36.2879196722787,35.9970339598887,37.8286970868923));
#27224=CARTESIAN_POINT('Ctrl Pts',(-36.3780233802332,35.9832090060956,37.93419665938));
#27225=CARTESIAN_POINT('Ctrl Pts',(-36.4682164713043,35.9751951836183,38.0400586344198));
#27226=CARTESIAN_POINT('Ctrl Pts',(-36.5584095623755,35.9671813611409,38.1459206094595));
#27227=CARTESIAN_POINT('Ctrl Pts',(-36.6486918903018,35.9649786828061,38.2521448153794));
#27228=CARTESIAN_POINT('Ctrl Pts',(-36.7387487221623,35.968594650789,38.3583609441637));
#27229=CARTESIAN_POINT('Ctrl Pts',(-36.8288055540228,35.9722106187718,38.464577072948));
#27230=CARTESIAN_POINT('Ctrl Pts',(-36.9186367437849,35.9816452270589,38.5707849523611));
#27231=CARTESIAN_POINT('Ctrl Pts',(-37.0079291388729,35.9968654303896,38.6766143417166));
#27232=CARTESIAN_POINT('Ctrl Pts',(-37.0972215339608,36.0120856337203,38.7824437310722));
#27233=CARTESIAN_POINT('Ctrl Pts',(-37.1859749895875,36.0330914072835,38.88789445877));
#27234=CARTESIAN_POINT('Ctrl Pts',(-37.2738801156494,36.0598093896721,38.9925989313764));
#27235=CARTESIAN_POINT('Ctrl Pts',(-37.3617852417113,36.0865273720607,39.0973034039828));
#27236=CARTESIAN_POINT('Ctrl Pts',(-37.4488418956745,36.118957519839,39.2012614517275));
#27237=CARTESIAN_POINT('Ctrl Pts',(-37.5347466057807,36.1569866675378,39.304110689855));
#27238=CARTESIAN_POINT('Ctrl Pts',(-37.6206513158869,36.1950158152366,39.4069599279825));
#27239=CARTESIAN_POINT('Ctrl Pts',(-37.705403942848,36.2386439010982,39.5087001897343));
#27240=CARTESIAN_POINT('Ctrl Pts',(-37.7887090478619,36.2877187449007,39.6089768241292));
#27241=CARTESIAN_POINT('Ctrl Pts',(-37.8720141528758,36.3367935887032,39.7092534585241));
#27242=CARTESIAN_POINT('Ctrl Pts',(-37.9538716008697,36.391315110797,39.8080663029763));
#27243=CARTESIAN_POINT('Ctrl Pts',(-38.0339960446261,36.4510931772414,39.9050709114673));
#27244=CARTESIAN_POINT('Ctrl Pts',(-38.1141204883824,36.5108712436857,40.0020755199584));
#27245=CARTESIAN_POINT('Ctrl Pts',(-38.1925117979841,36.5759057574937,40.097271735207));
#27246=CARTESIAN_POINT('Ctrl Pts',(-38.2688967061126,36.6459699563737,40.1903277162358));
#27247=CARTESIAN_POINT('Ctrl Pts',(-38.3452816142411,36.7160341552536,40.2833836972645));
#27248=CARTESIAN_POINT('Ctrl Pts',(-38.4196599970392,36.7911279255571,40.3742992931915));
#27249=CARTESIAN_POINT('Ctrl Pts',(-38.4917725712463,36.8709894571135,40.4627575803402));
#27250=CARTESIAN_POINT('Ctrl Pts',(-38.5638851454534,36.9508509886701,40.5512158674888));
#27251=CARTESIAN_POINT('Ctrl Pts',(-38.6337317941347,37.0354801519608,40.6372167024268));
#27252=CARTESIAN_POINT('Ctrl Pts',(-38.7010690248348,37.1245819135087,40.7204602871234));
#27253=CARTESIAN_POINT('Ctrl Pts',(-34.5541602432366,37.0269902948154,35.9977665285712));
#27254=CARTESIAN_POINT('Ctrl Pts',(-34.6282792954805,36.9396621033914,36.0812119484611));
#27255=CARTESIAN_POINT('Ctrl Pts',(-34.7046959128131,36.8570776877087,36.1675772839025));
#27256=CARTESIAN_POINT('Ctrl Pts',(-34.7831343550503,36.7795345937814,36.2565508787775));
#27257=CARTESIAN_POINT('Ctrl Pts',(-34.8615031475922,36.7020603545216,36.3454454692308));
#27258=CARTESIAN_POINT('Ctrl Pts',(-34.9418900404055,36.6296186217796,36.4369435352596));
#27259=CARTESIAN_POINT('Ctrl Pts',(-35.0240055191768,36.5624699166282,36.5307155327172));
#27260=CARTESIAN_POINT('Ctrl Pts',(-35.1061209979481,36.4953212114768,36.6244875301747));
#27261=CARTESIAN_POINT('Ctrl Pts',(-35.1899649205664,36.4334656497696,36.7205332967659));
#27262=CARTESIAN_POINT('Ctrl Pts',(-35.2752353489086,36.3771256469852,36.818506943316));
#27263=CARTESIAN_POINT('Ctrl Pts',(-35.3605057772508,36.3207856442009,36.9164805898661));
#27264=CARTESIAN_POINT('Ctrl Pts',(-35.4472025637708,36.2699612975081,37.0163819468398));
#27265=CARTESIAN_POINT('Ctrl Pts',(-35.5350135199691,36.2248353183834,37.1178512699157));
#27266=CARTESIAN_POINT('Ctrl Pts',(-35.6228244761675,36.1797093392588,37.2193205929915));
#27267=CARTESIAN_POINT('Ctrl Pts',(-35.7117494501238,36.1402818054887,37.322357706613));
#27268=CARTESIAN_POINT('Ctrl Pts',(-35.8014682500023,36.106694411774,37.4265916006991));
#27269=CARTESIAN_POINT('Ctrl Pts',(-35.8911870498807,36.0731070180593,37.5308254947853));
#27270=CARTESIAN_POINT('Ctrl Pts',(-35.9816995204786,36.0453598222465,37.6362559890205));
#27271=CARTESIAN_POINT('Ctrl Pts',(-36.0726797711134,36.0235524845427,37.7425034778403));
#27272=CARTESIAN_POINT('Ctrl Pts',(-36.1636600217483,36.0017451468388,37.8487509666601));
#27273=CARTESIAN_POINT('Ctrl Pts',(-36.255107895051,35.9858777047353,37.9558152662862));
#27274=CARTESIAN_POINT('Ctrl Pts',(-36.3466941468655,35.9760070685835,38.0633109076383));
#27275=CARTESIAN_POINT('Ctrl Pts',(-36.4382803986801,35.9661364324317,38.1708065489904));
#27276=CARTESIAN_POINT('Ctrl Pts',(-36.5300048706022,35.9622626190992,38.2787333461486));
#27277=CARTESIAN_POINT('Ctrl Pts',(-36.6215373343988,35.9643993812032,38.3867027405372));
#27278=CARTESIAN_POINT('Ctrl Pts',(-36.7130697981954,35.9665361433072,38.4946721349258));
#27279=CARTESIAN_POINT('Ctrl Pts',(-36.8044100955656,35.9746834769709,38.6026839398195));
#27280=CARTESIAN_POINT('Ctrl Pts',(-36.8952293905873,35.9888118796016,38.7103493032797));
#27281=CARTESIAN_POINT('Ctrl Pts',(-36.9860486856089,36.0029402822323,38.8180146667399));
#27282=CARTESIAN_POINT('Ctrl Pts',(-37.0763468212224,36.0230497292377,38.9253334025781));
#27283=CARTESIAN_POINT('Ctrl Pts',(-37.1657987201138,36.0490676764313,39.0319191636385));
#27284=CARTESIAN_POINT('Ctrl Pts',(-37.2552506190054,36.0750856236247,39.138504924699));
#27285=CARTESIAN_POINT('Ctrl Pts',(-37.3438561264855,36.1070120258759,39.2443575266683));
#27286=CARTESIAN_POINT('Ctrl Pts',(-37.4312962630486,36.1447318205671,39.3490959072212));
#27287=CARTESIAN_POINT('Ctrl Pts',(-37.5187363996116,36.1824516152582,39.453834287774));
#27288=CARTESIAN_POINT('Ctrl Pts',(-37.6050110140502,36.2259647370456,39.5574582657969));
#27289=CARTESIAN_POINT('Ctrl Pts',(-37.6898095199542,36.2751144338207,39.6595948057618));
#27290=CARTESIAN_POINT('Ctrl Pts',(-37.7746080258582,36.3242641305957,39.7617313457267));
#27291=CARTESIAN_POINT('Ctrl Pts',(-37.857930276589,36.3790503172715,39.8623802710219));
#27292=CARTESIAN_POINT('Ctrl Pts',(-37.9394763137113,36.4392756810004,39.9611792570969));
#27293=CARTESIAN_POINT('Ctrl Pts',(-38.0210223508336,36.4995010447292,40.0599782431719));
#27294=CARTESIAN_POINT('Ctrl Pts',(-38.1007920333314,36.565165481293,40.1569271191858));
#27295=CARTESIAN_POINT('Ctrl Pts',(-38.178498189151,36.6360325375495,40.2516768786658));
#27296=CARTESIAN_POINT('Ctrl Pts',(-38.2562043449706,36.706899593806,40.3464266381459));
#27297=CARTESIAN_POINT('Ctrl Pts',(-38.3318468397324,36.7829691471553,40.4389771172502));
#27298=CARTESIAN_POINT('Ctrl Pts',(-38.4051533541858,36.8639673060839,40.5289951388672));
#27299=CARTESIAN_POINT('Ctrl Pts',(-38.4784598686392,36.9449654650124,40.6190131604841));
#27300=CARTESIAN_POINT('Ctrl Pts',(-38.5494302760069,37.0308920894196,40.7064985689482));
#27301=CARTESIAN_POINT('Ctrl Pts',(-38.6178090694252,37.121437820586,40.7911364139259));
#27302=CARTESIAN_POINT('Ctrl Pts',(-34.4174636369452,37.0920493708544,36.0044534955695));
#27303=CARTESIAN_POINT('Ctrl Pts',(-34.4915103886568,37.0009023997844,36.0876630582019));
#27304=CARTESIAN_POINT('Ctrl Pts',(-34.5679972742404,36.9145644290366,36.1739686895439));
#27305=CARTESIAN_POINT('Ctrl Pts',(-34.6466394145708,36.8333570035688,36.263048938941));
#27306=CARTESIAN_POINT('Ctrl Pts',(-34.7252117243315,36.7522216865249,36.3520500892121));
#27307=CARTESIAN_POINT('Ctrl Pts',(-34.8059353179264,36.6762079572462,36.443820767926));
#27308=CARTESIAN_POINT('Ctrl Pts',(-34.8885100776198,36.6055984229273,36.5380197860067));
#27309=CARTESIAN_POINT('Ctrl Pts',(-34.9710848373132,36.5349888886083,36.6322188040875));
#27310=CARTESIAN_POINT('Ctrl Pts',(-35.0555106106353,36.4697836796259,36.7288459876017));
#27311=CARTESIAN_POINT('Ctrl Pts',(-35.1414735157231,36.4102252187812,36.8275420917456));
#27312=CARTESIAN_POINT('Ctrl Pts',(-35.2274364208109,36.3506667579364,36.9262381958896));
#27313=CARTESIAN_POINT('Ctrl Pts',(-35.3149362989387,36.2967551552008,37.0270030384264));
#27314=CARTESIAN_POINT('Ctrl Pts',(-35.4036478392012,36.2486908455082,37.129461991381));
#27315=CARTESIAN_POINT('Ctrl Pts',(-35.4923593794637,36.2006265358157,37.2319209443357));
#27316=CARTESIAN_POINT('Ctrl Pts',(-35.5822824180598,36.1584096079143,37.3360738185234));
#27317=CARTESIAN_POINT('Ctrl Pts',(-35.6730826351516,36.1221970177602,37.4415333897958));
#27318=CARTESIAN_POINT('Ctrl Pts',(-35.7638828522433,36.0859844276062,37.5469929610681));
#27319=CARTESIAN_POINT('Ctrl Pts',(-35.855560080173,36.055776242064,37.6537590346999));
#27320=CARTESIAN_POINT('Ctrl Pts',(-35.9477734773,36.0316847704579,37.7614346710745));
#27321=CARTESIAN_POINT('Ctrl Pts',(-36.039986874427,36.0075932988519,37.8691103074492));
#27322=CARTESIAN_POINT('Ctrl Pts',(-36.1327362704844,35.9896185856657,37.9776953077495));
#27323=CARTESIAN_POINT('Ctrl Pts',(-36.2256768376776,35.9778274580804,38.0867859698732));
#27324=CARTESIAN_POINT('Ctrl Pts',(-36.3186174048707,35.9660363304952,38.195876631997));
#27325=CARTESIAN_POINT('Ctrl Pts',(-36.4117489715901,35.9604288102826,38.3054727545143));
#27326=CARTESIAN_POINT('Ctrl Pts',(-36.5047252891902,35.9610257453286,38.415166876128));
#27327=CARTESIAN_POINT('Ctrl Pts',(-36.5977016067903,35.9616226803746,38.5248609977418));
#27328=CARTESIAN_POINT('Ctrl Pts',(-36.6905225035954,35.9684240695771,38.6346529159078));
#27329=CARTESIAN_POINT('Ctrl Pts',(-36.7828428859823,35.9814046264313,38.7441344413914));
#27330=CARTESIAN_POINT('Ctrl Pts',(-36.8751632683692,35.9943851832855,38.853615966875));
#27331=CARTESIAN_POINT('Ctrl Pts',(-36.9669829658735,36.0135448838234,38.9627868975245));
#27332=CARTESIAN_POINT('Ctrl Pts',(-37.0579606071748,36.0388124952658,39.0712413528399));
#27333=CARTESIAN_POINT('Ctrl Pts',(-37.1489382484762,36.0640801067081,39.1796958081554));
#27334=CARTESIAN_POINT('Ctrl Pts',(-37.2390736655894,36.0954555823994,39.2874335878816));
#27335=CARTESIAN_POINT('Ctrl Pts',(-37.3280317490861,36.1328222732128,39.3940541397503));
#27336=CARTESIAN_POINT('Ctrl Pts',(-37.4169898325828,36.1701889640262,39.500674691619));
#27337=CARTESIAN_POINT('Ctrl Pts',(-37.5047704182067,36.2135468009659,39.6061778187612));
#27338=CARTESIAN_POINT('Ctrl Pts',(-37.5910471514259,36.2627345863541,39.7101712769985));
#27339=CARTESIAN_POINT('Ctrl Pts',(-37.6773238846452,36.3119223717422,39.8141647352358));
#27340=CARTESIAN_POINT('Ctrl Pts',(-37.7620966061544,36.3669400147562,39.91664833255));
#27341=CARTESIAN_POINT('Ctrl Pts',(-37.8450501441915,36.4275829683767,40.0172410509039));
#27342=CARTESIAN_POINT('Ctrl Pts',(-37.9280036822286,36.4882259219973,40.1178337692578));
#27343=CARTESIAN_POINT('Ctrl Pts',(-38.0091378836244,36.5544940742505,40.2165354229125));
#27344=CARTESIAN_POINT('Ctrl Pts',(-38.0881511040673,36.6261410504777,40.3129790545077));
#27345=CARTESIAN_POINT('Ctrl Pts',(-38.1671643245102,36.697788026705,40.4094226861029));
#27346=CARTESIAN_POINT('Ctrl Pts',(-38.2440564181065,36.7748136946141,40.5036081175607));
#27347=CARTESIAN_POINT('Ctrl Pts',(-38.3185415120401,36.8569316847805,40.5951851821307));
#27348=CARTESIAN_POINT('Ctrl Pts',(-38.3930266059737,36.9390496749468,40.6867622467008));
#27349=CARTESIAN_POINT('Ctrl Pts',(-38.465104562712,37.026259835744,40.7757307752912));
#27350=CARTESIAN_POINT('Ctrl Pts',(-38.5345074076489,37.1182379333905,40.8617599967831));
#27351=CARTESIAN_POINT('Ctrl Pts',(-34.2807670306538,37.1571084468935,36.0111404625678));
#27352=CARTESIAN_POINT('Ctrl Pts',(-34.3547414818331,37.0621426961774,36.0941141679427));
#27353=CARTESIAN_POINT('Ctrl Pts',(-34.4312986356677,36.9720511703645,36.1803600951854));
#27354=CARTESIAN_POINT('Ctrl Pts',(-34.5101444740912,36.8871794133564,36.2695469991044));
#27355=CARTESIAN_POINT('Ctrl Pts',(-34.5889203010707,36.8023830185282,36.3586547091934));
#27356=CARTESIAN_POINT('Ctrl Pts',(-34.6699805954473,36.7227972927127,36.4506980005925));
#27357=CARTESIAN_POINT('Ctrl Pts',(-34.7530146360628,36.6487269292264,36.5453240392963));
#27358=CARTESIAN_POINT('Ctrl Pts',(-34.8360486766783,36.5746565657399,36.6399500780003));
#27359=CARTESIAN_POINT('Ctrl Pts',(-34.9210563007041,36.5061017094822,36.7371586784375));
#27360=CARTESIAN_POINT('Ctrl Pts',(-35.0077116825375,36.4433247905771,36.8365772401753));
#27361=CARTESIAN_POINT('Ctrl Pts',(-35.0943670643709,36.3805478716719,36.9359958019131));
#27362=CARTESIAN_POINT('Ctrl Pts',(-35.1826700341066,36.3235490128934,37.0376241300129));
#27363=CARTESIAN_POINT('Ctrl Pts',(-35.2722821584332,36.272546372633,37.1410727128464));
#27364=CARTESIAN_POINT('Ctrl Pts',(-35.3618942827598,36.2215437323726,37.2445212956798));
#27365=CARTESIAN_POINT('Ctrl Pts',(-35.4528153859958,36.1765374103399,37.3497899304337));
#27366=CARTESIAN_POINT('Ctrl Pts',(-35.5446970203009,36.1376996237464,37.4564751788924));
#27367=CARTESIAN_POINT('Ctrl Pts',(-35.6365786546059,36.0988618371529,37.563160427351));
#27368=CARTESIAN_POINT('Ctrl Pts',(-35.7294206398673,36.0661926618815,37.6712620803793));
#27369=CARTESIAN_POINT('Ctrl Pts',(-35.8228671834865,36.0398170563733,37.7803658643088));
#27370=CARTESIAN_POINT('Ctrl Pts',(-35.9163137271057,36.013441450865,37.8894696482382));
#27371=CARTESIAN_POINT('Ctrl Pts',(-36.0103646459177,35.993359466596,37.9995753492128));
#27372=CARTESIAN_POINT('Ctrl Pts',(-36.1046595284896,35.9796478475772,38.1102610321082));
#27373=CARTESIAN_POINT('Ctrl Pts',(-36.1989544110615,35.9659362285585,38.2209467150036));
#27374=CARTESIAN_POINT('Ctrl Pts',(-36.2934930725781,35.9585950014659,38.3322121628799));
#27375=CARTESIAN_POINT('Ctrl Pts',(-36.3879132439816,35.957652109454,38.4436310117189));
#27376=CARTESIAN_POINT('Ctrl Pts',(-36.4823334153852,35.9567092174422,38.5550498605578));
#27377=CARTESIAN_POINT('Ctrl Pts',(-36.5766349116251,35.9621646621833,38.6666218919961));
#27378=CARTESIAN_POINT('Ctrl Pts',(-36.6704563813773,35.973997373261,38.7779195795031));
#27379=CARTESIAN_POINT('Ctrl Pts',(-36.7642778511296,35.9858300843386,38.8892172670101));
#27380=CARTESIAN_POINT('Ctrl Pts',(-36.8576191105247,36.0040400384092,39.0002403924709));
#27381=CARTESIAN_POINT('Ctrl Pts',(-36.9501224942359,36.0285573141003,39.1105635420414));
#27382=CARTESIAN_POINT('Ctrl Pts',(-37.042625877947,36.0530745897914,39.2208866916118));
#27383=CARTESIAN_POINT('Ctrl Pts',(-37.1342912046932,36.083899138923,39.3305096490948));
#27384=CARTESIAN_POINT('Ctrl Pts',(-37.2247672351236,36.1209127258585,39.4390123722794));
#27385=CARTESIAN_POINT('Ctrl Pts',(-37.3152432655539,36.1579263127941,39.547515095464));
#27386=CARTESIAN_POINT('Ctrl Pts',(-37.4045298223632,36.2011288648863,39.6548973717255));
#27387=CARTESIAN_POINT('Ctrl Pts',(-37.4922847828977,36.2503547388875,39.7607477482352));
#27388=CARTESIAN_POINT('Ctrl Pts',(-37.5800397434322,36.2995806128888,39.8665981247448));
#27389=CARTESIAN_POINT('Ctrl Pts',(-37.6662629357198,36.3548297122409,39.9709163940781));
#27390=CARTESIAN_POINT('Ctrl Pts',(-37.7506239746718,36.4158902557531,40.0733028447109));
#27391=CARTESIAN_POINT('Ctrl Pts',(-37.8349850136237,36.4769507992654,40.1756892953438));
#27392=CARTESIAN_POINT('Ctrl Pts',(-37.9174837339175,36.543822667208,40.2761437266394));
#27393=CARTESIAN_POINT('Ctrl Pts',(-37.9978040189836,36.616249563406,40.3742812303496));
#27394=CARTESIAN_POINT('Ctrl Pts',(-38.0781243040497,36.688676459604,40.4724187340598));
#27395=CARTESIAN_POINT('Ctrl Pts',(-38.1562659964805,36.766658242073,40.5682391178711));
#27396=CARTESIAN_POINT('Ctrl Pts',(-38.2319296698944,36.8498960634771,40.6613752253943));
#27397=CARTESIAN_POINT('Ctrl Pts',(-38.3075933433082,36.9331338848813,40.7545113329175));
#27398=CARTESIAN_POINT('Ctrl Pts',(-38.3807788494171,37.0216275820683,40.8449629816342));
#27399=CARTESIAN_POINT('Ctrl Pts',(-38.4512057458726,37.115038046195,40.9323835796403));
#27400=CARTESIAN_POINT('Ctrl Pts',(-34.1460670485564,37.2242742219759,36.0197904648656));
#27401=CARTESIAN_POINT('Ctrl Pts',(-34.2198633028138,37.1254709932035,36.1023985558072));
#27402=CARTESIAN_POINT('Ctrl Pts',(-34.2963896997116,37.0315989199376,36.1884614659634));
#27403=CARTESIAN_POINT('Ctrl Pts',(-34.3753432965714,36.9430291072631,36.2776384801598));
#27404=CARTESIAN_POINT('Ctrl Pts',(-34.4542267863025,36.8545379404703,36.3667363093075));
#27405=CARTESIAN_POINT('Ctrl Pts',(-34.5355330030382,36.7713398060557,36.4589425288971));
#27406=CARTESIAN_POINT('Ctrl Pts',(-34.618940697983,36.6937630110328,36.5538928082319));
#27407=CARTESIAN_POINT('Ctrl Pts',(-34.7023483929277,36.61618621601,36.6488430875667));
#27408=CARTESIAN_POINT('Ctrl Pts',(-34.7878573922997,36.5442309215851,36.7465372288016));
#27409=CARTESIAN_POINT('Ctrl Pts',(-34.8751298724766,36.4781810345725,36.8465892569098));
#27410=CARTESIAN_POINT('Ctrl Pts',(-34.9624023526535,36.4121311475598,36.9466412850182));
#27411=CARTESIAN_POINT('Ctrl Pts',(-35.0514381318324,36.3519868051728,37.049050991565));
#27412=CARTESIAN_POINT('Ctrl Pts',(-35.1418854798034,36.2979852747439,37.153413805841));
#27413=CARTESIAN_POINT('Ctrl Pts',(-35.2323328277744,36.2439837443151,37.257776620117));
#27414=CARTESIAN_POINT('Ctrl Pts',(-35.3241915561479,36.1961251379842,37.3640923247422));
#27415=CARTESIAN_POINT('Ctrl Pts',(-35.4170988059786,36.1545982125046,37.4719409485585));
#27416=CARTESIAN_POINT('Ctrl Pts',(-35.5100060558093,36.1130712870252,37.5797895723749));
#27417=CARTESIAN_POINT('Ctrl Pts',(-35.6039616336074,36.0778761285799,37.6891708907723));
#27418=CARTESIAN_POINT('Ctrl Pts',(-35.6985944172415,36.04915149517,37.7996528487545));
#27419=CARTESIAN_POINT('Ctrl Pts',(-35.7932272008757,36.0204268617601,37.9101348067368));
#27420=CARTESIAN_POINT('Ctrl Pts',(-35.8885369932823,35.9981728129329,38.0217171742356));
#27421=CARTESIAN_POINT('Ctrl Pts',(-35.984147339783,35.9824770144079,38.1339592242373));
#27422=CARTESIAN_POINT('Ctrl Pts',(-36.0797576862837,35.9667812158829,38.2462012742389));
#27423=CARTESIAN_POINT('Ctrl Pts',(-36.1756683877955,35.9576437001034,38.3591027730317));
#27424=CARTESIAN_POINT('Ctrl Pts',(-36.2715006297025,35.9551003502302,38.4722178016998));
#27425=CARTESIAN_POINT('Ctrl Pts',(-36.3673328716094,35.9525570003569,38.5853328303679));
#27426=CARTESIAN_POINT('Ctrl Pts',(-36.4630864543794,35.9566078214742,38.6986611534001));
#27427=CARTESIAN_POINT('Ctrl Pts',(-36.5583831945893,35.9672366325882,38.811755180936));
#27428=CARTESIAN_POINT('Ctrl Pts',(-36.6536799347991,35.9778654437021,38.924849208472));
#27429=CARTESIAN_POINT('Ctrl Pts',(-36.7485196340419,35.9950722224986,39.0377087050586));
#27430=CARTESIAN_POINT('Ctrl Pts',(-36.8425277261441,36.0187888531204,39.1498879439181));
#27431=CARTESIAN_POINT('Ctrl Pts',(-36.9365358182464,36.0425054837423,39.2620671827775));
#27432=CARTESIAN_POINT('Ctrl Pts',(-37.0297121074911,36.0727319166539,39.3735659303718));
#27433=CARTESIAN_POINT('Ctrl Pts',(-37.1216886023854,36.1093486402811,39.4839438422258));
#27434=CARTESIAN_POINT('Ctrl Pts',(-37.2136650972797,36.1459653639082,39.5943217540799));
#27435=CARTESIAN_POINT('Ctrl Pts',(-37.3044416063403,36.1889723018853,39.703578600413));
#27436=CARTESIAN_POINT('Ctrl Pts',(-37.393659618231,36.2381994916581,39.8112828957086));
#27437=CARTESIAN_POINT('Ctrl Pts',(-37.4828776301218,36.2874266814309,39.9189871910042));
#27438=CARTESIAN_POINT('Ctrl Pts',(-37.5705369591035,36.342874020407,40.025138711051));
#27439=CARTESIAN_POINT('Ctrl Pts',(-37.6562914046025,36.4043224379193,40.1293182359613));
#27440=CARTESIAN_POINT('Ctrl Pts',(-37.7420458501015,36.4657708554316,40.2334977608714));
#27441=CARTESIAN_POINT('Ctrl Pts',(-37.8258952335875,36.5332202234704,40.3357050737716));
#27442=CARTESIAN_POINT('Ctrl Pts',(-37.9075083986571,36.6064040936536,40.4355365302169));
#27443=CARTESIAN_POINT('Ctrl Pts',(-37.9891215637268,36.6795879638368,40.5353679866623));
#27444=CARTESIAN_POINT('Ctrl Pts',(-38.0684983404671,36.7585061837471,40.632823378828));
#27445=CARTESIAN_POINT('Ctrl Pts',(-38.145325231296,36.8428470315601,40.7275178245671));
#27446=CARTESIAN_POINT('Ctrl Pts',(-38.222152122125,36.9271878793732,40.822212270306));
#27447=CARTESIAN_POINT('Ctrl Pts',(-38.2964289670869,37.0169511794669,40.914145572481));
#27448=CARTESIAN_POINT('Ctrl Pts',(-38.3678624026918,37.1117823981211,41.0029546500012));
#27449=CARTESIAN_POINT('Ctrl Pts',(-34.0133169793171,37.2934251222052,36.0303088752264));
#27450=CARTESIAN_POINT('Ctrl Pts',(-34.0868306484354,37.1907737376081,36.1124205074871));
#27451=CARTESIAN_POINT('Ctrl Pts',(-34.1632264785125,37.0931013004299,36.1981758655312));
#27452=CARTESIAN_POINT('Ctrl Pts',(-34.2421929094087,37.0008061104388,36.2872252173864));
#27453=CARTESIAN_POINT('Ctrl Pts',(-34.3210892217803,36.9085928742915,36.3761954975512));
#27454=CARTESIAN_POINT('Ctrl Pts',(-34.4025513971612,36.8217475442532,36.4684537273036));
#27455=CARTESIAN_POINT('Ctrl Pts',(-34.4862478133071,36.7406236567121,36.5636243350232));
#27456=CARTESIAN_POINT('Ctrl Pts',(-34.5699442294529,36.6594997691709,36.6587949427428));
#27457=CARTESIAN_POINT('Ctrl Pts',(-34.6558747010474,36.5840975037473,36.7568777177077));
#27458=CARTESIAN_POINT('Ctrl Pts',(-34.7436894159758,36.5147238135561,36.8574733773083));
#27459=CARTESIAN_POINT('Ctrl Pts',(-34.8315041309041,36.4453501233649,36.958069036909));
#27460=CARTESIAN_POINT('Ctrl Pts',(-34.9212028947314,36.3820051620099,37.0611773584116));
#27461=CARTESIAN_POINT('Ctrl Pts',(-35.0124205551003,36.3249467988416,37.1663786008404));
#27462=CARTESIAN_POINT('Ctrl Pts',(-35.1036382154692,36.2678884356732,37.2715798432691));
#27463=CARTESIAN_POINT('Ctrl Pts',(-35.1963745704102,36.2171167970273,37.3788737736927));
#27464=CARTESIAN_POINT('Ctrl Pts',(-35.2902521019156,36.1728385678428,37.4878236120493));
#27465=CARTESIAN_POINT('Ctrl Pts',(-35.3841296334209,36.1285603386583,37.5967734504059));
#27466=CARTESIAN_POINT('Ctrl Pts',(-35.4791481336318,36.0907756169739,37.7073789554642));
#27467=CARTESIAN_POINT('Ctrl Pts',(-35.5749207942147,36.0596382196272,37.8191898661595));
#27468=CARTESIAN_POINT('Ctrl Pts',(-35.6706934547976,36.0285008222805,37.9310007768548));
#27469=CARTESIAN_POINT('Ctrl Pts',(-35.7672200636977,36.0040108182144,38.0440168456211));
#27470=CARTESIAN_POINT('Ctrl Pts',(-35.8641076732612,35.9862679031475,38.1577779982926));
#27471=CARTESIAN_POINT('Ctrl Pts',(-35.9609952828248,35.9685249880804,38.2715391509643));
#27472=CARTESIAN_POINT('Ctrl Pts',(-36.0582436785282,35.9575292012981,38.386045135657));
#27473=CARTESIAN_POINT('Ctrl Pts',(-36.1554569744145,35.953325305262,38.5008298129453));
#27474=CARTESIAN_POINT('Ctrl Pts',(-36.252670270301,35.9491214092257,38.6156144902337));
#27475=CARTESIAN_POINT('Ctrl Pts',(-36.3498482511257,35.9517094132437,38.7306776059673));
#27476=CARTESIAN_POINT('Ctrl Pts',(-36.4465953175821,35.9610787818779,38.8455507527104));
#27477=CARTESIAN_POINT('Ctrl Pts',(-36.5433423840385,35.970448150512,38.9604238994535));
#27478=CARTESIAN_POINT('Ctrl Pts',(-36.639658321914,35.9865988630172,39.0751068228598));
#27479=CARTESIAN_POINT('Ctrl Pts',(-36.7351510411702,36.0094651718792,39.1891326632086));
#27480=CARTESIAN_POINT('Ctrl Pts',(-36.8306437604265,36.0323314807412,39.3031585035574));
#27481=CARTESIAN_POINT('Ctrl Pts',(-36.9253130496283,36.0619133353305,39.4165270083786));
#27482=CARTESIAN_POINT('Ctrl Pts',(-37.0187735220362,36.0980903116474,39.5287766687835));
#27483=CARTESIAN_POINT('Ctrl Pts',(-37.1122339944442,36.1342672879641,39.6410263291885));
#27484=CARTESIAN_POINT('Ctrl Pts',(-37.2044854431228,36.1770393059071,39.7521568966399));
#27485=CARTESIAN_POINT('Ctrl Pts',(-37.2951523240567,36.2262322459843,39.8617159726101));
#27486=CARTESIAN_POINT('Ctrl Pts',(-37.3858192049906,36.2754251860615,39.9712750485804));
#27487=CARTESIAN_POINT('Ctrl Pts',(-37.4749013174297,36.3310389393525,40.0792623904894));
#27488=CARTESIAN_POINT('Ctrl Pts',(-37.5620360193267,36.39284710928,40.1852383954844));
#27489=CARTESIAN_POINT('Ctrl Pts',(-37.6491707212237,36.4546552792075,40.2912144004794));
#27490=CARTESIAN_POINT('Ctrl Pts',(-37.7343578196495,36.522657728919,40.3951788339138));
#27491=CARTESIAN_POINT('Ctrl Pts',(-37.8172505286675,36.5965776290162,40.496708469688));
#27492=CARTESIAN_POINT('Ctrl Pts',(-37.9001432376856,36.6704975291134,40.5982381054622));
#27493=CARTESIAN_POINT('Ctrl Pts',(-37.9807413737591,36.7503347159268,40.6973327187745));
#27494=CARTESIAN_POINT('Ctrl Pts',(-38.058716832039,36.8357641823352,40.7935889079489));
#27495=CARTESIAN_POINT('Ctrl Pts',(-38.1366922903187,36.9211936487438,40.8898450971234));
#27496=CARTESIAN_POINT('Ctrl Pts',(-38.2120448981555,37.012215205594,40.9832626490344));
#27497=CARTESIAN_POINT('Ctrl Pts',(-38.2844679045839,37.1084583156049,41.0734612726074));
#27498=CARTESIAN_POINT('Ctrl Pts',(-33.7253196498837,37.443445944854,36.0531282538614));
#27499=CARTESIAN_POINT('Ctrl Pts',(-33.798220258942,37.3324461005754,36.1341628337704));
#27500=CARTESIAN_POINT('Ctrl Pts',(-33.8743328281826,37.226528886849,36.2192509666488));
#27501=CARTESIAN_POINT('Ctrl Pts',(-33.9533271021394,37.1261516015003,36.3080233588493));
#27502=CARTESIAN_POINT('Ctrl Pts',(-34.0322512328483,37.025863446521,36.3967169252868));
#27503=CARTESIAN_POINT('Ctrl Pts',(-34.1140517558741,36.9311056339844,36.4890879895414));
#27504=CARTESIAN_POINT('Ctrl Pts',(-34.1983745440842,36.8422864346562,36.584736593143));
#27505=CARTESIAN_POINT('Ctrl Pts',(-34.2826973322941,36.7534672353282,36.6803851967446));
#27506=CARTESIAN_POINT('Ctrl Pts',(-34.3695421753479,36.6705868687782,36.7793111010353));
#27507=CARTESIAN_POINT('Ctrl Pts',(-34.4585332524524,36.5940022863859,36.881086153));
#27508=CARTESIAN_POINT('Ctrl Pts',(-34.547524329557,36.5174177039936,36.9828612049648));
#27509=CARTESIAN_POINT('Ctrl Pts',(-34.6386614188727,36.4471290949209,37.0874851508487));
#27510=CARTESIAN_POINT('Ctrl Pts',(-34.7315502490925,36.3834390239837,37.1945053382339));
#27511=CARTESIAN_POINT('Ctrl Pts',(-34.8244390793125,36.3197489530465,37.301525525619));
#27512=CARTESIAN_POINT('Ctrl Pts',(-34.9190794190056,36.2626575773783,37.4109416878363));
#27513=CARTESIAN_POINT('Ctrl Pts',(-35.0150619477641,36.2124104765838,37.5222805784061));
#27514=CARTESIAN_POINT('Ctrl Pts',(-35.1110444765225,36.1621633757894,37.6336194689758));
#27515=CARTESIAN_POINT('Ctrl Pts',(-35.2083689553143,36.1187606736282,37.746880810608));
#27516=CARTESIAN_POINT('Ctrl Pts',(-35.3066145450565,36.0823888566362,37.8615748447133));
#27517=CARTESIAN_POINT('Ctrl Pts',(-35.4048601347988,36.0460170396441,37.9762688788185));
#27518=CARTESIAN_POINT('Ctrl Pts',(-35.5040265909137,36.0166761971474,38.09239531987));
#27519=CARTESIAN_POINT('Ctrl Pts',(-35.6036851847274,35.9944921235898,38.2094521206313));
#27520=CARTESIAN_POINT('Ctrl Pts',(-35.7033437785412,35.9723080500322,38.3265089213925));
#27521=CARTESIAN_POINT('Ctrl Pts',(-35.8034942620323,35.9572807995434,38.4444957905543));
#27522=CARTESIAN_POINT('Ctrl Pts',(-35.9037037134776,35.9494743979637,38.5629027208967));
#27523=CARTESIAN_POINT('Ctrl Pts',(-36.003913164923,35.941667996384,38.6813096512391));
#27524=CARTESIAN_POINT('Ctrl Pts',(-36.1041813349894,35.941082462185,38.8001363481746));
#27525=CARTESIAN_POINT('Ctrl Pts',(-36.2040748411289,35.9477195077942,38.9188692411561));
#27526=CARTESIAN_POINT('Ctrl Pts',(-36.3039683472685,35.9543565534034,39.0376021341376));
#27527=CARTESIAN_POINT('Ctrl Pts',(-36.4034869409791,35.9682161614792,39.1562409278309));
#27528=CARTESIAN_POINT('Ctrl Pts',(-36.5022005147178,35.9892377225577,39.2742729152236));
#27529=CARTESIAN_POINT('Ctrl Pts',(-36.6009140884566,36.0102592836361,39.3923049026164));
#27530=CARTESIAN_POINT('Ctrl Pts',(-36.6988223966881,36.0384427447144,39.5097297901655));
#27531=CARTESIAN_POINT('Ctrl Pts',(-36.7955023142031,36.073665702312,39.6260401534171));
#27532=CARTESIAN_POINT('Ctrl Pts',(-36.8921822317181,36.1088886599098,39.7423505166686));
#27533=CARTESIAN_POINT('Ctrl Pts',(-36.987633518058,36.1511510258213,39.8575460663928));
#27534=CARTESIAN_POINT('Ctrl Pts',(-37.0814436773156,36.2002696622019,39.9711290339064));
#27535=CARTESIAN_POINT('Ctrl Pts',(-37.1752538365732,36.2493882985826,40.0847120014199));
#27536=CARTESIAN_POINT('Ctrl Pts',(-37.2674226354332,36.3053630827835,40.196682104292));
#27537=CARTESIAN_POINT('Ctrl Pts',(-37.3575517625599,36.3679517248826,40.3065555194336));
#27538=CARTESIAN_POINT('Ctrl Pts',(-37.4476808896867,36.4305403669817,40.4164289345753));
#27539=CARTESIAN_POINT('Ctrl Pts',(-37.5357701209128,36.4997427109428,40.5242053887811));
#27540=CARTESIAN_POINT('Ctrl Pts',(-37.6214387624945,36.5752594060612,40.6294191741335));
#27541=CARTESIAN_POINT('Ctrl Pts',(-37.7071074040762,36.6507761011797,40.7346329594859));
#27542=CARTESIAN_POINT('Ctrl Pts',(-37.7903552429203,36.7326069593742,40.8372838143524));
#27543=CARTESIAN_POINT('Ctrl Pts',(-37.8708224841454,36.8203981514681,40.9369281594897));
#27544=CARTESIAN_POINT('Ctrl Pts',(-37.9512897253705,36.908189343562,41.036572504627));
#27545=CARTESIAN_POINT('Ctrl Pts',(-38.0289761687888,37.0019406510458,41.1332100922236));
#27546=CARTESIAN_POINT('Ctrl Pts',(-38.1035460197056,37.101246817389,41.2264232946562));
#27547=CARTESIAN_POINT('Ctrl Pts',(-33.4464716391097,37.6027954918844,36.0847240772064));
#27548=CARTESIAN_POINT('Ctrl Pts',(-33.5182678730472,37.4833965665413,36.1640670442977));
#27549=CARTESIAN_POINT('Ctrl Pts',(-33.5936274837347,37.3691410204676,36.2479030934173));
#27550=CARTESIAN_POINT('Ctrl Pts',(-33.6722029585856,37.2605528414183,36.3358454797662));
#27551=CARTESIAN_POINT('Ctrl Pts',(-33.7507086620627,37.1520610836308,36.4237097773588));
#27552=CARTESIAN_POINT('Ctrl Pts',(-33.8324242998089,37.0492269351005,36.5156728750437));
#27553=CARTESIAN_POINT('Ctrl Pts',(-33.9169739581447,36.9525210040537,36.6113116112086));
#27554=CARTESIAN_POINT('Ctrl Pts',(-34.0015236164805,36.8558150730067,36.7069503473736));
#27555=CARTESIAN_POINT('Ctrl Pts',(-34.0889070572831,36.7652376288277,36.806264452547));
#27556=CARTESIAN_POINT('Ctrl Pts',(-34.1787224889782,36.681203003299,36.9087972015629));
#27557=CARTESIAN_POINT('Ctrl Pts',(-34.2685379206733,36.5971683777704,37.0113299505787));
#27558=CARTESIAN_POINT('Ctrl Pts',(-34.3607850905433,36.5196768047354,37.1170810548562));
#27559=CARTESIAN_POINT('Ctrl Pts',(-34.4550400125873,36.4490825631191,37.2255644135308));
#27560=CARTESIAN_POINT('Ctrl Pts',(-34.5492949346313,36.3784883215028,37.3340477722053));
#27561=CARTESIAN_POINT('Ctrl Pts',(-34.6455573438433,36.3147916074869,37.4452630802213));
#27562=CARTESIAN_POINT('Ctrl Pts',(-34.7433849450011,36.2582834200688,37.5586993159057));
#27563=CARTESIAN_POINT('Ctrl Pts',(-34.8412125461588,36.2017752326507,37.67213555159));
#27564=CARTESIAN_POINT('Ctrl Pts',(-34.9406050643861,36.1524557285732,37.7877923961955));
#27565=CARTESIAN_POINT('Ctrl Pts',(-35.0411059467308,36.1105499784281,37.9051385885108));
#27566=CARTESIAN_POINT('Ctrl Pts',(-35.1416068290756,36.0686442282829,38.0224847808262));
#27567=CARTESIAN_POINT('Ctrl Pts',(-35.2432157932981,36.0341523479556,38.1415199913194));
#27568=CARTESIAN_POINT('Ctrl Pts',(-35.3454662095403,36.0072314337289,38.2616975841894));
#27569=CARTESIAN_POINT('Ctrl Pts',(-35.4477166257825,35.9803105195023,38.3818751770595));
#27570=CARTESIAN_POINT('Ctrl Pts',(-35.550608207014,35.9609606453576,38.503194814994));
#27571=CARTESIAN_POINT('Ctrl Pts',(-35.6536685185057,35.9492695084397,38.6250994918713));
#27572=CARTESIAN_POINT('Ctrl Pts',(-35.7567288299973,35.9375783715217,38.7470041687487));
#27573=CARTESIAN_POINT('Ctrl Pts',(-35.8599575825441,35.933546003242,38.86949354255));
#27574=CARTESIAN_POINT('Ctrl Pts',(-35.9628808608495,35.9371899107033,38.9920053348079));
#27575=CARTESIAN_POINT('Ctrl Pts',(-36.0658041391548,35.9408338181645,39.1145171270658));
#27576=CARTESIAN_POINT('Ctrl Pts',(-36.1684216544745,35.9521539899298,39.2370509941715));
#27577=CARTESIAN_POINT('Ctrl Pts',(-36.2702623481083,35.9710975931683,39.359044530537));
#27578=CARTESIAN_POINT('Ctrl Pts',(-36.3721030417422,35.9900411964069,39.4810380669025));
#27579=CARTESIAN_POINT('Ctrl Pts',(-36.4731666280375,36.016608176944,39.6024909304591));
#27580=CARTESIAN_POINT('Ctrl Pts',(-36.5729892153952,36.0506758543964,39.722845734098));
#27581=CARTESIAN_POINT('Ctrl Pts',(-36.6728118027528,36.0847435318488,39.8432005377368));
#27582=CARTESIAN_POINT('Ctrl Pts',(-36.771393111214,36.1263118098031,39.9624569440451));
#27583=CARTESIAN_POINT('Ctrl Pts',(-36.8682806608543,36.1751892903995,40.0800676834957));
#27584=CARTESIAN_POINT('Ctrl Pts',(-36.9651682104947,36.2240667709959,40.1976784229463));
#27585=CARTESIAN_POINT('Ctrl Pts',(-37.0603617295996,36.2802533164657,40.3136431658551));
#27586=CARTESIAN_POINT('Ctrl Pts',(-37.153424289896,36.3434905688718,40.4274297664406));
#27587=CARTESIAN_POINT('Ctrl Pts',(-37.2464868501925,36.4067278212778,40.5412163670262));
#27588=CARTESIAN_POINT('Ctrl Pts',(-37.3374181906852,36.4770156027545,40.6528245063355));
#27589=CARTESIAN_POINT('Ctrl Pts',(-37.4258009324191,36.554030963938,40.7617420299664));
#27590=CARTESIAN_POINT('Ctrl Pts',(-37.5141836741531,36.6310463251215,40.8706595535973));
#27591=CARTESIAN_POINT('Ctrl Pts',(-37.6000175692298,36.7147890496724,40.9768861562323));
#27592=CARTESIAN_POINT('Ctrl Pts',(-37.6829086069535,36.8048745550757,41.0799343596235));
#27593=CARTESIAN_POINT('Ctrl Pts',(-37.7657996446773,36.894960060479,41.1829825630148));
#27594=CARTESIAN_POINT('Ctrl Pts',(-37.8457475925048,36.991388093894,41.2828520782612));
#27595=CARTESIAN_POINT('Ctrl Pts',(-37.9223854134262,37.0937159605723,41.3790845625229));
#27596=CARTESIAN_POINT('Ctrl Pts',(-33.1766930776214,37.7705087843601,36.1244244172113));
#27597=CARTESIAN_POINT('Ctrl Pts',(-33.2469057853303,37.6427433806131,36.2014333689329));
#27598=CARTESIAN_POINT('Ctrl Pts',(-33.3210512350507,37.5201296639953,36.2834032413025));
#27599=CARTESIAN_POINT('Ctrl Pts',(-33.3987671367845,37.4032666996501,36.3699335096646));
#27600=CARTESIAN_POINT('Ctrl Pts',(-33.4764140304055,37.2865075041919,36.4563869431656));
#27601=CARTESIAN_POINT('Ctrl Pts',(-33.5576247911777,37.1754892239836,36.5473924025272));
#27602=CARTESIAN_POINT('Ctrl Pts',(-33.6420033278953,37.0707533308666,36.6425060244189));
#27603=CARTESIAN_POINT('Ctrl Pts',(-33.7263818646128,36.9660174377497,36.7376196463106));
#27604=CARTESIAN_POINT('Ctrl Pts',(-33.8139279089859,36.8675642647401,36.836841128309));
#27605=CARTESIAN_POINT('Ctrl Pts',(-33.9042144706173,36.7758739995088,36.9396865349718));
#27606=CARTESIAN_POINT('Ctrl Pts',(-33.9945010322489,36.6841837342774,37.0425319416347));
#27607=CARTESIAN_POINT('Ctrl Pts',(-34.0875278240641,36.5992566683603,37.149000945955));
#27608=CARTESIAN_POINT('Ctrl Pts',(-34.1828411243289,36.5215070181751,37.2585742640763));
#27609=CARTESIAN_POINT('Ctrl Pts',(-34.2781544245936,36.4437573679901,37.3681475821975));
#27610=CARTESIAN_POINT('Ctrl Pts',(-34.3757539302503,36.3731853807473,37.4808248657209));
#27611=CARTESIAN_POINT('Ctrl Pts',(-34.4751636170032,36.3101352584734,37.5960565511047));
#27612=CARTESIAN_POINT('Ctrl Pts',(-34.5745733037561,36.2470851361995,37.7112882364884));
#27613=CARTESIAN_POINT('Ctrl Pts',(-34.675792855523,36.1915570793665,37.8290739573426));
#27614=CARTESIAN_POINT('Ctrl Pts',(-34.778328591915,36.1438219158808,37.9488392347248));
#27615=CARTESIAN_POINT('Ctrl Pts',(-34.8808643283069,36.0960867523952,38.068604512107));
#27616=CARTESIAN_POINT('Ctrl Pts',(-34.9847159233021,36.0561446340336,38.1903489652127));
#27617=CARTESIAN_POINT('Ctrl Pts',(-35.0893768592252,36.0241903710571,38.3134788071787));
#27618=CARTESIAN_POINT('Ctrl Pts',(-35.1940377951484,35.9922361080806,38.4366086491448));
#27619=CARTESIAN_POINT('Ctrl Pts',(-35.2995077392206,35.9682698020891,38.5611234884689));
#27620=CARTESIAN_POINT('Ctrl Pts',(-35.4052722805894,35.9524083441775,38.6864160263084));
#27621=CARTESIAN_POINT('Ctrl Pts',(-35.5110368219582,35.9365468862658,38.8117085641479));
#27622=CARTESIAN_POINT('Ctrl Pts',(-35.6170956243359,35.9287903268657,38.9377784021244));
#27623=CARTESIAN_POINT('Ctrl Pts',(-35.7229314048457,35.9291764969512,39.0640106572437));
#27624=CARTESIAN_POINT('Ctrl Pts',(-35.8287671853555,35.9295626670368,39.190242912363));
#27625=CARTESIAN_POINT('Ctrl Pts',(-35.9343796074835,35.9380915653791,39.316637183259));
#27626=CARTESIAN_POINT('Ctrl Pts',(-36.0392535655137,35.9547215935791,39.4425770046408));
#27627=CARTESIAN_POINT('Ctrl Pts',(-36.144127523544,35.971351621779,39.5685168260227));
#27628=CARTESIAN_POINT('Ctrl Pts',(-36.2482626840209,35.996082726959,39.6940017974544));
#27629=CARTESIAN_POINT('Ctrl Pts',(-36.3511511463227,36.0287942874002,39.8184198886456));
#27630=CARTESIAN_POINT('Ctrl Pts',(-36.4540396086244,36.0615058478414,39.9428379798368));
#27631=CARTESIAN_POINT('Ctrl Pts',(-36.5556810456084,36.1021977595337,40.0661887951901));
#27632=CARTESIAN_POINT('Ctrl Pts',(-36.6555797193503,36.1506715548338,40.1878707134216));
#27633=CARTESIAN_POINT('Ctrl Pts',(-36.7554783930923,36.1991453501339,40.3095526316531));
#27634=CARTESIAN_POINT('Ctrl Pts',(-36.853633985956,36.2554008749145,40.4295652658654));
#27635=CARTESIAN_POINT('Ctrl Pts',(-36.949567761598,36.3191637528529,40.5473232761837));
#27636=CARTESIAN_POINT('Ctrl Pts',(-37.04550153724,36.3829266307912,40.6650812865021));
#27637=CARTESIAN_POINT('Ctrl Pts',(-37.1392131906308,36.4541966591475,40.7805842985054));
#27638=CARTESIAN_POINT('Ctrl Pts',(-37.2302456599391,36.5326262311041,40.8932689672078));
#27639=CARTESIAN_POINT('Ctrl Pts',(-37.3212781292474,36.6110558030609,41.0059536359101));
#27640=CARTESIAN_POINT('Ctrl Pts',(-37.4096311250278,36.6966446692444,41.1158196030214));
#27641=CARTESIAN_POINT('Ctrl Pts',(-37.4948737213283,36.7889753853261,41.2223310172326));
#27642=CARTESIAN_POINT('Ctrl Pts',(-37.5801163176289,36.8813061014078,41.3288424314437));
#27643=CARTESIAN_POINT('Ctrl Pts',(-37.6622482434134,36.9803783738144,41.4319989540929));
#27644=CARTESIAN_POINT('Ctrl Pts',(-37.7408689148655,37.0857089953691,41.5312974579708));
#27645=CARTESIAN_POINT('',(-37.7834004681043,37.0875767698756,41.4956185460356));
#27646=CARTESIAN_POINT('Ctrl Pts',(-41.7981279794346,37.2631014686576,38.1264711628116));
#27647=CARTESIAN_POINT('Ctrl Pts',(-41.7952803682454,37.2626276178739,38.1282941998091));
#27648=CARTESIAN_POINT('Ctrl Pts',(-41.7924327570584,37.2621537670904,38.1301172368054));
#27649=CARTESIAN_POINT('Ctrl Pts',(-41.7895851458665,37.2616799163062,38.1319402738046));
#27650=CARTESIAN_POINT('Ctrl Pts',(-41.7888732430902,37.2615614536138,38.1323960330406));
#27651=CARTESIAN_POINT('Ctrl Pts',(-41.7881613402824,37.261442990916,38.1328517922966));
#27652=CARTESIAN_POINT('Ctrl Pts',(-41.7874494374748,37.2613245282183,38.1333075515525));
#27653=CARTESIAN_POINT('Ctrl Pts',(-41.7870934860748,37.2612652968701,38.133535431178));
#27654=CARTESIAN_POINT('Ctrl Pts',(-41.7867375346748,37.2612060655218,38.1337633108035));
#27655=CARTESIAN_POINT('Ctrl Pts',(-41.7863815832788,37.2611468341743,38.1339911904264));
#27656=CARTESIAN_POINT('Ctrl Pts',(-41.7860256318321,37.2610876028183,38.1342190700819));
#27657=CARTESIAN_POINT('Ctrl Pts',(-41.7856628656225,37.2610301617684,38.1344560559244));
#27658=CARTESIAN_POINT('Ctrl Pts',(-41.7853034269248,37.2609721218352,38.1346890419301));
#27659=CARTESIAN_POINT('Ctrl Pts',(-41.7838656722769,37.2607399621266,38.1356209858621));
#27660=CARTESIAN_POINT('Ctrl Pts',(-41.7824297932713,37.2605103116342,38.1365552928376));
#27661=CARTESIAN_POINT('Ctrl Pts',(-41.780995781495,37.2602831590315,38.1374919521413));
#27662=CARTESIAN_POINT('Ctrl Pts',(-41.7752597343898,37.259374548621,38.1412385893563));
#27663=CARTESIAN_POINT('Ctrl Pts',(-41.7695535667904,37.2585059112087,38.1450228712984));
#27664=CARTESIAN_POINT('Ctrl Pts',(-41.7638757728966,37.257675231489,38.1488428994769));
#27665=CARTESIAN_POINT('Ctrl Pts',(-41.7581979790448,37.2568445517755,38.1526629276272));
#27666=CARTESIAN_POINT('Ctrl Pts',(-41.7525485535461,37.2560518229013,38.1565186957688));
#27667=CARTESIAN_POINT('Ctrl Pts',(-41.7469251703319,37.2552939330802,38.1604072733946));
#27668=CARTESIAN_POINT('Ctrl Pts',(-41.7413017870347,37.254536043248,38.1642958510777));
#27669=CARTESIAN_POINT('Ctrl Pts',(-41.7357044238504,37.2538129628078,38.1682172103118));
#27670=CARTESIAN_POINT('Ctrl Pts',(-41.7301301522264,37.2531207739776,38.1721676615473));
#27671=CARTESIAN_POINT('Ctrl Pts',(-41.7245558806842,37.2524285851575,38.176118112725));
#27672=CARTESIAN_POINT('Ctrl Pts',(-41.7190046733824,37.251767251399,38.1800976214849));
#27673=CARTESIAN_POINT('Ctrl Pts',(-41.7134733845952,37.2511325643884,38.184102224671));
#27674=CARTESIAN_POINT('Ctrl Pts',(-41.7079420957676,37.2504978773732,38.1881068278865));
#27675=CARTESIAN_POINT('Ctrl Pts',(-41.7024307055449,37.2498898104708,38.1921365004449));
#27676=CARTESIAN_POINT('Ctrl Pts',(-41.6969362138226,37.2493043501777,38.1961874626515));
#27677=CARTESIAN_POINT('Ctrl Pts',(-41.6914417221003,37.2487188898845,38.200238424858));
#27678=CARTESIAN_POINT('Ctrl Pts',(-41.6859641201875,37.2481560245742,38.2043106657638));
#27679=CARTESIAN_POINT('Ctrl Pts',(-41.6805007672794,37.2476122214099,38.2084008583392));
#27680=CARTESIAN_POINT('Ctrl Pts',(-41.675037414332,37.2470684182417,38.2124910509441));
#27681=CARTESIAN_POINT('Ctrl Pts',(-41.6695883098069,37.2465436764404,38.2165991944852));
#27682=CARTESIAN_POINT('Ctrl Pts',(-41.6641512373951,37.2460350310546,38.2207224967357));
#27683=CARTESIAN_POINT('Ctrl Pts',(-41.6532770926885,37.2450177402938,38.2289691011478));
#27684=CARTESIAN_POINT('Ctrl Pts',(-41.6424507433835,37.2440643896428,38.2372759208019));
#27685=CARTESIAN_POINT('Ctrl Pts',(-41.6316590585708,37.24315741273,38.2456264126654));
#27686=CARTESIAN_POINT('Ctrl Pts',(-41.6208673736816,37.2422504358108,38.2539769045882));
#27687=CARTESIAN_POINT('Ctrl Pts',(-41.6101104832692,37.2413900065215,38.2623712324819));
#27688=CARTESIAN_POINT('Ctrl Pts',(-41.5993797204532,37.2405645304145,38.2707984773402));
#27689=CARTESIAN_POINT('Ctrl Pts',(-41.5886489577125,37.2397390543133,38.2792257221395));
#27690=CARTESIAN_POINT('Ctrl Pts',(-41.5779444113226,37.238948650129,38.287685995721));
#27691=CARTESIAN_POINT('Ctrl Pts',(-41.5672602276774,37.2381854869781,38.2961719233939));
#27692=CARTESIAN_POINT('Ctrl Pts',(-41.5565760439582,37.2374223238219,38.3046578511256));
#27693=CARTESIAN_POINT('Ctrl Pts',(-41.5459122765069,37.2366864733018,38.31316950038));
#27694=CARTESIAN_POINT('Ctrl Pts',(-41.5352648323389,37.2359724598726,38.3217017145931));
#27695=CARTESIAN_POINT('Ctrl Pts',(-41.524617388244,37.2352584464482,38.3302339287476));
#27696=CARTESIAN_POINT('Ctrl Pts',(-41.5139862993864,37.2345663128625,38.3387867481182));
#27697=CARTESIAN_POINT('Ctrl Pts',(-41.5033686034439,37.2338920961565,38.3473564406103));
#27698=CARTESIAN_POINT('Ctrl Pts',(-41.492750907465,37.2332178794481,38.3559261331318));
#27699=CARTESIAN_POINT('Ctrl Pts',(-41.4821466239335,37.2325616057495,38.3645127233828));
#27700=CARTESIAN_POINT('Ctrl Pts',(-41.4715535415973,37.2319203168746,38.3731134255079));
#27701=CARTESIAN_POINT('Ctrl Pts',(-41.4503673768902,37.2306377391226,38.3903148297865));
#27702=CARTESIAN_POINT('Ctrl Pts',(-41.4292256929265,37.2294146671707,38.4075722733206));
#27703=CARTESIAN_POINT('Ctrl Pts',(-41.4081164361093,37.228234975863,38.4248705703345));
#27704=CARTESIAN_POINT('Ctrl Pts',(-41.3870071793618,37.2270552845593,38.4421688672915));
#27705=CARTESIAN_POINT('Ctrl Pts',(-41.3659305268728,37.2259192108381,38.4595082408637));
#27706=CARTESIAN_POINT('Ctrl Pts',(-41.3448787787704,37.2248164539037,38.4768789903342));
#27707=CARTESIAN_POINT('Ctrl Pts',(-41.3238270305998,37.2237136969658,38.4942497398608));
#27708=CARTESIAN_POINT('Ctrl Pts',(-41.3028002730303,37.2226443721514,38.5116519739034));
#27709=CARTESIAN_POINT('Ctrl Pts',(-41.2817932595768,37.2216014607763,38.5290790826552));
#27710=CARTESIAN_POINT('Ctrl Pts',(-41.2607862461898,37.2205585494046,38.5465061913519));
#27711=CARTESIAN_POINT('Ctrl Pts',(-41.2397990228863,37.2195421129669,38.5639582326701));
#27712=CARTESIAN_POINT('Ctrl Pts',(-41.2188278343381,37.2185471276308,38.5814304754436));
#27713=CARTESIAN_POINT('Ctrl Pts',(-41.1978566457246,37.2175521422917,38.5989027182715));
#27714=CARTESIAN_POINT('Ctrl Pts',(-41.1769015182199,37.2165786433093,38.6163951957561));
#27715=CARTESIAN_POINT('Ctrl Pts',(-41.1559596578763,37.2156228929745,38.6339043879306));
#27716=CARTESIAN_POINT('Ctrl Pts',(-41.1350177975965,37.2146671426426,38.6514135800517));
#27717=CARTESIAN_POINT('Ctrl Pts',(-41.1140892204956,37.2137291623866,38.6689395070428));
#27718=CARTESIAN_POINT('Ctrl Pts',(-41.0931717822014,37.2128060834914,38.6864794673073));
#27719=CARTESIAN_POINT('Ctrl Pts',(-41.0722543438446,37.2118830045934,38.7040194276243));
#27720=CARTESIAN_POINT('Ctrl Pts',(-41.0513480545069,37.2109748407181,38.7215734340807));
#27721=CARTESIAN_POINT('Ctrl Pts',(-41.0304512257111,37.2100793330414,38.7391393594415));
#27722=CARTESIAN_POINT('Ctrl Pts',(-40.9886575682115,37.2082883176918,38.774271210086));
#27723=CARTESIAN_POINT('Ctrl Pts',(-40.9469015299109,37.2065476288515,38.8094504554401));
#27724=CARTESIAN_POINT('Ctrl Pts',(-40.905173253682,37.2048440797747,38.8446646769593));
#27725=CARTESIAN_POINT('Ctrl Pts',(-40.8634449773944,37.2031405306954,38.879878898528));
#27726=CARTESIAN_POINT('Ctrl Pts',(-40.8217445702088,37.2014742645636,38.9151282311048));
#27727=CARTESIAN_POINT('Ctrl Pts',(-40.7800652132294,37.1998361591428,38.9504040838741));
#27728=CARTESIAN_POINT('Ctrl Pts',(-40.7383858563063,37.1981980537242,38.9856799365958));
#27729=CARTESIAN_POINT('Ctrl Pts',(-40.6967276065313,37.1965881851929,39.0209823812487));
#27730=CARTESIAN_POINT('Ctrl Pts',(-40.6550854902778,37.1949998998914,39.056305151788));
#27731=CARTESIAN_POINT('Ctrl Pts',(-40.6134433739704,37.1934116145878,39.0916279223729));
#27732=CARTESIAN_POINT('Ctrl Pts',(-40.5718174239146,37.1918449562999,39.1269710600792));
#27733=CARTESIAN_POINT('Ctrl Pts',(-40.5302038548951,37.1902948612125,39.1623297960873));
#27734=CARTESIAN_POINT('Ctrl Pts',(-40.488590285927,37.188744766127,39.1976885320517));
#27735=CARTESIAN_POINT('Ctrl Pts',(-40.4469891179915,37.1872112609928,39.2330628915102));
#27736=CARTESIAN_POINT('Ctrl Pts',(-40.4053973662081,37.1856903526728,39.2684491139483));
#27737=CARTESIAN_POINT('Ctrl Pts',(-40.3638056143756,37.1841694443511,39.3038353364282));
#27738=CARTESIAN_POINT('Ctrl Pts',(-40.3222232915335,37.1826611500186,39.3392334380622));
#27739=CARTESIAN_POINT('Ctrl Pts',(-40.2806479706236,37.1811622227862,39.3746403611105));
#27740=CARTESIAN_POINT('Ctrl Pts',(-40.1974973288739,37.178164368324,39.4454542071473));
#27741=CARTESIAN_POINT('Ctrl Pts',(-40.1143744321379,37.1752036308053,39.5163030078588));
#27742=CARTESIAN_POINT('Ctrl Pts',(-40.0312642571702,37.1722599123143,39.5871678361448));
#27743=CARTESIAN_POINT('Ctrl Pts',(-39.9481540821605,37.1693161938219,39.6580326644667));
#27744=CARTESIAN_POINT('Ctrl Pts',(-39.8650567681428,37.1663896806089,39.7289136957646));
#27745=CARTESIAN_POINT('Ctrl Pts',(-39.78196079965,37.1634649674229,39.799796422228));
#27746=CARTESIAN_POINT('Ctrl Pts',(-39.6988648311948,37.1605402542383,39.8706791486594));
#27747=CARTESIAN_POINT('Ctrl Pts',(-39.6157702857781,37.1576174447775,39.941563667912));
#27748=CARTESIAN_POINT('Ctrl Pts',(-39.5326675761395,37.1546837133193,40.0124379014345));
#27749=CARTESIAN_POINT('Ctrl Pts',(-39.4495648664821,37.1517499818605,40.0833121349731));
#27750=CARTESIAN_POINT('Ctrl Pts',(-39.3664540409006,37.1488053930167,40.1541761436298));
#27751=CARTESIAN_POINT('Ctrl Pts',(-39.2833265166636,37.1458384649135,40.2250191144136));
#27752=CARTESIAN_POINT('Ctrl Pts',(-39.2001989924265,37.1428715368103,40.2958620851973));
#27753=CARTESIAN_POINT('Ctrl Pts',(-39.1170548033789,37.1398823147253,40.366684060748));
#27754=CARTESIAN_POINT('Ctrl Pts',(-39.0338857649331,37.1368598494162,40.4374747296777));
#27755=CARTESIAN_POINT('Ctrl Pts',(-38.9507167264778,37.1338373841067,40.5082653986154));
#27756=CARTESIAN_POINT('Ctrl Pts',(-38.8675228655626,37.1307817116108,40.5790247948705));
#27757=CARTESIAN_POINT('Ctrl Pts',(-38.7842959451795,37.127681812559,40.6497425410132));
#27758=CARTESIAN_POINT('Ctrl Pts',(-38.7010690248156,37.124581913508,40.7204602871396));
#27759=CARTESIAN_POINT('Ctrl Pts',(-38.6178090694157,37.1214378205856,40.791136413934));
#27760=CARTESIAN_POINT('Ctrl Pts',(-38.5345074076489,37.1182379333905,40.8617599967831));
#27761=CARTESIAN_POINT('Ctrl Pts',(-38.4512057458678,37.1150380461948,40.9323835796444));
#27762=CARTESIAN_POINT('Ctrl Pts',(-38.3678624026822,37.1117823981208,41.0029546500094));
#27763=CARTESIAN_POINT('Ctrl Pts',(-38.2844679045694,37.1084583156043,41.0734612726197));
#27764=CARTESIAN_POINT('Ctrl Pts',(-38.1176789083584,37.1018101505721,41.2144745178281));
#27765=CARTESIAN_POINT('Ctrl Pts',(-37.9506870299514,37.0948905721936,41.3552321610306));
#27766=CARTESIAN_POINT('Ctrl Pts',(-37.7834004681043,37.0875767698756,41.4956185460356));
#27767=CARTESIAN_POINT('Origin',(-35.6284929434833,40.9281765976896,39.1278840755075));
#27768=CARTESIAN_POINT('Ctrl Pts',(-38.0398886763086,37.4073630839359,41.7808966890464));
#27769=CARTESIAN_POINT('Ctrl Pts',(-37.9326177918203,37.4114807225354,41.8852044318755));
#27770=CARTESIAN_POINT('Ctrl Pts',(-37.8096166958413,37.3290227884235,41.8633979578226));
#27771=CARTESIAN_POINT('Ctrl Pts',(-37.6866155998624,37.2465648543116,41.8415914837696));
#27772=CARTESIAN_POINT('Ctrl Pts',(-37.6777121386978,37.1645658239806,41.7166875597931));
#27773=CARTESIAN_POINT('Ctrl Pts',(-37.6688086775333,37.0825667936495,41.5917836358167));
#27774=CARTESIAN_POINT('Ctrl Pts',(-37.7834004681593,37.087576769944,41.4956185461047));
#27775=CARTESIAN_POINT('Ctrl Pts',(-40.7814290969457,40.6059367497034,44.4740514613886));
#27776=CARTESIAN_POINT('Ctrl Pts',(-38.5287405218227,40.692407160327,46.6645140616453));
#27777=CARTESIAN_POINT('Ctrl Pts',(-35.9457175052688,38.960790543309,46.2065781063563));
#27778=CARTESIAN_POINT('Ctrl Pts',(-33.362694488715,37.229173926291,45.7486421510673));
#27779=CARTESIAN_POINT('Ctrl Pts',(-33.1757218041875,35.5071942886757,43.1256597465504));
#27780=CARTESIAN_POINT('Ctrl Pts',(-32.9887491196601,33.7852146510605,40.5026773420335));
#27781=CARTESIAN_POINT('Ctrl Pts',(-35.3951767237337,33.8904241532856,38.4832104573036));
#27782=CARTESIAN_POINT('Ctrl Pts',(-38.6265215723274,44.4465365775852,42.1063169907319));
#27783=CARTESIAN_POINT('Ctrl Pts',(-36.3738329972119,44.5330069882085,44.2967795909812));
#27784=CARTESIAN_POINT('Ctrl Pts',(-33.7908099806667,42.8013903711963,43.8388436356938));
#27785=CARTESIAN_POINT('Ctrl Pts',(-31.2077869641214,41.0697737541841,43.3809076804063));
#27786=CARTESIAN_POINT('Ctrl Pts',(-31.0208142795946,39.3477941165746,40.7579252758982));
#27787=CARTESIAN_POINT('Ctrl Pts',(-30.8338415950678,37.6258144789651,38.13494287139));
#27788=CARTESIAN_POINT('Ctrl Pts',(-33.2402691991333,37.7310239811898,36.1154759866669));
#27789=CARTESIAN_POINT('',(-38.0398886763558,37.4073630839945,41.7808966890927));
#27790=CARTESIAN_POINT('Origin',(-35.8849811517349,41.2479629118085,39.4131622185645));
#27791=CARTESIAN_POINT('Origin',(-37.9028116553955,37.2474344007039,41.6462389504159));
#27792=CARTESIAN_POINT('Ctrl Pts',(-41.7981279794346,37.2631014686576,38.1264711628116));
#27793=CARTESIAN_POINT('Ctrl Pts',(-41.7981279794346,37.2631014686576,38.1264711628116));
#27794=CARTESIAN_POINT('Ctrl Pts',(-41.7981279794346,37.2631014686576,38.1264711628116));
#27795=CARTESIAN_POINT('Ctrl Pts',(-41.7981279794346,37.2631014686576,38.1264711628116));
#27796=CARTESIAN_POINT('Ctrl Pts',(-41.7981279794346,37.2631014686576,38.1264711628116));
#27797=CARTESIAN_POINT('Ctrl Pts',(-41.7981279794346,37.2631014686576,38.1264711628116));
#27798=CARTESIAN_POINT('Ctrl Pts',(-41.7981279794346,37.2631014686576,38.1264711628116));
#27799=CARTESIAN_POINT('Ctrl Pts',(-41.7981279794346,37.2631014686576,38.1264711628116));
#27800=CARTESIAN_POINT('Ctrl Pts',(-41.7981279794346,37.2631014686576,38.1264711628116));
#27801=CARTESIAN_POINT('Ctrl Pts',(-41.7981279794346,37.2631014686576,38.1264711628116));
#27802=CARTESIAN_POINT('Ctrl Pts',(-41.7981279794346,37.2631014686576,38.1264711628116));
#27803=CARTESIAN_POINT('Ctrl Pts',(-41.7981279794346,37.2631014686576,38.1264711628116));
#27804=CARTESIAN_POINT('Ctrl Pts',(-41.7981279794346,37.2631014686576,38.1264711628116));
#27805=CARTESIAN_POINT('Ctrl Pts',(-41.7981279794346,37.2631014686576,38.1264711628116));
#27806=CARTESIAN_POINT('Ctrl Pts',(-41.7981279794346,37.2631014686576,38.1264711628116));
#27807=CARTESIAN_POINT('Ctrl Pts',(-41.7981279794346,37.2631014686576,38.1264711628116));
#27808=CARTESIAN_POINT('Ctrl Pts',(-41.7981279794346,37.2631014686576,38.1264711628116));
#27809=CARTESIAN_POINT('Ctrl Pts',(-41.7981279794346,37.2631014686576,38.1264711628116));
#27810=CARTESIAN_POINT('Ctrl Pts',(-41.7981279794346,37.2631014686576,38.1264711628116));
#27811=CARTESIAN_POINT('Ctrl Pts',(-41.7981279794346,37.2631014686576,38.1264711628116));
#27812=CARTESIAN_POINT('Ctrl Pts',(-41.7981279794346,37.2631014686576,38.1264711628116));
#27813=CARTESIAN_POINT('Ctrl Pts',(-41.7981279794346,37.2631014686576,38.1264711628116));
#27814=CARTESIAN_POINT('Ctrl Pts',(-41.7981279794346,37.2631014686576,38.1264711628116));
#27815=CARTESIAN_POINT('Ctrl Pts',(-41.7981279794346,37.2631014686576,38.1264711628116));
#27816=CARTESIAN_POINT('Ctrl Pts',(-41.7981279794346,37.2631014686576,38.1264711628116));
#27817=CARTESIAN_POINT('Ctrl Pts',(-41.7981279794346,37.2631014686576,38.1264711628116));
#27818=CARTESIAN_POINT('Ctrl Pts',(-41.7981279794346,37.2631014686576,38.1264711628116));
#27819=CARTESIAN_POINT('Ctrl Pts',(-41.7981279794346,37.2631014686576,38.1264711628116));
#27820=CARTESIAN_POINT('Ctrl Pts',(-41.7981279794346,37.2631014686576,38.1264711628116));
#27821=CARTESIAN_POINT('Ctrl Pts',(-41.7981279794346,37.2631014686576,38.1264711628116));
#27822=CARTESIAN_POINT('Ctrl Pts',(-41.7981279794346,37.2631014686576,38.1264711628116));
#27823=CARTESIAN_POINT('Ctrl Pts',(-41.7981279794346,37.2631014686576,38.1264711628116));
#27824=CARTESIAN_POINT('Ctrl Pts',(-41.7981279794346,37.2631014686576,38.1264711628116));
#27825=CARTESIAN_POINT('Ctrl Pts',(-41.7981279794346,37.2631014686576,38.1264711628116));
#27826=CARTESIAN_POINT('Ctrl Pts',(-41.7981279794346,37.2631014686576,38.1264711628116));
#27827=CARTESIAN_POINT('Ctrl Pts',(-41.7981279794346,37.2631014686576,38.1264711628116));
#27828=CARTESIAN_POINT('Ctrl Pts',(-41.7981279794346,37.2631014686576,38.1264711628116));
#27829=CARTESIAN_POINT('Ctrl Pts',(-41.7981279794346,37.2631014686576,38.1264711628116));
#27830=CARTESIAN_POINT('Ctrl Pts',(-41.7981279794346,37.2631014686576,38.1264711628116));
#27831=CARTESIAN_POINT('Ctrl Pts',(-41.7981279794346,37.2631014686576,38.1264711628116));
#27832=CARTESIAN_POINT('Ctrl Pts',(-41.7981279794346,37.2631014686576,38.1264711628116));
#27833=CARTESIAN_POINT('Ctrl Pts',(-41.7981279794346,37.2631014686576,38.1264711628116));
#27834=CARTESIAN_POINT('Ctrl Pts',(-41.7981279794346,37.2631014686576,38.1264711628116));
#27835=CARTESIAN_POINT('Ctrl Pts',(-41.7981279794346,37.2631014686576,38.1264711628116));
#27836=CARTESIAN_POINT('Ctrl Pts',(-41.7981279794346,37.2631014686576,38.1264711628116));
#27837=CARTESIAN_POINT('Ctrl Pts',(-41.7981279794346,37.2631014686576,38.1264711628116));
#27838=CARTESIAN_POINT('Ctrl Pts',(-41.7981279794346,37.2631014686576,38.1264711628116));
#27839=CARTESIAN_POINT('Ctrl Pts',(-41.7981279794346,37.2631014686576,38.1264711628116));
#27840=CARTESIAN_POINT('Ctrl Pts',(-41.7981279794346,37.2631014686576,38.1264711628116));
#27841=CARTESIAN_POINT('Ctrl Pts',(-41.7960245110197,37.2635554058993,38.1291218701799));
#27842=CARTESIAN_POINT('Ctrl Pts',(-41.7962311144902,37.2637489024678,38.1292476999627));
#27843=CARTESIAN_POINT('Ctrl Pts',(-41.7964377179608,37.2639423990362,38.1293735297455));
#27844=CARTESIAN_POINT('Ctrl Pts',(-41.7966443214313,37.2641358956046,38.1294993595282));
#27845=CARTESIAN_POINT('Ctrl Pts',(-41.7968509249018,37.264329392173,38.129625189311));
#27846=CARTESIAN_POINT('Ctrl Pts',(-41.7970575283723,37.2645228887414,38.1297510190938));
#27847=CARTESIAN_POINT('Ctrl Pts',(-41.7972641318428,37.2647163853098,38.1298768488765));
#27848=CARTESIAN_POINT('Ctrl Pts',(-41.7974707353134,37.2649098818782,38.1300026786593));
#27849=CARTESIAN_POINT('Ctrl Pts',(-41.7976773387839,37.2651033784466,38.1301285084421));
#27850=CARTESIAN_POINT('Ctrl Pts',(-41.7978839422544,37.265296875015,38.1302543382248));
#27851=CARTESIAN_POINT('Ctrl Pts',(-41.7980905457249,37.2654903715834,38.1303801680076));
#27852=CARTESIAN_POINT('Ctrl Pts',(-41.7982971491955,37.2656838681519,38.1305059977904));
#27853=CARTESIAN_POINT('Ctrl Pts',(-41.798503752666,37.2658773647203,38.1306318275731));
#27854=CARTESIAN_POINT('Ctrl Pts',(-41.7987103561365,37.2660708612887,38.1307576573559));
#27855=CARTESIAN_POINT('Ctrl Pts',(-41.798916959607,37.2662643578571,38.1308834871387));
#27856=CARTESIAN_POINT('Ctrl Pts',(-41.7991235630775,37.2664578544255,38.1310093169214));
#27857=CARTESIAN_POINT('Ctrl Pts',(-41.7993301665481,37.2666513509939,38.1311351467042));
#27858=CARTESIAN_POINT('Ctrl Pts',(-41.7995367700186,37.2668448475623,38.131260976487));
#27859=CARTESIAN_POINT('Ctrl Pts',(-41.7997433734891,37.2670383441307,38.1313868062697));
#27860=CARTESIAN_POINT('Ctrl Pts',(-41.7999499769596,37.2672318406991,38.1315126360525));
#27861=CARTESIAN_POINT('Ctrl Pts',(-41.8001565804302,37.2674253372675,38.1316384658353));
#27862=CARTESIAN_POINT('Ctrl Pts',(-41.8003631839007,37.2676188338359,38.131764295618));
#27863=CARTESIAN_POINT('Ctrl Pts',(-41.8005697873712,37.2678123304043,38.1318901254008));
#27864=CARTESIAN_POINT('Ctrl Pts',(-41.8007763908417,37.2680058269728,38.1320159551836));
#27865=CARTESIAN_POINT('Ctrl Pts',(-41.8009829943122,37.2681993235412,38.1321417849663));
#27866=CARTESIAN_POINT('Ctrl Pts',(-41.8011895977828,37.2683928201096,38.1322676147491));
#27867=CARTESIAN_POINT('Ctrl Pts',(-41.8013962012533,37.268586316678,38.1323934445319));
#27868=CARTESIAN_POINT('Ctrl Pts',(-41.8016028047238,37.2687798132464,38.1325192743146));
#27869=CARTESIAN_POINT('Ctrl Pts',(-41.8018094081943,37.2689733098148,38.1326451040974));
#27870=CARTESIAN_POINT('Ctrl Pts',(-41.8020160116648,37.2691668063832,38.1327709338802));
#27871=CARTESIAN_POINT('Ctrl Pts',(-41.8022226151354,37.2693603029516,38.1328967636629));
#27872=CARTESIAN_POINT('Ctrl Pts',(-41.8024292186059,37.26955379952,38.1330225934457));
#27873=CARTESIAN_POINT('Ctrl Pts',(-41.8026358220764,37.2697472960884,38.1331484232285));
#27874=CARTESIAN_POINT('Ctrl Pts',(-41.8028424255469,37.2699407926569,38.1332742530112));
#27875=CARTESIAN_POINT('Ctrl Pts',(-41.8030490290175,37.2701342892253,38.133400082794));
#27876=CARTESIAN_POINT('Ctrl Pts',(-41.803255632488,37.2703277857937,38.1335259125768));
#27877=CARTESIAN_POINT('Ctrl Pts',(-41.8034622359585,37.2705212823621,38.1336517423595));
#27878=CARTESIAN_POINT('Ctrl Pts',(-41.803668839429,37.2707147789305,38.1337775721423));
#27879=CARTESIAN_POINT('Ctrl Pts',(-41.8038754428995,37.2709082754989,38.1339034019251));
#27880=CARTESIAN_POINT('Ctrl Pts',(-41.8040820463701,37.2711017720673,38.1340292317078));
#27881=CARTESIAN_POINT('Ctrl Pts',(-41.8042886498406,37.2712952686357,38.1341550614906));
#27882=CARTESIAN_POINT('Ctrl Pts',(-41.8044952533111,37.2714887652041,38.1342808912734));
#27883=CARTESIAN_POINT('Ctrl Pts',(-41.8047018567816,37.2716822617725,38.1344067210561));
#27884=CARTESIAN_POINT('Ctrl Pts',(-41.8049084602521,37.2718757583409,38.1345325508389));
#27885=CARTESIAN_POINT('Ctrl Pts',(-41.8051150637227,37.2720692549094,38.1346583806217));
#27886=CARTESIAN_POINT('Ctrl Pts',(-41.8053216671932,37.2722627514778,38.1347842104044));
#27887=CARTESIAN_POINT('Ctrl Pts',(-41.805528454281,37.2724564200148,38.1349101520175));
#27888=CARTESIAN_POINT('Ctrl Pts',(-41.8057352413689,37.2726500885519,38.1350360936305));
#27889=CARTESIAN_POINT('Ctrl Pts',(-41.8059420284567,37.272843757089,38.1351620352436));
#27890=CARTESIAN_POINT('Ctrl Pts',(-41.7939210565382,37.2640093183082,38.1317725928578));
#27891=CARTESIAN_POINT('Ctrl Pts',(-41.7943397763188,37.2644044471742,38.1320324388456));
#27892=CARTESIAN_POINT('Ctrl Pts',(-41.7947584589863,37.2647996421852,38.1322922440548));
#27893=CARTESIAN_POINT('Ctrl Pts',(-41.7951771045444,37.2651949033453,38.1325520084888));
#27894=CARTESIAN_POINT('Ctrl Pts',(-41.7955957501026,37.2655901645054,38.1328117729228));
#27895=CARTESIAN_POINT('Ctrl Pts',(-41.7960143585513,37.2659854918146,38.1330714965815));
#27896=CARTESIAN_POINT('Ctrl Pts',(-41.7964329298944,37.2663808852769,38.1333311794681));
#27897=CARTESIAN_POINT('Ctrl Pts',(-41.7968515012375,37.2667762787392,38.1335908623546));
#27898=CARTESIAN_POINT('Ctrl Pts',(-41.7972700354749,37.2671717383546,38.133850504469));
#27899=CARTESIAN_POINT('Ctrl Pts',(-41.7976885326102,37.2675672641272,38.1341101058145));
#27900=CARTESIAN_POINT('Ctrl Pts',(-41.7981070297456,37.2679627898998,38.1343697071599));
#27901=CARTESIAN_POINT('Ctrl Pts',(-41.7985254897789,37.2683583818297,38.1346292677364));
#27902=CARTESIAN_POINT('Ctrl Pts',(-41.7989439127138,37.2687540399209,38.134888787547));
#27903=CARTESIAN_POINT('Ctrl Pts',(-41.7993623356487,37.2691496980122,38.1351483073576));
#27904=CARTESIAN_POINT('Ctrl Pts',(-41.7997807214852,37.2695454222648,38.1354077864023));
#27905=CARTESIAN_POINT('Ctrl Pts',(-41.800199070227,37.269941212683,38.1356672246842));
#27906=CARTESIAN_POINT('Ctrl Pts',(-41.8006174189687,37.2703370031012,38.1359266629662));
#27907=CARTESIAN_POINT('Ctrl Pts',(-41.8010357306157,37.2707328596848,38.1361860604855));
#27908=CARTESIAN_POINT('Ctrl Pts',(-41.8014540051714,37.2711287824383,38.136445417245));
#27909=CARTESIAN_POINT('Ctrl Pts',(-41.8018722797272,37.2715247051917,38.1367047740046));
#27910=CARTESIAN_POINT('Ctrl Pts',(-41.8022905171918,37.2719206941149,38.1369640900045));
#27911=CARTESIAN_POINT('Ctrl Pts',(-41.8027087175689,37.2723167492119,38.1372233652478));
#27912=CARTESIAN_POINT('Ctrl Pts',(-41.8031269179459,37.272712804309,38.1374826404911));
#27913=CARTESIAN_POINT('Ctrl Pts',(-41.8035450812354,37.2731089255801,38.1377418749778));
#27914=CARTESIAN_POINT('Ctrl Pts',(-41.8039632074408,37.2735051130292,38.1380010687111));
#27915=CARTESIAN_POINT('Ctrl Pts',(-41.8043813336463,37.2739013004784,38.1382602624443));
#27916=CARTESIAN_POINT('Ctrl Pts',(-41.8047994227677,37.2742975541059,38.138519415424));
#27917=CARTESIAN_POINT('Ctrl Pts',(-41.8052174748088,37.2746938739157,38.1387785276532));
#27918=CARTESIAN_POINT('Ctrl Pts',(-41.8056355268498,37.2750901937255,38.1390376398824));
#27919=CARTESIAN_POINT('Ctrl Pts',(-41.8060535418103,37.2754865797179,38.1392967113611));
#27920=CARTESIAN_POINT('Ctrl Pts',(-41.8064715196939,37.275883031897,38.1395557420923));
#27921=CARTESIAN_POINT('Ctrl Pts',(-41.8068894975776,37.276279484076,38.1398147728236));
#27922=CARTESIAN_POINT('Ctrl Pts',(-41.8073074383844,37.2766760024418,38.1400737628074));
#27923=CARTESIAN_POINT('Ctrl Pts',(-41.8077253421178,37.2770725869988,38.1403327120467));
#27924=CARTESIAN_POINT('Ctrl Pts',(-41.8081432458511,37.2774691715558,38.140591661286));
#27925=CARTESIAN_POINT('Ctrl Pts',(-41.8085611125111,37.2778658223038,38.1408505697809));
#27926=CARTESIAN_POINT('Ctrl Pts',(-41.8089789421013,37.2782625392472,38.1411094375343));
#27927=CARTESIAN_POINT('Ctrl Pts',(-41.8093967716914,37.2786592561906,38.1413683052878));
#27928=CARTESIAN_POINT('Ctrl Pts',(-41.8098145642117,37.2790560393296,38.1416271322997));
#27929=CARTESIAN_POINT('Ctrl Pts',(-41.8102323196656,37.2794528886683,38.1418859185732));
#27930=CARTESIAN_POINT('Ctrl Pts',(-41.8106500751195,37.2798497380071,38.1421447048466));
#27931=CARTESIAN_POINT('Ctrl Pts',(-41.8110677935071,37.2802466535456,38.1424034503816));
#27932=CARTESIAN_POINT('Ctrl Pts',(-41.8114854748317,37.2806436352884,38.142662155181));
#27933=CARTESIAN_POINT('Ctrl Pts',(-41.8119031561564,37.2810406170312,38.1429208599804));
#27934=CARTESIAN_POINT('Ctrl Pts',(-41.8123208004182,37.2814376649782,38.1431795240443));
#27935=CARTESIAN_POINT('Ctrl Pts',(-41.8127384076205,37.2818347791339,38.1434381473755));
#27936=CARTESIAN_POINT('Ctrl Pts',(-41.8131563859682,37.2822322462219,38.1436970005564));
#27937=CARTESIAN_POINT('Ctrl Pts',(-41.8135743271905,37.2826297796363,38.1439558129322));
#27938=CARTESIAN_POINT('Ctrl Pts',(-41.813992231291,37.2830273793816,38.1442145845059));
#27939=CARTESIAN_POINT('Ctrl Pts',(-41.79181757419,37.2644632803828,38.1344232849166));
#27940=CARTESIAN_POINT('Ctrl Pts',(-41.7924539645127,37.2650685630173,38.1348259073185));
#27941=CARTESIAN_POINT('Ctrl Pts',(-41.7930902341437,37.2656740607558,38.1352283971087));
#27942=CARTESIAN_POINT('Ctrl Pts',(-41.7937263829759,37.2662797734963,38.1356307542194));
#27943=CARTESIAN_POINT('Ctrl Pts',(-41.7943625318081,37.2668854862368,38.1360331113302));
#27944=CARTESIAN_POINT('Ctrl Pts',(-41.7949985598417,37.2674914139794,38.1364353357616));
#27945=CARTESIAN_POINT('Ctrl Pts',(-41.7956344669696,37.2680975566223,38.1368374274459));
#27946=CARTESIAN_POINT('Ctrl Pts',(-41.7962703740977,37.2687036992651,38.1372395191303));
#27947=CARTESIAN_POINT('Ctrl Pts',(-41.7969061603201,37.2693100568083,38.1376414780677));
#27948=CARTESIAN_POINT('Ctrl Pts',(-41.7975418255301,37.2699166291498,38.1380433041906));
#27949=CARTESIAN_POINT('Ctrl Pts',(-41.7981774907402,37.2705232014914,38.1384451303135));
#27950=CARTESIAN_POINT('Ctrl Pts',(-41.7988130349378,37.2711299886313,38.1388468236219));
#27951=CARTESIAN_POINT('Ctrl Pts',(-41.7994484580163,37.2717369904676,38.1392483840483));
#27952=CARTESIAN_POINT('Ctrl Pts',(-41.8000838810948,37.2723439923039,38.1396499444747));
#27953=CARTESIAN_POINT('Ctrl Pts',(-41.8007191830542,37.2729512088367,38.140051372019));
#27954=CARTESIAN_POINT('Ctrl Pts',(-41.8013543637875,37.2735586399639,38.1404526666139));
#27955=CARTESIAN_POINT('Ctrl Pts',(-41.8019895445209,37.2741660710911,38.1408539612088));
#27956=CARTESIAN_POINT('Ctrl Pts',(-41.8026246040285,37.2747737168126,38.1412551228543));
#27957=CARTESIAN_POINT('Ctrl Pts',(-41.8032595422033,37.2753815770265,38.1416561514829));
#27958=CARTESIAN_POINT('Ctrl Pts',(-41.8038944803782,37.2759894372404,38.1420571801114));
#27959=CARTESIAN_POINT('Ctrl Pts',(-41.8045292972204,37.2765975119466,38.1424580757232));
#27960=CARTESIAN_POINT('Ctrl Pts',(-41.8051639926234,37.2772058010429,38.1428588382507));
#27961=CARTESIAN_POINT('Ctrl Pts',(-41.8057986880264,37.2778140901392,38.1432596007782));
#27962=CARTESIAN_POINT('Ctrl Pts',(-41.80643326199,37.2784225936257,38.1436602302214));
#27963=CARTESIAN_POINT('Ctrl Pts',(-41.8070677144078,37.2790313114001,38.1440607265132));
#27964=CARTESIAN_POINT('Ctrl Pts',(-41.8077021668256,37.2796400291744,38.1444612228049));
#27965=CARTESIAN_POINT('Ctrl Pts',(-41.8083364976974,37.2802489612367,38.1448615859451));
#27966=CARTESIAN_POINT('Ctrl Pts',(-41.8089707069168,37.2808581074845,38.1452618158665));
#27967=CARTESIAN_POINT('Ctrl Pts',(-41.8096049161361,37.2814672537324,38.1456620457879));
#27968=CARTESIAN_POINT('Ctrl Pts',(-41.810239003703,37.2820766141657,38.1460621424905));
#27969=CARTESIAN_POINT('Ctrl Pts',(-41.8108729695109,37.2826861886823,38.1464621059071));
#27970=CARTESIAN_POINT('Ctrl Pts',(-41.8115069353187,37.2832957631989,38.1468620693236));
#27971=CARTESIAN_POINT('Ctrl Pts',(-41.8121407793675,37.2839055517988,38.1472618994541));
#27972=CARTESIAN_POINT('Ctrl Pts',(-41.8127745015508,37.2845155543793,38.1476615962314));
#27973=CARTESIAN_POINT('Ctrl Pts',(-41.8134082237341,37.2851255569598,38.1480612930087));
#27974=CARTESIAN_POINT('Ctrl Pts',(-41.8140418240518,37.285735773521,38.1484608564328));
#27975=CARTESIAN_POINT('Ctrl Pts',(-41.8146753023975,37.2863462039604,38.1488602864366));
#27976=CARTESIAN_POINT('Ctrl Pts',(-41.8153087807433,37.2869566343999,38.1492597164403));
#27977=CARTESIAN_POINT('Ctrl Pts',(-41.815942137117,37.2875672787175,38.1496590130237));
#27978=CARTESIAN_POINT('Ctrl Pts',(-41.8165753714124,37.2881781368108,38.1500581761196));
#27979=CARTESIAN_POINT('Ctrl Pts',(-41.8172086057077,37.288788994904,38.1504573392156));
#27980=CARTESIAN_POINT('Ctrl Pts',(-41.8178417179246,37.2894000667729,38.1508563688241));
#27981=CARTESIAN_POINT('Ctrl Pts',(-41.8184747079568,37.2900113523147,38.1512552648781));
#27982=CARTESIAN_POINT('Ctrl Pts',(-41.8191076979889,37.2906226378565,38.1516541609321));
#27983=CARTESIAN_POINT('Ctrl Pts',(-41.8197405658363,37.2912341370712,38.1520529234316));
#27984=CARTESIAN_POINT('Ctrl Pts',(-41.8203733113925,37.291845849856,38.1524515523097));
#27985=CARTESIAN_POINT('Ctrl Pts',(-41.8210066192967,37.2924581062961,38.1528505354662));
#27986=CARTESIAN_POINT('Ctrl Pts',(-41.8216398046923,37.2930705766862,38.1532493847636));
#27987=CARTESIAN_POINT('Ctrl Pts',(-41.8222728674726,37.2936832609232,38.1536481001348));
#27988=CARTESIAN_POINT('Ctrl Pts',(-41.7912917036029,37.2645767709014,38.1350859579313));
#27989=CARTESIAN_POINT('Ctrl Pts',(-41.7919825115612,37.2652345919781,38.1355242744368));
#27990=CARTESIAN_POINT('Ctrl Pts',(-41.792673177933,37.2658926653985,38.1359624353721));
#27991=CARTESIAN_POINT('Ctrl Pts',(-41.7933637025837,37.2665509910341,38.1364004406521));
#27992=CARTESIAN_POINT('Ctrl Pts',(-41.7940542272345,37.2672093166697,38.1368384459321));
#27993=CARTESIAN_POINT('Ctrl Pts',(-41.7947446101643,37.2678678945206,38.1372762955566));
#27994=CARTESIAN_POINT('Ctrl Pts',(-41.7954348512385,37.2685267244587,38.1377139894404));
#27995=CARTESIAN_POINT('Ctrl Pts',(-41.7961250923127,37.2691855543967,38.1381516833243));
#27996=CARTESIAN_POINT('Ctrl Pts',(-41.7968151915314,37.2698446364218,38.1385892214674));
#27997=CARTESIAN_POINT('Ctrl Pts',(-41.7975051487601,37.2705039704055,38.1390266037847));
#27998=CARTESIAN_POINT('Ctrl Pts',(-41.7981951059888,37.2711633043892,38.139463986102));
#27999=CARTESIAN_POINT('Ctrl Pts',(-41.7988849212276,37.2718228903316,38.1399012125933));
#28000=CARTESIAN_POINT('Ctrl Pts',(-41.799574594342,37.2724827281042,38.1403382831736));
#28001=CARTESIAN_POINT('Ctrl Pts',(-41.8002642674564,37.2731425658768,38.1407753537539));
#28002=CARTESIAN_POINT('Ctrl Pts',(-41.8009537984464,37.2738026554797,38.1412122684232));
#28003=CARTESIAN_POINT('Ctrl Pts',(-41.8016431871777,37.2744629967841,38.1416490270963));
#28004=CARTESIAN_POINT('Ctrl Pts',(-41.802332575909,37.2751233380886,38.1420857857694));
#28005=CARTESIAN_POINT('Ctrl Pts',(-41.8030218223817,37.2757839310946,38.1425223884465));
#28006=CARTESIAN_POINT('Ctrl Pts',(-41.8037109264613,37.2764447756736,38.1429588350423));
#28007=CARTESIAN_POINT('Ctrl Pts',(-41.8044000305409,37.2771056202526,38.1433952816381));
#28008=CARTESIAN_POINT('Ctrl Pts',(-41.8050889922276,37.2777667164045,38.1438315721529));
#28009=CARTESIAN_POINT('Ctrl Pts',(-41.805777811387,37.2784280640007,38.1442677065014));
#28010=CARTESIAN_POINT('Ctrl Pts',(-41.8064666305465,37.2790894115968,38.1447038408499));
#28011=CARTESIAN_POINT('Ctrl Pts',(-41.8071553071787,37.2797510106372,38.1451398190323));
#28012=CARTESIAN_POINT('Ctrl Pts',(-41.8078438411495,37.2804128609928,38.1455756409637));
#28013=CARTESIAN_POINT('Ctrl Pts',(-41.8085323751204,37.2810747113485,38.1460114628951));
#28014=CARTESIAN_POINT('Ctrl Pts',(-41.8092207664298,37.2817368130194,38.1464471285754));
#28015=CARTESIAN_POINT('Ctrl Pts',(-41.8099090149438,37.2823991658767,38.1468826379199));
#28016=CARTESIAN_POINT('Ctrl Pts',(-41.8105972634578,37.283061518734,38.1473181472643));
#28017=CARTESIAN_POINT('Ctrl Pts',(-41.8112853691762,37.2837241227777,38.1477535002729));
#28018=CARTESIAN_POINT('Ctrl Pts',(-41.8119733319651,37.2843869778787,38.1481886968607));
#28019=CARTESIAN_POINT('Ctrl Pts',(-41.812661294754,37.2850498329797,38.1486238934486));
#28020=CARTESIAN_POINT('Ctrl Pts',(-41.8133491146133,37.285712939138,38.1490589336158));
#28021=CARTESIAN_POINT('Ctrl Pts',(-41.814036791409,37.2863762962244,38.1494938172776));
#28022=CARTESIAN_POINT('Ctrl Pts',(-41.8147244682048,37.2870396533108,38.1499287009394));
#28023=CARTESIAN_POINT('Ctrl Pts',(-41.815412001937,37.2877032613253,38.1503634280958));
#28024=CARTESIAN_POINT('Ctrl Pts',(-41.8160993924716,37.2883671201388,38.1507979986621));
#28025=CARTESIAN_POINT('Ctrl Pts',(-41.8167867830062,37.2890309789523,38.1512325692284));
#28026=CARTESIAN_POINT('Ctrl Pts',(-41.8174740303434,37.2896950885646,38.1516669832047));
#28027=CARTESIAN_POINT('Ctrl Pts',(-41.8181611343491,37.2903594488464,38.1521012405063));
#28028=CARTESIAN_POINT('Ctrl Pts',(-41.8188482383547,37.2910238091284,38.1525354978078));
#28029=CARTESIAN_POINT('Ctrl Pts',(-41.819535199029,37.2916884200798,38.1529695984347));
#28030=CARTESIAN_POINT('Ctrl Pts',(-41.820222016238,37.2923532815713,38.1534035423024));
#28031=CARTESIAN_POINT('Ctrl Pts',(-41.820908833447,37.2930181430628,38.15383748617));
#28032=CARTESIAN_POINT('Ctrl Pts',(-41.8215955071908,37.2936832550944,38.1542712732784));
#28033=CARTESIAN_POINT('Ctrl Pts',(-41.8222820373355,37.2943486175366,38.1547049035432));
#28034=CARTESIAN_POINT('Ctrl Pts',(-41.8229691776288,37.2950145713147,38.1551389191936));
#28035=CARTESIAN_POINT('Ctrl Pts',(-41.8236561740677,37.2956807759487,38.1555727777215));
#28036=CARTESIAN_POINT('Ctrl Pts',(-41.8243430265181,37.2963472313086,38.156006479042));
#28037=CARTESIAN_POINT('Ctrl Pts',(-41.7907658588839,37.2646902153166,38.1357486593688));
#28038=CARTESIAN_POINT('Ctrl Pts',(-41.7915114300167,37.2654011073895,38.1362232160579));
#28039=CARTESIAN_POINT('Ctrl Pts',(-41.7922568357581,37.2661122942323,38.136697591021));
#28040=CARTESIAN_POINT('Ctrl Pts',(-41.7930020759386,37.2668237756833,38.1371717841502));
#28041=CARTESIAN_POINT('Ctrl Pts',(-41.7937473161191,37.2675352571344,38.1376459772793));
#28042=CARTESIAN_POINT('Ctrl Pts',(-41.7944923907387,37.2682470331936,38.1381199885747));
#28043=CARTESIAN_POINT('Ctrl Pts',(-41.7952372996279,37.2689591036991,38.1385938179283));
#28044=CARTESIAN_POINT('Ctrl Pts',(-41.7959822085171,37.2696711742047,38.1390676472819));
#28045=CARTESIAN_POINT('Ctrl Pts',(-41.7967269516758,37.2703835391565,38.1395412946939));
#28046=CARTESIAN_POINT('Ctrl Pts',(-41.7974715289348,37.2710961983927,38.1400147600566));
#28047=CARTESIAN_POINT('Ctrl Pts',(-41.7982161061936,37.2718088576289,38.1404882254192));
#28048=CARTESIAN_POINT('Ctrl Pts',(-41.7989605175528,37.2725218111494,38.1409615087326));
#28049=CARTESIAN_POINT('Ctrl Pts',(-41.7997047628426,37.2732350587921,38.1414346098889));
#28050=CARTESIAN_POINT('Ctrl Pts',(-41.8004490081325,37.2739483064348,38.1419077110453));
#28051=CARTESIAN_POINT('Ctrl Pts',(-41.8011930873532,37.2746618481997,38.1423806300447));
#28052=CARTESIAN_POINT('Ctrl Pts',(-41.8019370003355,37.2753756839244,38.1428533667796));
#28053=CARTESIAN_POINT('Ctrl Pts',(-41.8026809133178,37.2760895196491,38.1433261035146));
#28054=CARTESIAN_POINT('Ctrl Pts',(-41.8034246600615,37.2768036493338,38.143798657985));
#28055=CARTESIAN_POINT('Ctrl Pts',(-41.8041682403976,37.277518072816,38.1442710300836));
#28056=CARTESIAN_POINT('Ctrl Pts',(-41.8049118207338,37.2782324962982,38.1447434021821));
#28057=CARTESIAN_POINT('Ctrl Pts',(-41.8056552346622,37.2789472135778,38.1452155919088));
#28058=CARTESIAN_POINT('Ctrl Pts',(-41.8063984820139,37.2796622244925,38.1456875991561));
#28059=CARTESIAN_POINT('Ctrl Pts',(-41.8071417293656,37.280377235407,38.1461596064035));
#28060=CARTESIAN_POINT('Ctrl Pts',(-41.8078848101404,37.2810925399566,38.1466314311716));
#28061=CARTESIAN_POINT('Ctrl Pts',(-41.8086277241695,37.2818081379785,38.1471030733532));
#28062=CARTESIAN_POINT('Ctrl Pts',(-41.8093706381985,37.2825237360004,38.1475747155347));
#28063=CARTESIAN_POINT('Ctrl Pts',(-41.8101133854818,37.2832396274945,38.1480461751297));
#28064=CARTESIAN_POINT('Ctrl Pts',(-41.8108559658502,37.2839558122982,38.1485174520309));
#28065=CARTESIAN_POINT('Ctrl Pts',(-41.8115985462185,37.2846719971018,38.1489887289321));
#28066=CARTESIAN_POINT('Ctrl Pts',(-41.8123409596722,37.2853884752149,38.1494598231396));
#28067=CARTESIAN_POINT('Ctrl Pts',(-41.8130832060421,37.2861052464746,38.1499307345462));
#28068=CARTESIAN_POINT('Ctrl Pts',(-41.8138254524119,37.2868220177343,38.1504016459528));
#28069=CARTESIAN_POINT('Ctrl Pts',(-41.8145675316981,37.2875390821405,38.1508723745586));
#28070=CARTESIAN_POINT('Ctrl Pts',(-41.8153094437317,37.2882564395303,38.1513429202564));
#28071=CARTESIAN_POINT('Ctrl Pts',(-41.8160513557654,37.28897379692,38.1518134659542));
#28072=CARTESIAN_POINT('Ctrl Pts',(-41.8167931005464,37.2896914472933,38.1522838287441));
#28073=CARTESIAN_POINT('Ctrl Pts',(-41.8175346779063,37.2904093904868,38.1527540085193));
#28074=CARTESIAN_POINT('Ctrl Pts',(-41.8182762552661,37.2911273336803,38.1532241882944));
#28075=CARTESIAN_POINT('Ctrl Pts',(-41.8190176652046,37.2918455696942,38.1536941850546));
#28076=CARTESIAN_POINT('Ctrl Pts',(-41.8197589075531,37.292564098365,38.1541639986931));
#28077=CARTESIAN_POINT('Ctrl Pts',(-41.8205001499017,37.2932826270358,38.1546338123316));
#28078=CARTESIAN_POINT('Ctrl Pts',(-41.8212412246603,37.2940014483635,38.1551034428484));
#28079=CARTESIAN_POINT('Ctrl Pts',(-41.8219821316603,37.2947205621849,38.1555728901367));
#28080=CARTESIAN_POINT('Ctrl Pts',(-41.8227230386603,37.2954396760062,38.1560423374249));
#28081=CARTESIAN_POINT('Ctrl Pts',(-41.8234637779018,37.2961590823209,38.1565116014848));
#28082=CARTESIAN_POINT('Ctrl Pts',(-41.8242043492162,37.2968787809657,38.1569806822093));
#28083=CARTESIAN_POINT('Ctrl Pts',(-41.8249455787079,37.2975991192373,38.1574501798259));
#28084=CARTESIAN_POINT('Ctrl Pts',(-41.8256866399739,37.2983197503587,38.1579194937813));
#28085=CARTESIAN_POINT('Ctrl Pts',(-41.8264275328452,37.2990406741657,38.1583886239685));
#28086=CARTESIAN_POINT('Ctrl Pts',(-41.7902399728789,37.264803733314,38.1364113154429));
#28087=CARTESIAN_POINT('Ctrl Pts',(-41.791040652538,37.2655682301309,38.1369226670485));
#28088=CARTESIAN_POINT('Ctrl Pts',(-41.7918411399332,37.2663330696116,38.1374338074015));
#28089=CARTESIAN_POINT('Ctrl Pts',(-41.7926414348502,37.2670982515513,38.1379447363651));
#28090=CARTESIAN_POINT('Ctrl Pts',(-41.7934417297672,37.2678634334911,38.1384556653286));
#28091=CARTESIAN_POINT('Ctrl Pts',(-41.794241832206,37.2686289578899,38.1389663829027));
#28092=CARTESIAN_POINT('Ctrl Pts',(-41.7950417419526,37.2693948245428,38.1394768889507));
#28093=CARTESIAN_POINT('Ctrl Pts',(-41.795841651699,37.2701606911958,38.1399873949986));
#28094=CARTESIAN_POINT('Ctrl Pts',(-41.7966413687531,37.2709269001031,38.1404976895203));
#28095=CARTESIAN_POINT('Ctrl Pts',(-41.7974408929009,37.2716934510593,38.1410077723793));
#28096=CARTESIAN_POINT('Ctrl Pts',(-41.7982404170486,37.2724600020156,38.1415178552383));
#28097=CARTESIAN_POINT('Ctrl Pts',(-41.7990397482899,37.2732268950209,38.1420277264346));
#28098=CARTESIAN_POINT('Ctrl Pts',(-41.7998388864109,37.2739941298702,38.1425373858316));
#28099=CARTESIAN_POINT('Ctrl Pts',(-41.8006380245318,37.2747613647194,38.1430470452286));
#28100=CARTESIAN_POINT('Ctrl Pts',(-41.8014369695325,37.2755289414123,38.1435564928264));
#28101=CARTESIAN_POINT('Ctrl Pts',(-41.8022357211989,37.2762968597437,38.1440657284886));
#28102=CARTESIAN_POINT('Ctrl Pts',(-41.8030344728653,37.2770647780751,38.1445749641509));
#28103=CARTESIAN_POINT('Ctrl Pts',(-41.8038330311975,37.2778330380449,38.1450839878774));
#28104=CARTESIAN_POINT('Ctrl Pts',(-41.8046313959817,37.2786016394473,38.1455927995322));
#28105=CARTESIAN_POINT('Ctrl Pts',(-41.8054297607659,37.2793702408498,38.146101611187));
#28106=CARTESIAN_POINT('Ctrl Pts',(-41.8062279320023,37.280139183685,38.14661021077));
#28107=CARTESIAN_POINT('Ctrl Pts',(-41.8070259094769,37.2809084677471,38.1471185981449));
#28108=CARTESIAN_POINT('Ctrl Pts',(-41.8078238869517,37.2816777518092,38.1476269855199));
#28109=CARTESIAN_POINT('Ctrl Pts',(-41.8086216706648,37.2824473770983,38.1481351606869));
#28110=CARTESIAN_POINT('Ctrl Pts',(-41.8094192604028,37.2832173434083,38.1486431235099));
#28111=CARTESIAN_POINT('Ctrl Pts',(-41.8102168501408,37.2839873097182,38.1491510863329));
#28112=CARTESIAN_POINT('Ctrl Pts',(-41.8110142459036,37.2847576170491,38.1496588368119));
#28113=CARTESIAN_POINT('Ctrl Pts',(-41.8118114474779,37.2855282651947,38.1501663748111));
#28114=CARTESIAN_POINT('Ctrl Pts',(-41.8126086490522,37.2862989133403,38.1506739128102));
#28115=CARTESIAN_POINT('Ctrl Pts',(-41.8134056564379,37.2870699023006,38.1511812383294));
#28116=CARTESIAN_POINT('Ctrl Pts',(-41.8142024694217,37.2878412318693,38.1516883512329));
#28117=CARTESIAN_POINT('Ctrl Pts',(-41.8149992824055,37.288612561438,38.1521954641365));
#28118=CARTESIAN_POINT('Ctrl Pts',(-41.8157959009875,37.289384231615,38.1527023644243));
#28119=CARTESIAN_POINT('Ctrl Pts',(-41.8165923249543,37.2901562421939,38.1532090519608));
#28120=CARTESIAN_POINT('Ctrl Pts',(-41.8173887489211,37.2909282527728,38.1537157394973));
#28121=CARTESIAN_POINT('Ctrl Pts',(-41.8181849782728,37.2917006037534,38.1542222142824));
#28122=CARTESIAN_POINT('Ctrl Pts',(-41.8189810127963,37.2924732949292,38.1547284761806));
#28123=CARTESIAN_POINT('Ctrl Pts',(-41.8197770473197,37.293245986105,38.1552347380787));
#28124=CARTESIAN_POINT('Ctrl Pts',(-41.8205728870149,37.2940190174758,38.15574078709));
#28125=CARTESIAN_POINT('Ctrl Pts',(-41.8213685316688,37.2947923888349,38.1562466230788));
#28126=CARTESIAN_POINT('Ctrl Pts',(-41.8221641763227,37.2955657601939,38.1567524590677));
#28127=CARTESIAN_POINT('Ctrl Pts',(-41.8229596259354,37.2963394715411,38.1572580820341));
#28128=CARTESIAN_POINT('Ctrl Pts',(-41.8237548802939,37.2971135226694,38.1577634918429));
#28129=CARTESIAN_POINT('Ctrl Pts',(-41.8245501346524,37.2978875737977,38.1582689016516));
#28130=CARTESIAN_POINT('Ctrl Pts',(-41.8253451937568,37.298661964707,38.1587740983027));
#28131=CARTESIAN_POINT('Ctrl Pts',(-41.8261400573941,37.2994366951901,38.1592790816607));
#28132=CARTESIAN_POINT('Ctrl Pts',(-41.8269356274607,37.3002121142093,38.1597845138191));
#28133=CARTESIAN_POINT('Ctrl Pts',(-41.8277310017127,37.3009878734061,38.1602897323052));
#28134=CARTESIAN_POINT('Ctrl Pts',(-41.8285261799368,37.3017639725726,38.1607947369835));
#28135=CARTESIAN_POINT('Ctrl Pts',(-41.7899770298764,37.2648604923127,38.1367426434799));
#28136=CARTESIAN_POINT('Ctrl Pts',(-41.7908052637987,37.2656517915016,38.1372723925438));
#28137=CARTESIAN_POINT('Ctrl Pts',(-41.7916332920208,37.2664434573011,38.1378019155918));
#28138=CARTESIAN_POINT('Ctrl Pts',(-41.792461114306,37.2672354894853,38.1383312124726));
#28139=CARTESIAN_POINT('Ctrl Pts',(-41.7932889365913,37.2680275216694,38.1388605093533));
#28140=CARTESIAN_POINT('Ctrl Pts',(-41.7941165529397,37.268819920238,38.1393895800668));
#28141=CARTESIAN_POINT('Ctrl Pts',(-41.7949439631148,37.2696126849648,38.1399184244618));
#28142=CARTESIAN_POINT('Ctrl Pts',(-41.79577137329,37.2704054496914,38.1404472688569));
#28143=CARTESIAN_POINT('Ctrl Pts',(-41.7965985772918,37.2711985805763,38.1409758869336));
#28144=CARTESIAN_POINT('Ctrl Pts',(-41.7974255748839,37.2719920773926,38.1415042785407));
#28145=CARTESIAN_POINT('Ctrl Pts',(-41.7982525724761,37.2727855742089,38.1420326701479));
#28146=CARTESIAN_POINT('Ctrl Pts',(-41.7990793636585,37.2735794369567,38.1425608352856));
#28147=CARTESIAN_POINT('Ctrl Pts',(-41.799905948195,37.2743736654092,38.143088773803));
#28148=CARTESIAN_POINT('Ctrl Pts',(-41.8007325327315,37.2751678938616,38.1436167123203));
#28149=CARTESIAN_POINT('Ctrl Pts',(-41.8015589106221,37.2759624880186,38.1441444242173));
#28150=CARTESIAN_POINT('Ctrl Pts',(-41.8023850816305,37.2767574476534,38.1446719093431));
#28151=CARTESIAN_POINT('Ctrl Pts',(-41.803211252639,37.277552407288,38.145199394469));
#28152=CARTESIAN_POINT('Ctrl Pts',(-41.8040372167654,37.2783477324003,38.1457266528237));
#28153=CARTESIAN_POINT('Ctrl Pts',(-41.8048629737738,37.2791434227629,38.1462536842566));
#28154=CARTESIAN_POINT('Ctrl Pts',(-41.8056887307821,37.2799391131256,38.1467807156895));
#28155=CARTESIAN_POINT('Ctrl Pts',(-41.8065142806723,37.2807351687386,38.1473075202006));
#28156=CARTESIAN_POINT('Ctrl Pts',(-41.8073396232085,37.2815315893745,38.1478340976393));
#28157=CARTESIAN_POINT('Ctrl Pts',(-41.8081649657447,37.2823280100104,38.1483606750781));
#28158=CARTESIAN_POINT('Ctrl Pts',(-41.8089901009269,37.2831247956691,38.1488870254446));
#28159=CARTESIAN_POINT('Ctrl Pts',(-41.8098150285194,37.2839219461231,38.1494131485883));
#28160=CARTESIAN_POINT('Ctrl Pts',(-41.8106399561118,37.2847190965771,38.1499392717321));
#28161=CARTESIAN_POINT('Ctrl Pts',(-41.8114646761145,37.2855166118263,38.1504651676531));
#28162=CARTESIAN_POINT('Ctrl Pts',(-41.8122891882918,37.2863144916429,38.1509908362012));
#28163=CARTESIAN_POINT('Ctrl Pts',(-41.813113700469,37.2871123714595,38.1515165047493));
#28164=CARTESIAN_POINT('Ctrl Pts',(-41.8139380048207,37.2879106158435,38.1520419459243));
#28165=CARTESIAN_POINT('Ctrl Pts',(-41.8147621011115,37.2887092245666,38.1525671595763));
#28166=CARTESIAN_POINT('Ctrl Pts',(-41.8155861974023,37.2895078332898,38.1530923732283));
#28167=CARTESIAN_POINT('Ctrl Pts',(-41.8164100856322,37.2903068063522,38.1536173593573));
#28168=CARTESIAN_POINT('Ctrl Pts',(-41.8172337655656,37.2911061435257,38.154142117813));
#28169=CARTESIAN_POINT('Ctrl Pts',(-41.818057445499,37.2919054806991,38.1546668762689));
#28170=CARTESIAN_POINT('Ctrl Pts',(-41.818880917136,37.2927051819835,38.1551914070515));
#28171=CARTESIAN_POINT('Ctrl Pts',(-41.8197041802412,37.2935052471505,38.1557157100112));
#28172=CARTESIAN_POINT('Ctrl Pts',(-41.8205274433465,37.2943053123173,38.156240012971));
#28173=CARTESIAN_POINT('Ctrl Pts',(-41.82135049792,37.2951057413667,38.1567640881077));
#28174=CARTESIAN_POINT('Ctrl Pts',(-41.8221733437266,37.2959065340698,38.1572879352717));
#28175=CARTESIAN_POINT('Ctrl Pts',(-41.8229961895333,37.296707326773,38.1578117824357));
#28176=CARTESIAN_POINT('Ctrl Pts',(-41.823818826573,37.2975084831298,38.158335401627));
#28177=CARTESIAN_POINT('Ctrl Pts',(-41.8246412546107,37.2983100029116,38.158858792696));
#28178=CARTESIAN_POINT('Ctrl Pts',(-41.8254636826485,37.2991115226933,38.159382183765));
#28179=CARTESIAN_POINT('Ctrl Pts',(-41.8262859016842,37.2999134059,38.1599053467116));
#28180=CARTESIAN_POINT('Ctrl Pts',(-41.8271079114831,37.3007156523024,38.1604282813864));
#28181=CARTESIAN_POINT('Ctrl Pts',(-41.8279306518371,37.3015186116953,38.1609516808156));
#28182=CARTESIAN_POINT('Ctrl Pts',(-41.828753182582,37.3023219349298,38.1614748515671));
#28183=CARTESIAN_POINT('Ctrl Pts',(-41.8295755034826,37.303125621776,38.161997793491));
#28184=CARTESIAN_POINT('Ctrl Pts',(-41.7897141202235,37.2649171918739,38.1370740081602));
#28185=CARTESIAN_POINT('Ctrl Pts',(-41.7905699938216,37.2657354284759,38.1376222923523));
#28186=CARTESIAN_POINT('Ctrl Pts',(-41.7914256475163,37.2665540570026,38.1381703349224));
#28187=CARTESIAN_POINT('Ctrl Pts',(-41.7922810810461,37.267373077204,38.1387181357031));
#28188=CARTESIAN_POINT('Ctrl Pts',(-41.7931365145759,37.2681920974053,38.1392659364838));
#28189=CARTESIAN_POINT('Ctrl Pts',(-41.7939917279408,37.2690115092812,38.139813495475));
#28190=CARTESIAN_POINT('Ctrl Pts',(-41.7948467208796,37.2698313125814,38.1403608125096));
#28191=CARTESIAN_POINT('Ctrl Pts',(-41.7957017138184,37.2706511158816,38.1409081295443));
#28192=CARTESIAN_POINT('Ctrl Pts',(-41.7965564863311,37.271471310606,38.1414552046223));
#28193=CARTESIAN_POINT('Ctrl Pts',(-41.7974110381565,37.2722918965043,38.1420020375765));
#28194=CARTESIAN_POINT('Ctrl Pts',(-41.798265589982,37.2731124824025,38.1425488705307));
#28195=CARTESIAN_POINT('Ctrl Pts',(-41.7991199211203,37.2739334594745,38.1430954613612));
#28196=CARTESIAN_POINT('Ctrl Pts',(-41.7999740313103,37.2747548274695,38.143641809901));
#28197=CARTESIAN_POINT('Ctrl Pts',(-41.8008281415004,37.2755761954645,38.1441881584408));
#28198=CARTESIAN_POINT('Ctrl Pts',(-41.8016820307423,37.2763979543824,38.14473426469));
#28199=CARTESIAN_POINT('Ctrl Pts',(-41.8025356987751,37.2772201039724,38.1452801284816));
#28200=CARTESIAN_POINT('Ctrl Pts',(-41.803389366808,37.2780422535623,38.1458259922732));
#28201=CARTESIAN_POINT('Ctrl Pts',(-41.8042428136318,37.2788647938243,38.1463716136074));
#28202=CARTESIAN_POINT('Ctrl Pts',(-41.8050960389859,37.279687724507,38.1469169923174));
#28203=CARTESIAN_POINT('Ctrl Pts',(-41.80594926434,37.2805106551896,38.1474623710274));
#28204=CARTESIAN_POINT('Ctrl Pts',(-41.8068022682244,37.2813339762931,38.1480075071133));
#28205=CARTESIAN_POINT('Ctrl Pts',(-41.8076550503785,37.2821576875657,38.1485524004085));
#28206=CARTESIAN_POINT('Ctrl Pts',(-41.8085078325325,37.2829813988384,38.1490972937037));
#28207=CARTESIAN_POINT('Ctrl Pts',(-41.8093603929563,37.2838055002803,38.1496419442083));
#28208=CARTESIAN_POINT('Ctrl Pts',(-41.8102127313893,37.2846299916398,38.1501863517559));
#28209=CARTESIAN_POINT('Ctrl Pts',(-41.8110650698224,37.2854544829992,38.1507307593035));
#28210=CARTESIAN_POINT('Ctrl Pts',(-41.8119171862648,37.2862793642763,38.151274923894));
#28211=CARTESIAN_POINT('Ctrl Pts',(-41.8127690804561,37.2871046352189,38.1518188453614));
#28212=CARTESIAN_POINT('Ctrl Pts',(-41.8136209746473,37.2879299061615,38.1523627668288));
#28213=CARTESIAN_POINT('Ctrl Pts',(-41.8144726465877,37.2887555667696,38.1529064451729));
#28214=CARTESIAN_POINT('Ctrl Pts',(-41.8153240960168,37.2895816167912,38.1534498802278));
#28215=CARTESIAN_POINT('Ctrl Pts',(-41.8161755454458,37.2904076668127,38.1539933152827));
#28216=CARTESIAN_POINT('Ctrl Pts',(-41.8170267723638,37.2912341062476,38.1545365070483));
#28217=CARTESIAN_POINT('Ctrl Pts',(-41.8178777765105,37.2920609348435,38.1550794553588));
#28218=CARTESIAN_POINT('Ctrl Pts',(-41.8187287806572,37.2928877634394,38.1556224036692));
#28219=CARTESIAN_POINT('Ctrl Pts',(-41.8195795620327,37.2937149811963,38.1561651085245));
#28220=CARTESIAN_POINT('Ctrl Pts',(-41.8204301203771,37.2945425878614,38.1567075697588));
#28221=CARTESIAN_POINT('Ctrl Pts',(-41.8212806787215,37.2953701945265,38.1572500309931));
#28222=CARTESIAN_POINT('Ctrl Pts',(-41.8221310140348,37.2961981901,38.1577922486064));
#28223=CARTESIAN_POINT('Ctrl Pts',(-41.8229811260573,37.2970265743287,38.1583342224332));
#28224=CARTESIAN_POINT('Ctrl Pts',(-41.8238312380797,37.2978549585575,38.1588761962601));
#28225=CARTESIAN_POINT('Ctrl Pts',(-41.8246811268113,37.2986837314417,38.1594179263003));
#28226=CARTESIAN_POINT('Ctrl Pts',(-41.8255307919925,37.299512892728,38.1599594123885));
#28227=CARTESIAN_POINT('Ctrl Pts',(-41.8263804571736,37.3003420540145,38.1605008984767));
#28228=CARTESIAN_POINT('Ctrl Pts',(-41.8272298988042,37.3011716037031,38.1610421406129));
#28229=CARTESIAN_POINT('Ctrl Pts',(-41.8280791166249,37.3020015415406,38.1615831386317));
#28230=CARTESIAN_POINT('Ctrl Pts',(-41.8289290891818,37.3028322169792,38.1621246174586));
#28231=CARTESIAN_POINT('Ctrl Pts',(-41.8297788375306,37.303663281257,38.162665851734));
#28232=CARTESIAN_POINT('Ctrl Pts',(-41.8306283614115,37.3044947341195,38.1632068412924));
#28233=CARTESIAN_POINT('Ctrl Pts',(-41.7894511722233,37.2649739597797,38.137405330706));
#28234=CARTESIAN_POINT('Ctrl Pts',(-41.7903347721088,37.2658192665273,38.1379722901388));
#28235=CARTESIAN_POINT('Ctrl Pts',(-41.7912181371005,37.2666649919163,38.1385389914788));
#28236=CARTESIAN_POINT('Ctrl Pts',(-41.7921012669095,37.2675111356698,38.1391054345407));
#28237=CARTESIAN_POINT('Ctrl Pts',(-41.7929843967185,37.2683572794234,38.1396718776026));
#28238=CARTESIAN_POINT('Ctrl Pts',(-41.7938672913449,37.2692038415416,38.1402380623863));
#28239=CARTESIAN_POINT('Ctrl Pts',(-41.7947499504998,37.2700508217476,38.1408039887068));
#28240=CARTESIAN_POINT('Ctrl Pts',(-41.7956326096548,37.2708978019536,38.1413699150272));
#28241=CARTESIAN_POINT('Ctrl Pts',(-41.7965150333384,37.2717452002474,38.1419355828845));
#28242=CARTESIAN_POINT('Ctrl Pts',(-41.797397221262,37.2725930163519,38.1425009920934));
#28243=CARTESIAN_POINT('Ctrl Pts',(-41.7982794091856,37.2734408324565,38.1430664013023));
#28244=CARTESIAN_POINT('Ctrl Pts',(-41.7991613613493,37.2742890663717,38.1436315518629));
#28245=CARTESIAN_POINT('Ctrl Pts',(-41.8000430774646,37.2751377178202,38.1441964435905));
#28246=CARTESIAN_POINT('Ctrl Pts',(-41.8009247935799,37.2759863692687,38.1447613353181));
#28247=CARTESIAN_POINT('Ctrl Pts',(-41.8018062736468,37.2768354382506,38.1453259682126));
#28248=CARTESIAN_POINT('Ctrl Pts',(-41.8026875173771,37.2776849244881,38.1458903420894));
#28249=CARTESIAN_POINT('Ctrl Pts',(-41.8035687611075,37.2785344107256,38.1464547159662));
#28250=CARTESIAN_POINT('Ctrl Pts',(-41.8044497685012,37.2793843142188,38.1470188308252));
#28251=CARTESIAN_POINT('Ctrl Pts',(-41.8053305392701,37.2802346346897,38.1475826864821));
#28252=CARTESIAN_POINT('Ctrl Pts',(-41.8062113100392,37.2810849551606,38.148146542139));
#28253=CARTESIAN_POINT('Ctrl Pts',(-41.8070918441834,37.2819356926093,38.1487101385937));
#28254=CARTESIAN_POINT('Ctrl Pts',(-41.8079721414151,37.2827868467574,38.1492734756619));
#28255=CARTESIAN_POINT('Ctrl Pts',(-41.8088524386466,37.2836380009056,38.1498368127301));
#28256=CARTESIAN_POINT('Ctrl Pts',(-41.8097324989656,37.2844895717533,38.1503998904118));
#28257=CARTESIAN_POINT('Ctrl Pts',(-41.8106123220841,37.2853415590221,38.1509627085229));
#28258=CARTESIAN_POINT('Ctrl Pts',(-41.8114921452026,37.2861935462908,38.151525526634));
#28259=CARTESIAN_POINT('Ctrl Pts',(-41.8123717311206,37.2870459499806,38.1520880851745));
#28260=CARTESIAN_POINT('Ctrl Pts',(-41.8132510795506,37.2878987698127,38.1526503839604));
#28261=CARTESIAN_POINT('Ctrl Pts',(-41.8141304279805,37.2887515896449,38.1532126827462));
#28262=CARTESIAN_POINT('Ctrl Pts',(-41.8150095389224,37.2896048256193,38.1537747217775));
#28263=CARTESIAN_POINT('Ctrl Pts',(-41.8158884120887,37.2904584774571,38.1543365008704));
#28264=CARTESIAN_POINT('Ctrl Pts',(-41.816767285255,37.2913121292948,38.1548982799633));
#28265=CARTESIAN_POINT('Ctrl Pts',(-41.8176459206457,37.2921661969958,38.1554597991178));
#28266=CARTESIAN_POINT('Ctrl Pts',(-41.8185243179736,37.2930206802807,38.1560210581504));
#28267=CARTESIAN_POINT('Ctrl Pts',(-41.8194027153014,37.2938751635658,38.1565823171829));
#28268=CARTESIAN_POINT('Ctrl Pts',(-41.8202808745663,37.2947300624348,38.1571433160934));
#28269=CARTESIAN_POINT('Ctrl Pts',(-41.8211587954812,37.2955853766083,38.1577040546985));
#28270=CARTESIAN_POINT('Ctrl Pts',(-41.822036716396,37.2964406907818,38.1582647933035));
#28271=CARTESIAN_POINT('Ctrl Pts',(-41.8229143989609,37.2972964202596,38.1588252716031));
#28272=CARTESIAN_POINT('Ctrl Pts',(-41.8237918428886,37.2981525647621,38.1593854894139));
#28273=CARTESIAN_POINT('Ctrl Pts',(-41.8246692868163,37.2990087092646,38.1599457072248));
#28274=CARTESIAN_POINT('Ctrl Pts',(-41.825546492107,37.2998652687917,38.1605056645469));
#28275=CARTESIAN_POINT('Ctrl Pts',(-41.8264234584738,37.3007222430633,38.1610653611971));
#28276=CARTESIAN_POINT('Ctrl Pts',(-41.8273004248405,37.3015792173349,38.1616250578474));
#28277=CARTESIAN_POINT('Ctrl Pts',(-41.8281771522833,37.302436606351,38.1621844938258));
#28278=CARTESIAN_POINT('Ctrl Pts',(-41.8290536405155,37.3032944098312,38.1627436689494));
#28279=CARTESIAN_POINT('Ctrl Pts',(-41.8299309077201,37.304152975678,38.1633033410358));
#28280=CARTESIAN_POINT('Ctrl Pts',(-41.8308079352887,37.3050119567259,38.1638627518035));
#28281=CARTESIAN_POINT('Ctrl Pts',(-41.831684722934,37.3058713526935,38.1644219010693));
#28282=CARTESIAN_POINT('Ctrl Pts',(-41.7891882242231,37.2650307276855,38.1377366532517));
#28283=CARTESIAN_POINT('Ctrl Pts',(-41.790099550396,37.2659031045788,38.1383222879253));
#28284=CARTESIAN_POINT('Ctrl Pts',(-41.7910106266847,37.2667759268299,38.1389076480353));
#28285=CARTESIAN_POINT('Ctrl Pts',(-41.7919214527729,37.2676491941357,38.1394927333783));
#28286=CARTESIAN_POINT('Ctrl Pts',(-41.7928322788612,37.2685224614414,38.1400778187214));
#28287=CARTESIAN_POINT('Ctrl Pts',(-41.793742854749,37.269396173802,38.1406626292976));
#28288=CARTESIAN_POINT('Ctrl Pts',(-41.7946531801201,37.2702703309138,38.141247164904));
#28289=CARTESIAN_POINT('Ctrl Pts',(-41.7955635054912,37.2711444880256,38.1418317005103));
#28290=CARTESIAN_POINT('Ctrl Pts',(-41.7964735803457,37.2720190898887,38.1424159611466));
#28291=CARTESIAN_POINT('Ctrl Pts',(-41.7973834043674,37.2728941361996,38.1429999466102));
#28292=CARTESIAN_POINT('Ctrl Pts',(-41.7982932283892,37.2737691825104,38.1435839320738));
#28293=CARTESIAN_POINT('Ctrl Pts',(-41.7992028015783,37.2746446732689,38.1441676423646));
#28294=CARTESIAN_POINT('Ctrl Pts',(-41.8001121236188,37.2755206081709,38.14475107728));
#28295=CARTESIAN_POINT('Ctrl Pts',(-41.8010214456594,37.276396543073,38.1453345121953));
#28296=CARTESIAN_POINT('Ctrl Pts',(-41.8019305165514,37.2772729221187,38.1459176717352));
#28297=CARTESIAN_POINT('Ctrl Pts',(-41.8028393359792,37.2781497450038,38.1465005556972));
#28298=CARTESIAN_POINT('Ctrl Pts',(-41.803748155407,37.2790265678889,38.1470834396591));
#28299=CARTESIAN_POINT('Ctrl Pts',(-41.8046567233705,37.2799038346134,38.1476660480431));
#28300=CARTESIAN_POINT('Ctrl Pts',(-41.8055650395544,37.2807815448725,38.1482483806468));
#28301=CARTESIAN_POINT('Ctrl Pts',(-41.8064733557383,37.2816592551316,38.1488307132506));
#28302=CARTESIAN_POINT('Ctrl Pts',(-41.8073814201425,37.2825374089255,38.1494127700742));
#28303=CARTESIAN_POINT('Ctrl Pts',(-41.8082892324516,37.2834160059491,38.1499945509153));
#28304=CARTESIAN_POINT('Ctrl Pts',(-41.8091970447608,37.2842946029728,38.1505763317565));
#28305=CARTESIAN_POINT('Ctrl Pts',(-41.8101046049749,37.2851736432263,38.1511578366154));
#28306=CARTESIAN_POINT('Ctrl Pts',(-41.8110119127788,37.2860531264044,38.1517390652899));
#28307=CARTESIAN_POINT('Ctrl Pts',(-41.8119192205827,37.2869326095824,38.1523202939646));
#28308=CARTESIAN_POINT('Ctrl Pts',(-41.8128262759765,37.287812535685,38.1529012464549));
#28309=CARTESIAN_POINT('Ctrl Pts',(-41.8137330786451,37.2886929044066,38.1534819225593));
#28310=CARTESIAN_POINT('Ctrl Pts',(-41.8146398813137,37.2895732731283,38.1540625986637));
#28311=CARTESIAN_POINT('Ctrl Pts',(-41.8155464312571,37.290454084469,38.1546429983821));
#28312=CARTESIAN_POINT('Ctrl Pts',(-41.8164527281606,37.2913353381229,38.155223121513));
#28313=CARTESIAN_POINT('Ctrl Pts',(-41.8173590250641,37.2922165917768,38.1558032446439));
#28314=CARTESIAN_POINT('Ctrl Pts',(-41.8182650689276,37.2930982877439,38.1563830911873));
#28315=CARTESIAN_POINT('Ctrl Pts',(-41.8191708594366,37.293980425718,38.156962660942));
#28316=CARTESIAN_POINT('Ctrl Pts',(-41.8200766499455,37.2948625636922,38.1575422306965));
#28317=CARTESIAN_POINT('Ctrl Pts',(-41.8209821870999,37.2957451436734,38.1581215236623));
#28318=CARTESIAN_POINT('Ctrl Pts',(-41.8218874705853,37.2966281653551,38.1587005396381));
#28319=CARTESIAN_POINT('Ctrl Pts',(-41.8227927540706,37.2975111870369,38.1592795556139));
#28320=CARTESIAN_POINT('Ctrl Pts',(-41.8236977838869,37.2983946504193,38.1598582945997));
#28321=CARTESIAN_POINT('Ctrl Pts',(-41.82460255972,37.2992785551955,38.1604367563946));
#28322=CARTESIAN_POINT('Ctrl Pts',(-41.825507335553,37.3001624599717,38.1610152181895));
#28323=CARTESIAN_POINT('Ctrl Pts',(-41.8264118574027,37.3010468061417,38.1615934027935));
#28324=CARTESIAN_POINT('Ctrl Pts',(-41.827316124955,37.3019315933985,38.1621713100058));
#28325=CARTESIAN_POINT('Ctrl Pts',(-41.8282203925074,37.3028163806553,38.1627492172181));
#28326=CARTESIAN_POINT('Ctrl Pts',(-41.8291244057623,37.3037016089989,38.1633268470387));
#28327=CARTESIAN_POINT('Ctrl Pts',(-41.8300281644059,37.3045872781219,38.163904199267));
#28328=CARTESIAN_POINT('Ctrl Pts',(-41.8309327262584,37.3054737343768,38.1644820646129));
#28329=CARTESIAN_POINT('Ctrl Pts',(-41.8318370330468,37.3063606321949,38.1650596518729));
#28330=CARTESIAN_POINT('Ctrl Pts',(-41.8327410844565,37.3072479712676,38.1656369608462));
#28331=CARTESIAN_POINT('Ctrl Pts',(-41.7889155657315,37.2650855879526,38.1380738607379));
#28332=CARTESIAN_POINT('Ctrl Pts',(-41.7898542793006,37.2659844101691,38.1386774653796));
#28333=CARTESIAN_POINT('Ctrl Pts',(-41.7907927276113,37.2668837051443,38.1392807785649));
#28334=CARTESIAN_POINT('Ctrl Pts',(-41.7917309103178,37.2677834725466,38.1398838000717));
#28335=CARTESIAN_POINT('Ctrl Pts',(-41.7926690930243,37.2686832399489,38.1404868215784));
#28336=CARTESIAN_POINT('Ctrl Pts',(-41.7936070101265,37.2695834797784,38.1410895514065));
#28337=CARTESIAN_POINT('Ctrl Pts',(-41.7945446612787,37.2704841917031,38.1416919893337));
#28338=CARTESIAN_POINT('Ctrl Pts',(-41.795482312431,37.2713849036278,38.1422944272611));
#28339=CARTESIAN_POINT('Ctrl Pts',(-41.7964196976332,37.2722860876479,38.1428965732875));
#28340=CARTESIAN_POINT('Ctrl Pts',(-41.7973568165398,37.273187743431,38.1434984271912));
#28341=CARTESIAN_POINT('Ctrl Pts',(-41.7982939354465,37.2740893992142,38.1441002810949));
#28342=CARTESIAN_POINT('Ctrl Pts',(-41.7992307880576,37.2749915267605,38.1447018428759));
#28343=CARTESIAN_POINT('Ctrl Pts',(-41.8001673740279,37.2758941257373,38.1453031123123));
#28344=CARTESIAN_POINT('Ctrl Pts',(-41.8011039599982,37.2767967247142,38.1459043817488));
#28345=CARTESIAN_POINT('Ctrl Pts',(-41.8020402793276,37.2776997951217,38.1465053588408));
#28346=CARTESIAN_POINT('Ctrl Pts',(-41.8029763316709,37.2786033366268,38.1471060433667));
#28347=CARTESIAN_POINT('Ctrl Pts',(-41.8039123840142,37.2795068781321,38.1477067278927));
#28348=CARTESIAN_POINT('Ctrl Pts',(-41.8048481693716,37.2804108907349,38.1483071198526));
#28349=CARTESIAN_POINT('Ctrl Pts',(-41.8057836873979,37.2813153741023,38.1489072190253));
#28350=CARTESIAN_POINT('Ctrl Pts',(-41.8067192054243,37.2822198574697,38.1495073181979));
#28351=CARTESIAN_POINT('Ctrl Pts',(-41.8076544561196,37.2831248116015,38.1501071245833));
#28352=CARTESIAN_POINT('Ctrl Pts',(-41.8085894391392,37.2840302361643,38.1507066379602));
#28353=CARTESIAN_POINT('Ctrl Pts',(-41.8095244221589,37.2849356607271,38.1513061513371));
#28354=CARTESIAN_POINT('Ctrl Pts',(-41.8104591375028,37.2858415557209,38.1519053717056));
#28355=CARTESIAN_POINT('Ctrl Pts',(-41.8113935848264,37.2867479208116,38.1525042988449));
#28356=CARTESIAN_POINT('Ctrl Pts',(-41.81232803215,37.2876542859023,38.1531032259841));
#28357=CARTESIAN_POINT('Ctrl Pts',(-41.8132622114533,37.28856112109,38.1537018598942));
#28358=CARTESIAN_POINT('Ctrl Pts',(-41.814196122392,37.2894684260405,38.1543002003542));
#28359=CARTESIAN_POINT('Ctrl Pts',(-41.8151300333306,37.290375730991,38.1548985408142));
#28360=CARTESIAN_POINT('Ctrl Pts',(-41.8160636759047,37.2912835057042,38.1554965878244));
#28361=CARTESIAN_POINT('Ctrl Pts',(-41.8169970497698,37.2921917498456,38.1560943411641));
#28362=CARTESIAN_POINT('Ctrl Pts',(-41.8179304236351,37.2930999939869,38.1566920945039));
#28363=CARTESIAN_POINT('Ctrl Pts',(-41.8188635287915,37.2940087075564,38.1572895541733));
#28364=CARTESIAN_POINT('Ctrl Pts',(-41.8197963648951,37.2949178902191,38.1578867199521));
#28365=CARTESIAN_POINT('Ctrl Pts',(-41.8207292009987,37.2958270728817,38.1584838857309));
#28366=CARTESIAN_POINT('Ctrl Pts',(-41.8216617680496,37.2967367246376,38.1590807576191));
#28367=CARTESIAN_POINT('Ctrl Pts',(-41.8225940657039,37.2976468451513,38.1596773353967));
#28368=CARTESIAN_POINT('Ctrl Pts',(-41.8235263633582,37.2985569656651,38.1602739131743));
#28369=CARTESIAN_POINT('Ctrl Pts',(-41.824458391616,37.2994675549367,38.1608701968413));
#28370=CARTESIAN_POINT('Ctrl Pts',(-41.8253901501336,37.3003786126306,38.161466186178));
#28371=CARTESIAN_POINT('Ctrl Pts',(-41.8263219086513,37.3012896703245,38.1620621755146));
#28372=CARTESIAN_POINT('Ctrl Pts',(-41.8272533974288,37.3022011964406,38.1626578705208));
#28373=CARTESIAN_POINT('Ctrl Pts',(-41.8281846161229,37.303113190643,38.163253270977));
#28374=CARTESIAN_POINT('Ctrl Pts',(-41.829115834817,37.3040251848454,38.1638486714333));
#28375=CARTESIAN_POINT('Ctrl Pts',(-41.8300467834275,37.304937647134,38.1644437773396));
#28376=CARTESIAN_POINT('Ctrl Pts',(-41.8309774616115,37.3058505771725,38.1650385884766));
#28377=CARTESIAN_POINT('Ctrl Pts',(-41.8319089669289,37.306764318571,38.1656339282475));
#28378=CARTESIAN_POINT('Ctrl Pts',(-41.8328402013387,37.3076785285511,38.166228972725));
#28379=CARTESIAN_POINT('Ctrl Pts',(-41.833771164497,37.3085932067754,38.1668237216893));
#28380=CARTESIAN_POINT('Ctrl Pts',(-41.7886472049959,37.2651411028535,38.1384081478369));
#28381=CARTESIAN_POINT('Ctrl Pts',(-41.7896135096978,37.266066754582,38.1390301604039));
#28382=CARTESIAN_POINT('Ctrl Pts',(-41.7905795328642,37.2669929080792,38.1396518636297));
#28383=CARTESIAN_POINT('Ctrl Pts',(-41.7915452741163,37.2679195629823,38.1402732572709));
#28384=CARTESIAN_POINT('Ctrl Pts',(-41.7925110153685,37.2688462178852,38.1408946509121));
#28385=CARTESIAN_POINT('Ctrl Pts',(-41.7934764747066,37.269773374194,38.1415157349685));
#28386=CARTESIAN_POINT('Ctrl Pts',(-41.7944416517521,37.2707010315451,38.1421365091968));
#28387=CARTESIAN_POINT('Ctrl Pts',(-41.7954068287976,37.2716286888962,38.1427572834251));
#28388=CARTESIAN_POINT('Ctrl Pts',(-41.7963717235505,37.2725568472897,38.1433777478252));
#28389=CARTESIAN_POINT('Ctrl Pts',(-41.7973363356327,37.2734855063617,38.143997902154));
#28390=CARTESIAN_POINT('Ctrl Pts',(-41.7983009477148,37.2744141654338,38.1446180564827));
#28391=CARTESIAN_POINT('Ctrl Pts',(-41.7992652771263,37.2753433251844,38.1452379007402));
#28392=CARTESIAN_POINT('Ctrl Pts',(-41.800229323489,37.2762729852495,38.1458574346833));
#28393=CARTESIAN_POINT('Ctrl Pts',(-41.8011933698517,37.2772026453146,38.1464769686264));
#28394=CARTESIAN_POINT('Ctrl Pts',(-41.8021571331657,37.278132805694,38.1470961922553));
#28395=CARTESIAN_POINT('Ctrl Pts',(-41.8031206130533,37.2790634660233,38.1477151053271));
#28396=CARTESIAN_POINT('Ctrl Pts',(-41.8040840929409,37.2799941263525,38.148334018399));
#28397=CARTESIAN_POINT('Ctrl Pts',(-41.805047289402,37.2809252866316,38.1489526209138));
#28398=CARTESIAN_POINT('Ctrl Pts',(-41.8060102020591,37.2818569464955,38.1495709126293));
#28399=CARTESIAN_POINT('Ctrl Pts',(-41.8069731147162,37.2827886063595,38.1501892043446));
#28400=CARTESIAN_POINT('Ctrl Pts',(-41.8079357435694,37.2837207658083,38.1508071852606));
#28401=CARTESIAN_POINT('Ctrl Pts',(-41.8088980882413,37.2846534244766,38.1514248551349));
#28402=CARTESIAN_POINT('Ctrl Pts',(-41.8098604329132,37.2855860831449,38.1520425250092));
#28403=CARTESIAN_POINT('Ctrl Pts',(-41.8108224934038,37.2865192410328,38.1526598838418));
#28404=CARTESIAN_POINT('Ctrl Pts',(-41.8117842693361,37.2874528977743,38.1532769313908));
#28405=CARTESIAN_POINT('Ctrl Pts',(-41.8127460452683,37.2883865545159,38.1538939789397));
#28406=CARTESIAN_POINT('Ctrl Pts',(-41.8137075366422,37.2893207101113,38.1545107152051));
#28407=CARTESIAN_POINT('Ctrl Pts',(-41.814668743081,37.2902553641942,38.1551271399451));
#28408=CARTESIAN_POINT('Ctrl Pts',(-41.8156299495197,37.2911900182772,38.155743564685));
#28409=CARTESIAN_POINT('Ctrl Pts',(-41.8165908710233,37.2921251708477,38.1563596778997));
#28410=CARTESIAN_POINT('Ctrl Pts',(-41.8175515072149,37.2930608215395,38.1569754793474));
#28411=CARTESIAN_POINT('Ctrl Pts',(-41.8185121434066,37.2939964722311,38.1575912807952));
#28412=CARTESIAN_POINT('Ctrl Pts',(-41.8194724942865,37.2949326210439,38.1582067704761));
#28413=CARTESIAN_POINT('Ctrl Pts',(-41.8204325594782,37.2958692676108,38.158821948149));
#28414=CARTESIAN_POINT('Ctrl Pts',(-41.8213926246698,37.2968059141777,38.1594371258218));
#28415=CARTESIAN_POINT('Ctrl Pts',(-41.8223524041732,37.2977430584989,38.1600519914865));
#28416=CARTESIAN_POINT('Ctrl Pts',(-41.8233118976122,37.2986807002069,38.1606665449022));
#28417=CARTESIAN_POINT('Ctrl Pts',(-41.8242713910512,37.2996183419148,38.1612810983179));
#28418=CARTESIAN_POINT('Ctrl Pts',(-41.8252305984258,37.3005564810097,38.1618953394845));
#28419=CARTESIAN_POINT('Ctrl Pts',(-41.82618951936,37.3014951171236,38.1625092681612));
#28420=CARTESIAN_POINT('Ctrl Pts',(-41.8271484402942,37.3024337532377,38.163123196838));
#28421=CARTESIAN_POINT('Ctrl Pts',(-41.828107074788,37.3033728863708,38.1637368130249));
#28422=CARTESIAN_POINT('Ctrl Pts',(-41.8290654224657,37.3043125161551,38.1643501164815));
#28423=CARTESIAN_POINT('Ctrl Pts',(-41.8300237701435,37.3052521459393,38.1649634199381));
#28424=CARTESIAN_POINT('Ctrl Pts',(-41.8309818310051,37.3061922723746,38.1655764106644));
#28425=CARTESIAN_POINT('Ctrl Pts',(-41.8319396046751,37.3071328950925,38.1661890884201));
#28426=CARTESIAN_POINT('Ctrl Pts',(-41.8328982295595,37.3080743537819,38.1668023106886));
#28427=CARTESIAN_POINT('Ctrl Pts',(-41.8338565667415,37.3090163096364,38.16741521943));
#28428=CARTESIAN_POINT('Ctrl Pts',(-41.8348146158448,37.3099587622863,38.1680278144036));
#28429=CARTESIAN_POINT('Ctrl Pts',(-41.7875737620538,37.2653631624573,38.1397452962328));
#28430=CARTESIAN_POINT('Ctrl Pts',(-41.7886504312868,37.2663961322335,38.140440940501));
#28431=CARTESIAN_POINT('Ctrl Pts',(-41.7897267538755,37.267429719819,38.1411362038889));
#28432=CARTESIAN_POINT('Ctrl Pts',(-41.7908027293106,37.2684639247247,38.1418310860678));
#28433=CARTESIAN_POINT('Ctrl Pts',(-41.7918787047456,37.2694981296305,38.1425259682467));
#28434=CARTESIAN_POINT('Ctrl Pts',(-41.7929543330269,37.2705329518566,38.1432204692165));
#28435=CARTESIAN_POINT('Ctrl Pts',(-41.7940296136454,37.2715683909132,38.1439145886488));
#28436=CARTESIAN_POINT('Ctrl Pts',(-41.795104894264,37.2726038299698,38.1446087080811));
#28437=CARTESIAN_POINT('Ctrl Pts',(-41.7961798272198,37.2736398858571,38.1453024459759));
#28438=CARTESIAN_POINT('Ctrl Pts',(-41.7972544120039,37.2746765580847,38.1459958020049));
#28439=CARTESIAN_POINT('Ctrl Pts',(-41.7983289967881,37.2757132303124,38.1466891580339));
#28440=CARTESIAN_POINT('Ctrl Pts',(-41.7994032334007,37.2767505188804,38.1473821321973));
#28441=CARTESIAN_POINT('Ctrl Pts',(-41.8004771213333,37.2777884232982,38.1480747241671));
#28442=CARTESIAN_POINT('Ctrl Pts',(-41.8015510092659,37.2788263277159,38.1487673161369));
#28443=CARTESIAN_POINT('Ctrl Pts',(-41.8026245485185,37.2798648479832,38.1494595259133));
#28444=CARTESIAN_POINT('Ctrl Pts',(-41.8036977385828,37.2809039836088,38.1501513531687));
#28445=CARTESIAN_POINT('Ctrl Pts',(-41.8047709286472,37.2819431192344,38.1508431804241));
#28446=CARTESIAN_POINT('Ctrl Pts',(-41.8058437695235,37.2829828702182,38.1515346251586));
#28447=CARTESIAN_POINT('Ctrl Pts',(-41.8069162607038,37.2840232360685,38.152225687045));
#28448=CARTESIAN_POINT('Ctrl Pts',(-41.8079887518841,37.2850636019188,38.1529167489315));
#28449=CARTESIAN_POINT('Ctrl Pts',(-41.8090608933685,37.2861045826353,38.15360742797));
#28450=CARTESIAN_POINT('Ctrl Pts',(-41.8101326846494,37.2871461777257,38.1542977238337));
#28451=CARTESIAN_POINT('Ctrl Pts',(-41.8112044759304,37.2881877728161,38.1549880196974));
#28452=CARTESIAN_POINT('Ctrl Pts',(-41.8122759170079,37.2892299822803,38.1556779323864));
#28453=CARTESIAN_POINT('Ctrl Pts',(-41.8133470073749,37.2902728056253,38.1563674615743));
#28454=CARTESIAN_POINT('Ctrl Pts',(-41.8144180977418,37.2913156289704,38.1570569907622));
#28455=CARTESIAN_POINT('Ctrl Pts',(-41.8154888373982,37.2923590661962,38.157746136449));
#28456=CARTESIAN_POINT('Ctrl Pts',(-41.8165592258371,37.2934031168091,38.1584348983086));
#28457=CARTESIAN_POINT('Ctrl Pts',(-41.8176296142761,37.294447167422,38.1591236601683));
#28458=CARTESIAN_POINT('Ctrl Pts',(-41.8186996514976,37.2954918314221,38.1598120382009));
#28459=CARTESIAN_POINT('Ctrl Pts',(-41.8197693369953,37.296537108315,38.1605000320806));
#28460=CARTESIAN_POINT('Ctrl Pts',(-41.8208390224929,37.297582385208,38.1611880259604));
#28461=CARTESIAN_POINT('Ctrl Pts',(-41.8219083562667,37.2986282749938,38.1618756356875));
#28462=CARTESIAN_POINT('Ctrl Pts',(-41.8229773378104,37.2996747771778,38.1625628609364));
#28463=CARTESIAN_POINT('Ctrl Pts',(-41.8240463193541,37.3007212793618,38.1632500861854));
#28464=CARTESIAN_POINT('Ctrl Pts',(-41.8251149486677,37.3017683939439,38.1639369269563));
#28465=CARTESIAN_POINT('Ctrl Pts',(-41.8261832252455,37.3028161204288,38.1646233829242));
#28466=CARTESIAN_POINT('Ctrl Pts',(-41.8272515018232,37.3038638469136,38.1653098388921));
#28467=CARTESIAN_POINT('Ctrl Pts',(-41.828319425665,37.3049121853013,38.165995910057));
#28468=CARTESIAN_POINT('Ctrl Pts',(-41.8293869962654,37.3059611350958,38.1666815960944));
#28469=CARTESIAN_POINT('Ctrl Pts',(-41.8304545668658,37.3070100848902,38.1673672821317));
#28470=CARTESIAN_POINT('Ctrl Pts',(-41.8315217842248,37.3080596460915,38.1680525830415));
#28471=CARTESIAN_POINT('Ctrl Pts',(-41.8325886478371,37.3091098182032,38.1687374984995));
#28472=CARTESIAN_POINT('Ctrl Pts',(-41.8336555114495,37.3101599903149,38.1694224139574));
#28473=CARTESIAN_POINT('Ctrl Pts',(-41.8347220213153,37.3112107733369,38.1701069439635));
#28474=CARTESIAN_POINT('Ctrl Pts',(-41.8357881769296,37.3122621667721,38.1707910881941));
#28475=CARTESIAN_POINT('Ctrl Pts',(-41.8368552800818,37.3133144946256,38.1714758404528));
#28476=CARTESIAN_POINT('Ctrl Pts',(-41.8379220283527,37.3143674339778,38.1721602062498));
#28477=CARTESIAN_POINT('Ctrl Pts',(-41.8389884212363,37.3154209843298,38.1728441852607));
#28478=CARTESIAN_POINT('Ctrl Pts',(-41.7864981650237,37.2655827073535,38.1410803260952));
#28479=CARTESIAN_POINT('Ctrl Pts',(-41.7876857100844,37.2667240342716,38.1418508221963));
#28480=CARTESIAN_POINT('Ctrl Pts',(-41.7888728315231,37.2678661161931,38.1426208528369));
#28481=CARTESIAN_POINT('Ctrl Pts',(-41.7900595286536,37.269008952458,38.1433904175723));
#28482=CARTESIAN_POINT('Ctrl Pts',(-41.7912462257841,37.270151788723,38.1441599823077));
#28483=CARTESIAN_POINT('Ctrl Pts',(-41.7924324986064,37.2712953793314,38.144929081138));
#28484=CARTESIAN_POINT('Ctrl Pts',(-41.7936183464348,37.2724397236224,38.1456977136189));
#28485=CARTESIAN_POINT('Ctrl Pts',(-41.794804194263,37.2735840679135,38.1464663460999));
#28486=CARTESIAN_POINT('Ctrl Pts',(-41.7959896170973,37.2747291658873,38.1472345122315));
#28487=CARTESIAN_POINT('Ctrl Pts',(-41.7971746142523,37.2758750168822,38.1480022115702));
#28488=CARTESIAN_POINT('Ctrl Pts',(-41.7983596114072,37.2770208678771,38.1487699109088));
#28489=CARTESIAN_POINT('Ctrl Pts',(-41.7995441828828,37.2781674718931,38.1495371434545));
#28490=CARTESIAN_POINT('Ctrl Pts',(-41.8007283279944,37.2793148282676,38.1503039087642));
#28491=CARTESIAN_POINT('Ctrl Pts',(-41.8019124731059,37.2804621846422,38.1510706740739));
#28492=CARTESIAN_POINT('Ctrl Pts',(-41.8030961918533,37.2816102933754,38.1518369721475));
#28493=CARTESIAN_POINT('Ctrl Pts',(-41.8042794835522,37.2827591538039,38.1526028025426));
#28494=CARTESIAN_POINT('Ctrl Pts',(-41.8054627752511,37.2839080142324,38.1533686329376));
#28495=CARTESIAN_POINT('Ctrl Pts',(-41.8066456399015,37.2850576263563,38.154133995654));
#28496=CARTESIAN_POINT('Ctrl Pts',(-41.8078280768195,37.2862079895112,38.1548988902498));
#28497=CARTESIAN_POINT('Ctrl Pts',(-41.8090105137376,37.2873583526662,38.1556637848456));
#28498=CARTESIAN_POINT('Ctrl Pts',(-41.8101925229233,37.2885094668524,38.1564282113207));
#28499=CARTESIAN_POINT('Ctrl Pts',(-41.8113741036934,37.2896613314046,38.1571921692336));
#28500=CARTESIAN_POINT('Ctrl Pts',(-41.8125556844634,37.2908131959569,38.1579561271466));
#28501=CARTESIAN_POINT('Ctrl Pts',(-41.8137368368177,37.2919658108753,38.1587196164974));
#28502=CARTESIAN_POINT('Ctrl Pts',(-41.8149175600733,37.2931191754941,38.159482636845));
#28503=CARTESIAN_POINT('Ctrl Pts',(-41.816098283329,37.2942725401128,38.1602456571926));
#28504=CARTESIAN_POINT('Ctrl Pts',(-41.8172785774861,37.2954266544319,38.161008208537));
#28505=CARTESIAN_POINT('Ctrl Pts',(-41.8184584418621,37.2965815177845,38.1617702904379));
#28506=CARTESIAN_POINT('Ctrl Pts',(-41.8196383062381,37.2977363811371,38.1625323723387));
#28507=CARTESIAN_POINT('Ctrl Pts',(-41.8208177408331,37.2988919935233,38.1632939847959));
#28508=CARTESIAN_POINT('Ctrl Pts',(-41.8219967449651,37.3000483542757,38.1640551273696));
#28509=CARTESIAN_POINT('Ctrl Pts',(-41.8231757490971,37.301204715028,38.1648162699433));
#28510=CARTESIAN_POINT('Ctrl Pts',(-41.8243543227662,37.3023618241463,38.1655769426334));
#28511=CARTESIAN_POINT('Ctrl Pts',(-41.8255324652909,37.3035196809625,38.1663371450006));
#28512=CARTESIAN_POINT('Ctrl Pts',(-41.8267106078155,37.3046775377785,38.1670973473678));
#28513=CARTESIAN_POINT('Ctrl Pts',(-41.8278883191958,37.3058361422923,38.167857079412));
#28514=CARTESIAN_POINT('Ctrl Pts',(-41.8290655987506,37.3069954938345,38.1686163406944));
#28515=CARTESIAN_POINT('Ctrl Pts',(-41.8302428783055,37.3081548453767,38.1693756019768));
#28516=CARTESIAN_POINT('Ctrl Pts',(-41.831419726035,37.3093149439473,38.1701343924974));
#28517=CARTESIAN_POINT('Ctrl Pts',(-41.8325961412587,37.3104757888764,38.1708927118178));
#28518=CARTESIAN_POINT('Ctrl Pts',(-41.8337725564824,37.3116366338054,38.1716510311383));
#28519=CARTESIAN_POINT('Ctrl Pts',(-41.8349485392002,37.3127982250929,38.1724088792586));
#28520=CARTESIAN_POINT('Ctrl Pts',(-41.8361240887322,37.3139605620678,38.1731662557409));
#28521=CARTESIAN_POINT('Ctrl Pts',(-41.8372996382642,37.3151228990428,38.1739236322232));
#28522=CARTESIAN_POINT('Ctrl Pts',(-41.8384747546104,37.3162859817051,38.1746805370675));
#28523=CARTESIAN_POINT('Ctrl Pts',(-41.8396494370912,37.3174498093833,38.1754369698366));
#28524=CARTESIAN_POINT('Ctrl Pts',(-41.8408251635625,37.3186146714048,38.1761940748797));
#28525=CARTESIAN_POINT('Ctrl Pts',(-41.8420004553969,37.3197802797668,38.1769507070081));
#28526=CARTESIAN_POINT('Ctrl Pts',(-41.8431753119136,37.320946633795,38.1777068657839));
#28527=CARTESIAN_POINT('Ctrl Pts',(-41.785420431661,37.26579975827,38.1424132548863));
#28528=CARTESIAN_POINT('Ctrl Pts',(-41.786719321559,37.2670504478503,38.1432598069792));
#28529=CARTESIAN_POINT('Ctrl Pts',(-41.7880176984179,37.2683020517983,38.1441057953634));
#28530=CARTESIAN_POINT('Ctrl Pts',(-41.7893155613103,37.2695545692201,38.1449512194344));
#28531=CARTESIAN_POINT('Ctrl Pts',(-41.7906134242027,37.270807086642,38.1457966435054));
#28532=CARTESIAN_POINT('Ctrl Pts',(-41.7919107731286,37.2720605175377,38.1466415032634));
#28533=CARTESIAN_POINT('Ctrl Pts',(-41.7932076071614,37.2733148610119,38.1474857981048));
#28534=CARTESIAN_POINT('Ctrl Pts',(-41.7945044411943,37.2745692044862,38.1483300929463));
#28535=CARTESIAN_POINT('Ctrl Pts',(-41.795800760334,37.275824460539,38.1491738228712));
#28536=CARTESIAN_POINT('Ctrl Pts',(-41.7970965636547,37.2770806282739,38.150016987277));
#28537=CARTESIAN_POINT('Ctrl Pts',(-41.7983923669755,37.2783367960088,38.1508601516828));
#28538=CARTESIAN_POINT('Ctrl Pts',(-41.7996876544773,37.2795938754256,38.1517027505694));
#28539=CARTESIAN_POINT('Ctrl Pts',(-41.8009824252349,37.2808518656268,38.1525447833351));
#28540=CARTESIAN_POINT('Ctrl Pts',(-41.8022771959926,37.2821098558278,38.1533868161008));
#28541=CARTESIAN_POINT('Ctrl Pts',(-41.8035714500061,37.283368756813,38.1542282827456));
#28542=CARTESIAN_POINT('Ctrl Pts',(-41.8048651863511,37.2846285676834,38.1550691826683));
#28543=CARTESIAN_POINT('Ctrl Pts',(-41.8061589226961,37.2858883785537,38.1559100825911));
#28544=CARTESIAN_POINT('Ctrl Pts',(-41.8074521413726,37.287149099309,38.1567504157919));
#28545=CARTESIAN_POINT('Ctrl Pts',(-41.8087448414569,37.2884107290488,38.1575901816705));
#28546=CARTESIAN_POINT('Ctrl Pts',(-41.8100375415412,37.2896723587887,38.1584299475492));
#28547=CARTESIAN_POINT('Ctrl Pts',(-41.8113297230333,37.2909348975131,38.1592691461057));
#28548=CARTESIAN_POINT('Ctrl Pts',(-41.8126213850103,37.2921983443204,38.1601077767407));
#28549=CARTESIAN_POINT('Ctrl Pts',(-41.8139130469873,37.2934617911276,38.1609464073756));
#28550=CARTESIAN_POINT('Ctrl Pts',(-41.8152041894491,37.2947261460177,38.161784470089));
#28551=CARTESIAN_POINT('Ctrl Pts',(-41.8164948114736,37.2959914080875,38.1626219642823));
#28552=CARTESIAN_POINT('Ctrl Pts',(-41.8177854334982,37.2972566701574,38.1634594584755));
#28553=CARTESIAN_POINT('Ctrl Pts',(-41.8190755350855,37.298522839407,38.1642963841487));
#28554=CARTESIAN_POINT('Ctrl Pts',(-41.820365115314,37.299789914932,38.165132740704));
#28555=CARTESIAN_POINT('Ctrl Pts',(-41.8216546955425,37.301056990457,38.1659690972592));
#28556=CARTESIAN_POINT('Ctrl Pts',(-41.8229437544123,37.3023249722574,38.1668048846966));
#28557=CARTESIAN_POINT('Ctrl Pts',(-41.8242322910026,37.3035938594276,38.1676401024191));
#28558=CARTESIAN_POINT('Ctrl Pts',(-41.8255208275929,37.3048627465979,38.1684753201416));
#28559=CARTESIAN_POINT('Ctrl Pts',(-41.8268088419038,37.3061325391379,38.1693099681493));
#28560=CARTESIAN_POINT('Ctrl Pts',(-41.8280963330153,37.3074032361407,38.1701440458461));
#28561=CARTESIAN_POINT('Ctrl Pts',(-41.8293838241269,37.3086739331435,38.1709781235428));
#28562=CARTESIAN_POINT('Ctrl Pts',(-41.830670792039,37.3099455346092,38.1718116309285));
#28563=CARTESIAN_POINT('Ctrl Pts',(-41.8319572358326,37.3112180396295,38.172644567408));
#28564=CARTESIAN_POINT('Ctrl Pts',(-41.8332436796261,37.3124905446497,38.1734775038874));
#28565=CARTESIAN_POINT('Ctrl Pts',(-41.8345295993011,37.3137639532247,38.1743098694605));
#28566=CARTESIAN_POINT('Ctrl Pts',(-41.835814993939,37.3150382644446,38.1751416635329));
#28567=CARTESIAN_POINT('Ctrl Pts',(-41.8371003885769,37.3163125756647,38.1759734576052));
#28568=CARTESIAN_POINT('Ctrl Pts',(-41.8383852581778,37.3175877895298,38.1768046801767));
#28569=CARTESIAN_POINT('Ctrl Pts',(-41.8396696018239,37.3188639051292,38.1776353306538));
#28570=CARTESIAN_POINT('Ctrl Pts',(-41.8409539454701,37.3201400207286,38.1784659811308));
#28571=CARTESIAN_POINT('Ctrl Pts',(-41.8422377631615,37.3214170380623,38.1792960595133));
#28572=CARTESIAN_POINT('Ctrl Pts',(-41.8435210539812,37.3226949562182,38.1801255652085));
#28573=CARTESIAN_POINT('Ctrl Pts',(-41.8448054853162,37.3239740101144,38.1809558081207));
#28574=CARTESIAN_POINT('Ctrl Pts',(-41.8460893888426,37.3252539664348,38.1817854773272));
#28575=CARTESIAN_POINT('Ctrl Pts',(-41.8473727636417,37.3265348242634,38.1826145722343));
#28576=CARTESIAN_POINT('Ctrl Pts',(-41.7811094982102,37.2666679619361,38.1477449700507));
#28577=CARTESIAN_POINT('Ctrl Pts',(-41.7828537674574,37.2683561021649,38.1488957461111));
#28578=CARTESIAN_POINT('Ctrl Pts',(-41.7845971659969,37.2700457942191,38.1500455654693));
#28579=CARTESIAN_POINT('Ctrl Pts',(-41.7863396919368,37.2717370362685,38.1511944268828));
#28580=CARTESIAN_POINT('Ctrl Pts',(-41.7880822178768,37.273428278318,38.1523432882963));
#28581=CARTESIAN_POINT('Ctrl Pts',(-41.7898238712172,37.2751210703628,38.153491191765));
#28582=CARTESIAN_POINT('Ctrl Pts',(-41.7915646500682,37.2768154105697,38.1546381360485));
#28583=CARTESIAN_POINT('Ctrl Pts',(-41.7933054289192,37.2785097507767,38.1557850803319));
#28584=CARTESIAN_POINT('Ctrl Pts',(-41.7950453332808,37.2802056391457,38.1569310654301));
#28585=CARTESIAN_POINT('Ctrl Pts',(-41.7967843612647,37.2819030738406,38.1580760901044));
#28586=CARTESIAN_POINT('Ctrl Pts',(-41.7985233892487,37.2836005085354,38.1592211147786));
#28587=CARTESIAN_POINT('Ctrl Pts',(-41.8002615408549,37.2852994895561,38.160365179029));
#28588=CARTESIAN_POINT('Ctrl Pts',(-41.8019988141972,37.2870000150632,38.1615082816187));
#28589=CARTESIAN_POINT('Ctrl Pts',(-41.8037360875394,37.2887005405702,38.1626513842085));
#28590=CARTESIAN_POINT('Ctrl Pts',(-41.8054724826176,37.2904026105638,38.1637935251375));
#28591=CARTESIAN_POINT('Ctrl Pts',(-41.807207997547,37.2921062232011,38.1649347031713));
#28592=CARTESIAN_POINT('Ctrl Pts',(-41.8089435124765,37.2938098358385,38.1660758812051));
#28593=CARTESIAN_POINT('Ctrl Pts',(-41.8106781472572,37.2955149911197,38.1672160963434));
#28594=CARTESIAN_POINT('Ctrl Pts',(-41.8124119000063,37.2972216871992,38.1683553473536));
#28595=CARTESIAN_POINT('Ctrl Pts',(-41.8141456527554,37.2989283832786,38.1694945983638));
#28596=CARTESIAN_POINT('Ctrl Pts',(-41.8158785234729,37.3006366201563,38.1706328852458));
#28597=CARTESIAN_POINT('Ctrl Pts',(-41.8176105102778,37.3023463959835,38.1717702067688));
#28598=CARTESIAN_POINT('Ctrl Pts',(-41.8193424970826,37.3040561718106,38.1729075282917));
#28599=CARTESIAN_POINT('Ctrl Pts',(-41.8210735999748,37.3057674865872,38.1740438844557));
#28600=CARTESIAN_POINT('Ctrl Pts',(-41.8228038170748,37.3074803384615,38.1751792740315));
#28601=CARTESIAN_POINT('Ctrl Pts',(-41.824534034175,37.3091931903357,38.1763146636074));
#28602=CARTESIAN_POINT('Ctrl Pts',(-41.826263365483,37.3109075793076,38.1774490865953));
#28603=CARTESIAN_POINT('Ctrl Pts',(-41.8279918091215,37.3126235035221,38.1785825417683));
#28604=CARTESIAN_POINT('Ctrl Pts',(-41.82972025276,37.3143394277366,38.1797159969412));
#28605=CARTESIAN_POINT('Ctrl Pts',(-41.8314478087289,37.3160568871938,38.1808484842992));
#28606=CARTESIAN_POINT('Ctrl Pts',(-41.8331744751525,37.3177758800355,38.1819800026171));
#28607=CARTESIAN_POINT('Ctrl Pts',(-41.8349011415761,37.3194948728773,38.1831115209351));
#28608=CARTESIAN_POINT('Ctrl Pts',(-41.8366269184544,37.3212153991037,38.1842420702131));
#28609=CARTESIAN_POINT('Ctrl Pts',(-41.8383518039133,37.3229374568536,38.1853716492279));
#28610=CARTESIAN_POINT('Ctrl Pts',(-41.8400766893723,37.3246595146035,38.1865012282427));
#28611=CARTESIAN_POINT('Ctrl Pts',(-41.841800683412,37.326383103877,38.1876298369945));
#28612=CARTESIAN_POINT('Ctrl Pts',(-41.8435237841602,37.3281082228095,38.1887574742621));
#28613=CARTESIAN_POINT('Ctrl Pts',(-41.8452468849085,37.3298333417421,38.1898851115296));
#28614=CARTESIAN_POINT('Ctrl Pts',(-41.8469690923652,37.331559990334,38.1910117773129));
#28615=CARTESIAN_POINT('Ctrl Pts',(-41.8486904046602,37.3332881667178,38.1921374703929));
#28616=CARTESIAN_POINT('Ctrl Pts',(-41.8504117169551,37.3350163431016,38.1932631634728));
#28617=CARTESIAN_POINT('Ctrl Pts',(-41.8521321340882,37.3367460472773,38.1943878838494));
#28618=CARTESIAN_POINT('Ctrl Pts',(-41.8538516541909,37.3384772773746,38.1955116303053));
#28619=CARTESIAN_POINT('Ctrl Pts',(-41.8555711742936,37.3402085074719,38.1966353767613));
#28620=CARTESIAN_POINT('Ctrl Pts',(-41.8572897973659,37.3419412634907,38.1977581492966));
#28621=CARTESIAN_POINT('Ctrl Pts',(-41.859007521541,37.3436755435576,38.1988799466961));
#28622=CARTESIAN_POINT('Ctrl Pts',(-41.8607267723309,37.3454113649531,38.2000027410847));
#28623=CARTESIAN_POINT('Ctrl Pts',(-41.8624451226252,37.3471487131068,38.2011245586035));
#28624=CARTESIAN_POINT('Ctrl Pts',(-41.8641625705538,37.3488875861373,38.2022453980358));
#28625=CARTESIAN_POINT('Ctrl Pts',(-41.7767643079322,37.2674961737807,38.1530429938155));
#28626=CARTESIAN_POINT('Ctrl Pts',(-41.7789615970312,37.2696380573266,38.1545174677516));
#28627=CARTESIAN_POINT('Ctrl Pts',(-41.7811574577173,37.2717824866718,38.1559903721994));
#28628=CARTESIAN_POINT('Ctrl Pts',(-41.7833518861241,37.2739294580647,38.1574617046023));
#28629=CARTESIAN_POINT('Ctrl Pts',(-41.7855463145309,37.2760764294577,38.1589330370052));
#28630=CARTESIAN_POINT('Ctrl Pts',(-41.7877393106584,37.2782259428985,38.1604027973634));
#28631=CARTESIAN_POINT('Ctrl Pts',(-41.789930870644,37.2803779946286,38.1618709831246));
#28632=CARTESIAN_POINT('Ctrl Pts',(-41.7921224306297,37.2825300463587,38.1633391688858));
#28633=CARTESIAN_POINT('Ctrl Pts',(-41.7943125544735,37.2846846363782,38.1648057800501));
#28634=CARTESIAN_POINT('Ctrl Pts',(-41.796501238317,37.2868417609214,38.1662708140698));
#28635=CARTESIAN_POINT('Ctrl Pts',(-41.7986899221604,37.2889988854646,38.1677358480895));
#28636=CARTESIAN_POINT('Ctrl Pts',(-41.8008771660035,37.2911585445316,38.1691993049645));
#28637=CARTESIAN_POINT('Ctrl Pts',(-41.8030629659915,37.2933207343499,38.1706611821514));
#28638=CARTESIAN_POINT('Ctrl Pts',(-41.8052487659796,37.2954829241681,38.1721230593384));
#28639=CARTESIAN_POINT('Ctrl Pts',(-41.8074331221127,37.2976476447376,38.1735833568372));
#28640=CARTESIAN_POINT('Ctrl Pts',(-41.8096160305401,37.2998148922788,38.175042072109));
#28641=CARTESIAN_POINT('Ctrl Pts',(-41.8117989389676,37.3019821398199,38.1765007873808));
#28642=CARTESIAN_POINT('Ctrl Pts',(-41.8139803996895,37.3041519143327,38.1779579204255));
#28643=CARTESIAN_POINT('Ctrl Pts',(-41.8161604088591,37.3063242120306,38.1794134687084));
#28644=CARTESIAN_POINT('Ctrl Pts',(-41.8183404180287,37.3084965097284,38.1808690169913));
#28645=CARTESIAN_POINT('Ctrl Pts',(-41.820518975646,37.3106713306114,38.1823229805124));
#28646=CARTESIAN_POINT('Ctrl Pts',(-41.8226960778685,37.3128486708858,38.1837753567414));
#28647=CARTESIAN_POINT('Ctrl Pts',(-41.824873180091,37.3150260111601,38.1852277329705));
#28648=CARTESIAN_POINT('Ctrl Pts',(-41.8270488269186,37.3172058708259,38.1866785219074));
#28649=CARTESIAN_POINT('Ctrl Pts',(-41.8292230145128,37.3193882460825,38.1881277210263));
#28650=CARTESIAN_POINT('Ctrl Pts',(-41.8313972021068,37.3215706213391,38.1895769201452));
#28651=CARTESIAN_POINT('Ctrl Pts',(-41.8335699304674,37.3237555121865,38.191024529446));
#28652=CARTESIAN_POINT('Ctrl Pts',(-41.8357411957597,37.3259429148172,38.1924705464073));
#28653=CARTESIAN_POINT('Ctrl Pts',(-41.8379124610521,37.3281303174478,38.1939165633685));
#28654=CARTESIAN_POINT('Ctrl Pts',(-41.8400822632763,37.3303202318617,38.19536098799));
#28655=CARTESIAN_POINT('Ctrl Pts',(-41.8422505986016,37.3325126542441,38.1968038177549));
#28656=CARTESIAN_POINT('Ctrl Pts',(-41.844418933927,37.3347050766265,38.1982466475196));
#28657=CARTESIAN_POINT('Ctrl Pts',(-41.8465858023535,37.3369000069775,38.1996878824276));
#28658=CARTESIAN_POINT('Ctrl Pts',(-41.8487512000545,37.3390974414755,38.2011275199659));
#28659=CARTESIAN_POINT('Ctrl Pts',(-41.8509165977556,37.3412948759734,38.2025671575042));
#28660=CARTESIAN_POINT('Ctrl Pts',(-41.8530805247312,37.3434948146184,38.2040051976728));
#28661=CARTESIAN_POINT('Ctrl Pts',(-41.8552429771587,37.3456972535817,38.2054416379634));
#28662=CARTESIAN_POINT('Ctrl Pts',(-41.8574054295863,37.3478996925451,38.206878078254));
#28663=CARTESIAN_POINT('Ctrl Pts',(-41.8595664074657,37.3501046318268,38.2083129186665));
#28664=CARTESIAN_POINT('Ctrl Pts',(-41.8617259069785,37.3523120675913,38.2097461566969));
#28665=CARTESIAN_POINT('Ctrl Pts',(-41.8638854064913,37.3545195033558,38.2111793947272));
#28666=CARTESIAN_POINT('Ctrl Pts',(-41.8660434276374,37.3567294356032,38.2126110303754));
#28667=CARTESIAN_POINT('Ctrl Pts',(-41.8681999666023,37.3589418604908,38.2140410611418));
#28668=CARTESIAN_POINT('Ctrl Pts',(-41.8703565055672,37.3611542853783,38.2154710919082));
#28669=CARTESIAN_POINT('Ctrl Pts',(-41.8725115623508,37.3633692029062,38.2168995177928));
#28670=CARTESIAN_POINT('Ctrl Pts',(-41.8746651331427,37.3655866092248,38.2183263363003));
#28671=CARTESIAN_POINT('Ctrl Pts',(-41.8768206179049,37.367805986247,38.2197544228823));
#28672=CARTESIAN_POINT('Ctrl Pts',(-41.8789746140328,37.3700278564857,38.2211808992288));
#28673=CARTESIAN_POINT('Ctrl Pts',(-41.8811271177098,37.372252216074,38.2226057628425));
#28674=CARTESIAN_POINT('Ctrl Pts',(-41.7723865878497,37.2682864099502,38.1583090246979));
#28675=CARTESIAN_POINT('Ctrl Pts',(-41.77504070807,37.2708945608831,38.160124042574));
#28676=CARTESIAN_POINT('Ctrl Pts',(-41.7776926120407,37.2735066617433,38.1619366253151));
#28677=CARTESIAN_POINT('Ctrl Pts',(-41.7803422915794,37.2761227044715,38.1637467673286));
#28678=CARTESIAN_POINT('Ctrl Pts',(-41.7829919711183,37.2787387471996,38.1655569093422));
#28679=CARTESIAN_POINT('Ctrl Pts',(-41.7856394262253,37.2813587317957,38.1673646106282));
#28680=CARTESIAN_POINT('Ctrl Pts',(-41.788284648732,37.283982650176,38.1691698656093));
#28681=CARTESIAN_POINT('Ctrl Pts',(-41.7909298712387,37.2866065685563,38.1709751205904));
#28682=CARTESIAN_POINT('Ctrl Pts',(-41.7935728611452,37.2892344207208,38.1727779292665));
#28683=CARTESIAN_POINT('Ctrl Pts',(-41.7962136102967,37.2918661985616,38.1745782860751));
#28684=CARTESIAN_POINT('Ctrl Pts',(-41.7988543594482,37.2944979764025,38.1763786428838));
#28685=CARTESIAN_POINT('Ctrl Pts',(-41.8014928678447,37.2971336799196,38.1781765478251));
#28686=CARTESIAN_POINT('Ctrl Pts',(-41.8041291273455,37.2997733009808,38.1799719953518));
#28687=CARTESIAN_POINT('Ctrl Pts',(-41.8067653868463,37.302412922042,38.1817674428785));
#28688=CARTESIAN_POINT('Ctrl Pts',(-41.8093993974513,37.3050564606473,38.1835604329906));
#28689=CARTESIAN_POINT('Ctrl Pts',(-41.8120311510335,37.3077039086403,38.1853509601559));
#28690=CARTESIAN_POINT('Ctrl Pts',(-41.8146629046157,37.3103513566333,38.1871414873213));
#28691=CARTESIAN_POINT('Ctrl Pts',(-41.8172924011752,37.3130027140141,38.1889295515399));
#28692=CARTESIAN_POINT('Ctrl Pts',(-41.8199196325989,37.3156579726021,38.190715147295));
#28693=CARTESIAN_POINT('Ctrl Pts',(-41.8225468640225,37.3183132311901,38.19250074305));
#28694=CARTESIAN_POINT('Ctrl Pts',(-41.8251718303104,37.3209723909853,38.1942838703415));
#28695=CARTESIAN_POINT('Ctrl Pts',(-41.8277945233635,37.3236354437833,38.1960645236678));
#28696=CARTESIAN_POINT('Ctrl Pts',(-41.8304172164165,37.3262984965811,38.197845176994));
#28697=CARTESIAN_POINT('Ctrl Pts',(-41.8330376362347,37.3289654423818,38.199623356355));
#28698=CARTESIAN_POINT('Ctrl Pts',(-41.835655774733,37.3316362729565,38.2013990562643));
#28699=CARTESIAN_POINT('Ctrl Pts',(-41.8382739132314,37.3343071035311,38.2031747561737));
#28700=CARTESIAN_POINT('Ctrl Pts',(-41.8408897704098,37.33698181888,38.2049479766314));
#28701=CARTESIAN_POINT('Ctrl Pts',(-41.8435033381974,37.3396604107503,38.2067187121664));
#28702=CARTESIAN_POINT('Ctrl Pts',(-41.846116905985,37.3423390026207,38.2084894477014));
#28703=CARTESIAN_POINT('Ctrl Pts',(-41.8487281843818,37.3450214710125,38.2102576983137));
#28704=CARTESIAN_POINT('Ctrl Pts',(-41.8513371653309,37.3477078076495,38.2120234585475));
#28705=CARTESIAN_POINT('Ctrl Pts',(-41.85394614628,37.3503941442864,38.2137892187814));
#28706=CARTESIAN_POINT('Ctrl Pts',(-41.8565528297814,37.3530843491685,38.2155524886367));
#28707=CARTESIAN_POINT('Ctrl Pts',(-41.8591572077926,37.3557784139952,38.2173132626732));
#28708=CARTESIAN_POINT('Ctrl Pts',(-41.8617615858037,37.358472478822,38.2190740367097));
#28709=CARTESIAN_POINT('Ctrl Pts',(-41.8643636583245,37.3611704035935,38.2208323149273));
#28710=CARTESIAN_POINT('Ctrl Pts',(-41.8669634173266,37.3638721799855,38.2225880919011));
#28711=CARTESIAN_POINT('Ctrl Pts',(-41.8695631763287,37.3665739563775,38.224343868875));
#28712=CARTESIAN_POINT('Ctrl Pts',(-41.872160621812,37.3692795843902,38.2260971446049));
#28713=CARTESIAN_POINT('Ctrl Pts',(-41.8747557457625,37.3719890556753,38.2278479136815));
#28714=CARTESIAN_POINT('Ctrl Pts',(-41.877350869713,37.3746985269606,38.229598682758));
#28715=CARTESIAN_POINT('Ctrl Pts',(-41.8799436721306,37.3774118415184,38.2313469451812));
#28716=CARTESIAN_POINT('Ctrl Pts',(-41.8825341450154,37.3801289909773,38.2330926955569));
#28717=CARTESIAN_POINT('Ctrl Pts',(-41.8851246179004,37.3828461404361,38.2348384459327));
#28718=CARTESIAN_POINT('Ctrl Pts',(-41.8877127612526,37.3855671247958,38.2365816842609));
#28719=CARTESIAN_POINT('Ctrl Pts',(-41.8902985670866,37.3882919356613,38.2383224051631));
#28720=CARTESIAN_POINT('Ctrl Pts',(-41.8928866710366,37.3910191681824,38.2400646731182));
#28721=CARTESIAN_POINT('Ctrl Pts',(-41.8954724333117,37.3937502340137,38.2418044191706));
#28722=CARTESIAN_POINT('Ctrl Pts',(-41.8980558459195,37.3964851247139,38.2435416379429));
#28723=CARTESIAN_POINT('Ctrl Pts',(-41.7680088677671,37.2690766461197,38.1635750555802));
#28724=CARTESIAN_POINT('Ctrl Pts',(-41.7711198191088,37.2721510644396,38.1657306173963));
#28725=CARTESIAN_POINT('Ctrl Pts',(-41.774227766364,37.2752308368149,38.1678828784307));
#28726=CARTESIAN_POINT('Ctrl Pts',(-41.7773326970348,37.2783159508782,38.170031830055));
#28727=CARTESIAN_POINT('Ctrl Pts',(-41.7804376277057,37.2814010649415,38.1721807816792));
#28728=CARTESIAN_POINT('Ctrl Pts',(-41.7835395417922,37.2844915206928,38.1743264238931));
#28729=CARTESIAN_POINT('Ctrl Pts',(-41.7866384268199,37.2875873057234,38.176468748094));
#28730=CARTESIAN_POINT('Ctrl Pts',(-41.7897373118478,37.2906830907538,38.1786110722949));
#28731=CARTESIAN_POINT('Ctrl Pts',(-41.7928331678168,37.2937842050635,38.1807500784827));
#28732=CARTESIAN_POINT('Ctrl Pts',(-41.7959259822763,37.296890636202,38.1828857580804));
#28733=CARTESIAN_POINT('Ctrl Pts',(-41.7990187967359,37.2999970673404,38.1850214376781));
#28734=CARTESIAN_POINT('Ctrl Pts',(-41.802108569686,37.3031088153076,38.1871537906857));
#28735=CARTESIAN_POINT('Ctrl Pts',(-41.8051952886994,37.3062258676117,38.1892828085522));
#28736=CARTESIAN_POINT('Ctrl Pts',(-41.8082820077129,37.3093429199158,38.1914118264186));
#28737=CARTESIAN_POINT('Ctrl Pts',(-41.8113656727898,37.3124652765569,38.1935375091439));
#28738=CARTESIAN_POINT('Ctrl Pts',(-41.8144462715268,37.3155929250019,38.1956598482028));
#28739=CARTESIAN_POINT('Ctrl Pts',(-41.8175268702638,37.3187205734467,38.1977821872618));
#28740=CARTESIAN_POINT('Ctrl Pts',(-41.8206044026609,37.3218535136954,38.1999011826544));
#28741=CARTESIAN_POINT('Ctrl Pts',(-41.8236788563386,37.3249917331736,38.2020168258816));
#28742=CARTESIAN_POINT('Ctrl Pts',(-41.8267533100164,37.3281299526517,38.2041324691088));
#28743=CARTESIAN_POINT('Ctrl Pts',(-41.8298246849748,37.3312734513592,38.2062447601707));
#28744=CARTESIAN_POINT('Ctrl Pts',(-41.8328929688584,37.3344222166808,38.2083536905941));
#28745=CARTESIAN_POINT('Ctrl Pts',(-41.835961252742,37.3375709820023,38.2104626210175));
#28746=CARTESIAN_POINT('Ctrl Pts',(-41.8390264455507,37.3407250139377,38.2125681908025));
#28747=CARTESIAN_POINT('Ctrl Pts',(-41.8420885349533,37.3438842998304,38.2146703915024));
#28748=CARTESIAN_POINT('Ctrl Pts',(-41.8451506243559,37.3470435857233,38.2167725922022));
#28749=CARTESIAN_POINT('Ctrl Pts',(-41.8482096103522,37.3502081255734,38.2188714238168));
#28750=CARTESIAN_POINT('Ctrl Pts',(-41.851265480635,37.3533779066835,38.2209668779256));
#28751=CARTESIAN_POINT('Ctrl Pts',(-41.8543213509179,37.3565476877935,38.2230623320344));
#28752=CARTESIAN_POINT('Ctrl Pts',(-41.8573741054873,37.3597227101635,38.2251544086374));
#28753=CARTESIAN_POINT('Ctrl Pts',(-41.8604237320601,37.362902961055,38.2272430993402));
#28754=CARTESIAN_POINT('Ctrl Pts',(-41.863473358633,37.3660832119465,38.2293317900431));
#28755=CARTESIAN_POINT('Ctrl Pts',(-41.8665198572093,37.3692686913596,38.2314170948458));
#28756=CARTESIAN_POINT('Ctrl Pts',(-41.8695632155305,37.3724593865151,38.2334990053805));
#28757=CARTESIAN_POINT('Ctrl Pts',(-41.8726065738518,37.3756500816706,38.2355809159152));
#28758=CARTESIAN_POINT('Ctrl Pts',(-41.8756467919178,37.3788459925686,38.2376594321818));
#28759=CARTESIAN_POINT('Ctrl Pts',(-41.8786838574945,37.3820471063893,38.2397345458388));
#28760=CARTESIAN_POINT('Ctrl Pts',(-41.8817209230711,37.3852482202101,38.2418096594958));
#28761=CARTESIAN_POINT('Ctrl Pts',(-41.8847548361584,37.3884545369535,38.2438813705433));
#28762=CARTESIAN_POINT('Ctrl Pts',(-41.8877855845465,37.3916660437595,38.2459496706661));
#28763=CARTESIAN_POINT('Ctrl Pts',(-41.8908163329347,37.3948775505653,38.2480179707889));
#28764=CARTESIAN_POINT('Ctrl Pts',(-41.8938439166238,37.3980942474337,38.250082859987));
#28765=CARTESIAN_POINT('Ctrl Pts',(-41.8968683234287,37.4013161214637,38.2521443299721));
#28766=CARTESIAN_POINT('Ctrl Pts',(-41.8998927302336,37.4045379954937,38.2542057999571));
#28767=CARTESIAN_POINT('Ctrl Pts',(-41.9029139601543,37.4077650466855,38.256263850729));
#28768=CARTESIAN_POINT('Ctrl Pts',(-41.9059320010304,37.4109972620978,38.2583184740259));
#28769=CARTESIAN_POINT('Ctrl Pts',(-41.9089527241683,37.4142323501178,38.2603749233541));
#28770=CARTESIAN_POINT('Ctrl Pts',(-41.9119702525905,37.4174726115418,38.2624279391123));
#28771=CARTESIAN_POINT('Ctrl Pts',(-41.9149845741293,37.4207180333538,38.2644775130434));
#28772=CARTESIAN_POINT('Ctrl Pts',(-41.7635986248403,37.2698289147397,38.1688091004257));
#28773=CARTESIAN_POINT('Ctrl Pts',(-41.767170149167,37.2733820604892,38.1713220115573));
#28774=CARTESIAN_POINT('Ctrl Pts',(-41.7707376507708,37.2769423757664,38.1738305026664));
#28775=CARTESIAN_POINT('Ctrl Pts',(-41.774301110476,37.2805098414877,38.1763345603498));
#28776=CARTESIAN_POINT('Ctrl Pts',(-41.7778645701812,37.284077307209,38.1788386180331));
#28777=CARTESIAN_POINT('Ctrl Pts',(-41.7814239879878,37.2876519233744,38.1813382422907));
#28778=CARTESIAN_POINT('Ctrl Pts',(-41.7849793447612,37.2912336708281,38.1838334197642));
#28779=CARTESIAN_POINT('Ctrl Pts',(-41.7885347015346,37.2948154182817,38.1863285972376));
#28780=CARTESIAN_POINT('Ctrl Pts',(-41.7920859972746,37.2984042970236,38.1888193279269));
#28781=CARTESIAN_POINT('Ctrl Pts',(-41.7956332128876,37.3020002878258,38.1913055985184));
#28782=CARTESIAN_POINT('Ctrl Pts',(-41.7991804285007,37.305596278628,38.19379186911));
#28783=CARTESIAN_POINT('Ctrl Pts',(-41.8027235639866,37.3091993814906,38.1962736796039));
#28784=CARTESIAN_POINT('Ctrl Pts',(-41.806262600293,37.3128095771137,38.1987510167316));
#28785=CARTESIAN_POINT('Ctrl Pts',(-41.8098016365993,37.3164197727369,38.2012283538592));
#28786=CARTESIAN_POINT('Ctrl Pts',(-41.813336573726,37.3200370611205,38.2037012176207));
#28787=CARTESIAN_POINT('Ctrl Pts',(-41.8168673926618,37.3236614228931,38.2061695947926));
#28788=CARTESIAN_POINT('Ctrl Pts',(-41.8203982115976,37.3272857846658,38.2086379719645));
#28789=CARTESIAN_POINT('Ctrl Pts',(-41.8239249123425,37.3309172198275,38.2111018625468));
#28790=CARTESIAN_POINT('Ctrl Pts',(-41.8274474759268,37.3345557089351,38.2135612533614));
#28791=CARTESIAN_POINT('Ctrl Pts',(-41.8309700395111,37.3381941980428,38.216020644176));
#28792=CARTESIAN_POINT('Ctrl Pts',(-41.8344884659347,37.3418397410965,38.2184755352229));
#28793=CARTESIAN_POINT('Ctrl Pts',(-41.8380027362697,37.3454923185817,38.2209259133694));
#28794=CARTESIAN_POINT('Ctrl Pts',(-41.8415170066047,37.349144896067,38.2233762915158));
#28795=CARTESIAN_POINT('Ctrl Pts',(-41.8450271208511,37.3528045079838,38.2258221567618));
#28796=CARTESIAN_POINT('Ctrl Pts',(-41.8485330601227,37.3564711347466,38.2282634960202));
#28797=CARTESIAN_POINT('Ctrl Pts',(-41.8520389993942,37.3601377615094,38.2307048352785));
#28798=CARTESIAN_POINT('Ctrl Pts',(-41.855540763691,37.3638114031182,38.2331416485492));
#28799=CARTESIAN_POINT('Ctrl Pts',(-41.8590383341689,37.3674920399165,38.2355739227905));
#28800=CARTESIAN_POINT('Ctrl Pts',(-41.8625359046468,37.3711726767147,38.2380061970319));
#28801=CARTESIAN_POINT('Ctrl Pts',(-41.8660292813057,37.3748603087024,38.240433932244));
#28802=CARTESIAN_POINT('Ctrl Pts',(-41.8695184453439,37.3785549161521,38.2428571154308));
#28803=CARTESIAN_POINT('Ctrl Pts',(-41.873007609382,37.3822495236018,38.2452802986178));
#28804=CARTESIAN_POINT('Ctrl Pts',(-41.8764925607994,37.3859511065137,38.2476989297795));
#28805=CARTESIAN_POINT('Ctrl Pts',(-41.8799732808366,37.3896596450895,38.250112995966));
#28806=CARTESIAN_POINT('Ctrl Pts',(-41.8834540008737,37.3933681836653,38.2525270621525));
#28807=CARTESIAN_POINT('Ctrl Pts',(-41.8869304895305,37.3970836779052,38.2549365633638));
#28808=CARTESIAN_POINT('Ctrl Pts',(-41.8904027280903,37.4008061079406,38.257341486696));
#28809=CARTESIAN_POINT('Ctrl Pts',(-41.89387496665,37.404528537976,38.2597464100281));
#28810=CARTESIAN_POINT('Ctrl Pts',(-41.8973429551125,37.4082579038071,38.2621467554809));
#28811=CARTESIAN_POINT('Ctrl Pts',(-41.9008066748037,37.4119941854949,38.2645425101966));
#28812=CARTESIAN_POINT('Ctrl Pts',(-41.904270394495,37.4157304671828,38.2669382649123));
#28813=CARTESIAN_POINT('Ctrl Pts',(-41.9077298454149,37.4194736647275,38.2693294288908));
#28814=CARTESIAN_POINT('Ctrl Pts',(-41.9111850089323,37.4232237581202,38.2717159893205));
#28815=CARTESIAN_POINT('Ctrl Pts',(-41.9146401724497,37.4269738515128,38.2741025497502));
#28816=CARTESIAN_POINT('Ctrl Pts',(-41.9180910485645,37.4307308407536,38.2764845066309));
#28817=CARTESIAN_POINT('Ctrl Pts',(-41.9215376186886,37.4344947057637,38.2788618471974));
#28818=CARTESIAN_POINT('Ctrl Pts',(-41.9249872519267,37.438261915881,38.2812413006078));
#28819=CARTESIAN_POINT('Ctrl Pts',(-41.9284325715169,37.4420360139948,38.2836161294949));
#28820=CARTESIAN_POINT('Ctrl Pts',(-41.9318735588647,37.4458169799027,38.2859863211058));
#28821=CARTESIAN_POINT('Ctrl Pts',(-41.7591585257862,37.2705463289668,38.1740137819355));
#28822=CARTESIAN_POINT('Ctrl Pts',(-41.7631892704991,37.2745846634979,38.1768957540815));
#28823=CARTESIAN_POINT('Ctrl Pts',(-41.7672147321291,37.2786324138423,38.1797719213672));
#28824=CARTESIAN_POINT('Ctrl Pts',(-41.7712348810694,37.2826895502289,38.1826422626386));
#28825=CARTESIAN_POINT('Ctrl Pts',(-41.7752550300097,37.2867466866155,38.1855126039099));
#28826=CARTESIAN_POINT('Ctrl Pts',(-41.7792698662602,37.2908132090444,38.1883771191669));
#28827=CARTESIAN_POINT('Ctrl Pts',(-41.783279360292,37.2948890876066,38.1912357873412));
#28828=CARTESIAN_POINT('Ctrl Pts',(-41.7872888543238,37.2989649661687,38.1940944555156));
#28829=CARTESIAN_POINT('Ctrl Pts',(-41.791293006137,37.3030502008641,38.1969472766072));
#28830=CARTESIAN_POINT('Ctrl Pts',(-41.7952917862812,37.3071447616462,38.1997942296338));
#28831=CARTESIAN_POINT('Ctrl Pts',(-41.7992905664254,37.3112393224283,38.2026411826604));
#28832=CARTESIAN_POINT('Ctrl Pts',(-41.8032839749007,37.315343209297,38.2054822676221));
#28833=CARTESIAN_POINT('Ctrl Pts',(-41.8072719823357,37.3194563920684,38.2083174636227));
#28834=CARTESIAN_POINT('Ctrl Pts',(-41.8112599897708,37.3235695748399,38.2111526596233));
#28835=CARTESIAN_POINT('Ctrl Pts',(-41.8152425961656,37.3276920535142,38.2139819666629));
#28836=CARTESIAN_POINT('Ctrl Pts',(-41.8192197722285,37.3318237977707,38.2168053639321));
#28837=CARTESIAN_POINT('Ctrl Pts',(-41.8231969482913,37.3359555420272,38.2196287612014));
#28838=CARTESIAN_POINT('Ctrl Pts',(-41.8271686940221,37.3400965518658,38.2224462487002));
#28839=CARTESIAN_POINT('Ctrl Pts',(-41.8311349802089,37.34424679683,38.2252578057062));
#28840=CARTESIAN_POINT('Ctrl Pts',(-41.8351012663957,37.348397041794,38.2280693627123));
#28841=CARTESIAN_POINT('Ctrl Pts',(-41.8390620930385,37.3525565218834,38.2308749892255));
#28842=CARTESIAN_POINT('Ctrl Pts',(-41.8430174310058,37.3567252065055,38.2336746646106));
#28843=CARTESIAN_POINT('Ctrl Pts',(-41.846972768973,37.3608938911276,38.2364743399958));
#28844=CARTESIAN_POINT('Ctrl Pts',(-41.8509226182647,37.3650717802822,38.2392680642529));
#28845=CARTESIAN_POINT('Ctrl Pts',(-41.8548669498298,37.3692588432415,38.2420558168344));
#28846=CARTESIAN_POINT('Ctrl Pts',(-41.8588112813949,37.3734459062008,38.2448435694158));
#28847=CARTESIAN_POINT('Ctrl Pts',(-41.8627500952336,37.3776421429644,38.2476253503216));
#28848=CARTESIAN_POINT('Ctrl Pts',(-41.866683362376,37.3818475226697,38.2504011390917));
#28849=CARTESIAN_POINT('Ctrl Pts',(-41.8706166295184,37.3860529023749,38.253176927862));
#28850=CARTESIAN_POINT('Ctrl Pts',(-41.8745443499646,37.3902674250216,38.2559467244967));
#28851=CARTESIAN_POINT('Ctrl Pts',(-41.8784664948264,37.3944910596122,38.2587105086242));
#28852=CARTESIAN_POINT('Ctrl Pts',(-41.8823886396882,37.3987146942029,38.2614742927517));
#28853=CARTESIAN_POINT('Ctrl Pts',(-41.8863052089657,37.4029474407374,38.264232064372));
#28854=CARTESIAN_POINT('Ctrl Pts',(-41.8902161738527,37.4071892680843,38.2669838032018));
#28855=CARTESIAN_POINT('Ctrl Pts',(-41.8941271387397,37.4114310954311,38.2697355420317));
#28856=CARTESIAN_POINT('Ctrl Pts',(-41.8980324992362,37.4156820035903,38.2724812480711));
#28857=CARTESIAN_POINT('Ctrl Pts',(-41.9019322266185,37.4199419612967,38.2752209011256));
#28858=CARTESIAN_POINT('Ctrl Pts',(-41.9058319540008,37.4242019190032,38.27796055418));
#28859=CARTESIAN_POINT('Ctrl Pts',(-41.909726048269,37.4284709262567,38.2806941542496));
#28860=CARTESIAN_POINT('Ctrl Pts',(-41.9136144807821,37.4327489516591,38.2834216812288));
#28861=CARTESIAN_POINT('Ctrl Pts',(-41.9175029132953,37.4370269770616,38.2861492082079));
#28862=CARTESIAN_POINT('Ctrl Pts',(-41.9213856840535,37.4413140206129,38.2888706620967));
#28863=CARTESIAN_POINT('Ctrl Pts',(-41.9252627644992,37.4456100507822,38.2915860228789));
#28864=CARTESIAN_POINT('Ctrl Pts',(-41.9291398449449,37.4499060809515,38.2943013836612));
#28865=CARTESIAN_POINT('Ctrl Pts',(-41.933011235078,37.4542110977388,38.2970106513369));
#28866=CARTESIAN_POINT('Ctrl Pts',(-41.9368769064249,37.4585250694809,38.2997138059797));
#28867=CARTESIAN_POINT('Ctrl Pts',(-41.9407460133587,37.4628428752336,38.3024193630313));
#28868=CARTESIAN_POINT('Ctrl Pts',(-41.9446093913366,37.4671696518656,38.3051187961791));
#28869=CARTESIAN_POINT('Ctrl Pts',(-41.9484670118931,37.4715053674971,38.3078120855339));
#28870=CARTESIAN_POINT('Ctrl Pts',(-41.7547184267321,37.271263743194,38.1792184634453));
#28871=CARTESIAN_POINT('Ctrl Pts',(-41.7592083918311,37.2757872665067,38.1824694966057));
#28872=CARTESIAN_POINT('Ctrl Pts',(-41.7636918134875,37.2803224519181,38.1857133400681));
#28873=CARTESIAN_POINT('Ctrl Pts',(-41.7681686516628,37.28486925897,38.1889499649274));
#28874=CARTESIAN_POINT('Ctrl Pts',(-41.7726454898382,37.2894160660219,38.1921865897868));
#28875=CARTESIAN_POINT('Ctrl Pts',(-41.7771157445325,37.2939744947144,38.1954159960432));
#28876=CARTESIAN_POINT('Ctrl Pts',(-41.7815793758228,37.2985445043851,38.1986381549183));
#28877=CARTESIAN_POINT('Ctrl Pts',(-41.7860430071131,37.3031145140558,38.2018603137936));
#28878=CARTESIAN_POINT('Ctrl Pts',(-41.7905000149993,37.3076961047048,38.2050752252875));
#28879=CARTESIAN_POINT('Ctrl Pts',(-41.7949503596747,37.3122892354667,38.2082828607492));
#28880=CARTESIAN_POINT('Ctrl Pts',(-41.7994007043501,37.3168823662286,38.2114904962109));
#28881=CARTESIAN_POINT('Ctrl Pts',(-41.8038443858147,37.3214870371033,38.2146908556402));
#28882=CARTESIAN_POINT('Ctrl Pts',(-41.8082813643785,37.3261032070232,38.2178839105138));
#28883=CARTESIAN_POINT('Ctrl Pts',(-41.8127183429423,37.330719376943,38.2210769653874));
#28884=CARTESIAN_POINT('Ctrl Pts',(-41.8171486186053,37.3353470459079,38.2242627157051));
#28885=CARTESIAN_POINT('Ctrl Pts',(-41.8215721517952,37.3399861726482,38.2274411330717));
#28886=CARTESIAN_POINT('Ctrl Pts',(-41.825995684985,37.3446252993886,38.2306195504382));
#28887=CARTESIAN_POINT('Ctrl Pts',(-41.8304124757016,37.3492758839043,38.2337906348536));
#28888=CARTESIAN_POINT('Ctrl Pts',(-41.834822484491,37.3539378847247,38.2369543580511));
#28889=CARTESIAN_POINT('Ctrl Pts',(-41.8392324932803,37.3585998855452,38.2401180812485));
#28890=CARTESIAN_POINT('Ctrl Pts',(-41.8436357201424,37.3632733026704,38.243274443228));
#28891=CARTESIAN_POINT('Ctrl Pts',(-41.8480321257418,37.3679580944293,38.2464234158519));
#28892=CARTESIAN_POINT('Ctrl Pts',(-41.8524285313413,37.3726428861882,38.2495723884758));
#28893=CARTESIAN_POINT('Ctrl Pts',(-41.8568181156782,37.3773390525808,38.252713971744));
#28894=CARTESIAN_POINT('Ctrl Pts',(-41.8612008395369,37.3820465517364,38.2558481376486));
#28895=CARTESIAN_POINT('Ctrl Pts',(-41.8655835633956,37.3867540508921,38.2589823035531));
#28896=CARTESIAN_POINT('Ctrl Pts',(-41.8699594267761,37.3914728828107,38.2621090520939));
#28897=CARTESIAN_POINT('Ctrl Pts',(-41.8743283905831,37.396203005423,38.265228355393));
#28898=CARTESIAN_POINT('Ctrl Pts',(-41.8786973543901,37.4009331280351,38.2683476586921));
#28899=CARTESIAN_POINT('Ctrl Pts',(-41.8830594186235,37.4056745413409,38.2714595167494));
#28900=CARTESIAN_POINT('Ctrl Pts',(-41.887414544309,37.4104272030723,38.2745639018175));
#28901=CARTESIAN_POINT('Ctrl Pts',(-41.8917696699944,37.4151798648039,38.2776682868856));
#28902=CARTESIAN_POINT('Ctrl Pts',(-41.8961178571319,37.4199437749612,38.2807651989644));
#28903=CARTESIAN_POINT('Ctrl Pts',(-41.9004590668688,37.4247188910791,38.2838546104377));
#28904=CARTESIAN_POINT('Ctrl Pts',(-41.9048002766057,37.429494007197,38.2869440219109));
#28905=CARTESIAN_POINT('Ctrl Pts',(-41.9091345089417,37.4342803292756,38.2900259327783));
#28906=CARTESIAN_POINT('Ctrl Pts',(-41.9134617251467,37.4390778146529,38.2931003155552));
#28907=CARTESIAN_POINT('Ctrl Pts',(-41.9177889413516,37.4438753000302,38.2961746983321));
#28908=CARTESIAN_POINT('Ctrl Pts',(-41.9221091414255,37.4486839487062,38.2992415530183));
#28909=CARTESIAN_POINT('Ctrl Pts',(-41.9264222867606,37.4535037178233,38.3023008522609));
#28910=CARTESIAN_POINT('Ctrl Pts',(-41.9307354320957,37.4583234869404,38.3053601515035));
#28911=CARTESIAN_POINT('Ctrl Pts',(-41.9350415226922,37.4631543764984,38.3084118953025));
#28912=CARTESIAN_POINT('Ctrl Pts',(-41.9393405200661,37.4679963434443,38.3114560564374));
#28913=CARTESIAN_POINT('Ctrl Pts',(-41.9436395174402,37.4728383103901,38.3145002175723));
#28914=CARTESIAN_POINT('Ctrl Pts',(-41.9479314215916,37.4776913547239,38.317536796043));
#28915=CARTESIAN_POINT('Ctrl Pts',(-41.9522161941611,37.482555433198,38.320565764762));
#28916=CARTESIAN_POINT('Ctrl Pts',(-41.9565047747907,37.4874238345862,38.3235974254546));
#28917=CARTESIAN_POINT('Ctrl Pts',(-41.9607862111563,37.4923032897364,38.3266214628634));
#28918=CARTESIAN_POINT('Ctrl Pts',(-41.9650604649214,37.4971937550915,38.329637849962));
#28919=CARTESIAN_POINT('Ctrl Pts',(-41.7502484969702,37.2719463327032,38.1843938066194));
#28920=CARTESIAN_POINT('Ctrl Pts',(-41.7551962256523,37.276961374585,38.1880254939256));
#28921=CARTESIAN_POINT('Ctrl Pts',(-41.7601359088508,37.2819907555891,38.1916483411455));
#28922=CARTESIAN_POINT('Ctrl Pts',(-41.7650674923212,37.2870344205738,38.1952623086258));
#28923=CARTESIAN_POINT('Ctrl Pts',(-41.7699990757916,37.2920780855585,38.1988762761062));
#28924=CARTESIAN_POINT('Ctrl Pts',(-41.7749225595338,37.2971360345237,38.2024813638471));
#28925=CARTESIAN_POINT('Ctrl Pts',(-41.7798378894764,37.3022082120227,38.2060775323852));
#28926=CARTESIAN_POINT('Ctrl Pts',(-41.784753219419,37.3072803895216,38.2096737009232));
#28927=CARTESIAN_POINT('Ctrl Pts',(-41.7896603955619,37.3123667955542,38.2132609502583));
#28928=CARTESIAN_POINT('Ctrl Pts',(-41.7945593640076,37.3174673743695,38.2168392411177));
#28929=CARTESIAN_POINT('Ctrl Pts',(-41.7994583324533,37.3225679531848,38.2204175319771));
#28930=CARTESIAN_POINT('Ctrl Pts',(-41.8043490932019,37.3276827047826,38.2239868643607));
#28931=CARTESIAN_POINT('Ctrl Pts',(-41.8092315925311,37.3328115731093,38.2275471991868));
#28932=CARTESIAN_POINT('Ctrl Pts',(-41.8141140918603,37.3379404414361,38.231107534013));
#28933=CARTESIAN_POINT('Ctrl Pts',(-41.8189883297701,37.3430834264914,38.2346588712817));
#28934=CARTESIAN_POINT('Ctrl Pts',(-41.8238542527147,37.3482404719199,38.2382011721036));
#28935=CARTESIAN_POINT('Ctrl Pts',(-41.8287201756593,37.3533975173484,38.2417434729254));
#28936=CARTESIAN_POINT('Ctrl Pts',(-41.8335777836387,37.3585686231499,38.2452767373004));
#28937=CARTESIAN_POINT('Ctrl Pts',(-41.8384270232845,37.3637537326682,38.2488009265318));
#28938=CARTESIAN_POINT('Ctrl Pts',(-41.8432762629303,37.3689388421866,38.2523251157632));
#28939=CARTESIAN_POINT('Ctrl Pts',(-41.8481171342425,37.3741379554216,38.2558402298512));
#28940=CARTESIAN_POINT('Ctrl Pts',(-41.8529495840314,37.3793510154178,38.2593462302928));
#28941=CARTESIAN_POINT('Ctrl Pts',(-41.8577820338202,37.3845640754139,38.2628522307343));
#28942=CARTESIAN_POINT('Ctrl Pts',(-41.8626060620857,37.389791082171,38.2663491175296));
#28943=CARTESIAN_POINT('Ctrl Pts',(-41.8674216158177,37.3950319784353,38.2698368523701));
#28944=CARTESIAN_POINT('Ctrl Pts',(-41.8722371695496,37.4002728746996,38.2733245872106));
#28945=CARTESIAN_POINT('Ctrl Pts',(-41.8770442487481,37.4055276604708,38.2768031700963));
#28946=CARTESIAN_POINT('Ctrl Pts',(-41.8818428005838,37.4107962781982,38.2802725629143));
#28947=CARTESIAN_POINT('Ctrl Pts',(-41.8866413524195,37.4160648959255,38.2837419557322));
#28948=CARTESIAN_POINT('Ctrl Pts',(-41.8914313768924,37.4213473456087,38.2872021584824));
#28949=CARTESIAN_POINT('Ctrl Pts',(-41.8962128213549,37.4266435694012,38.2906531332478));
#28950=CARTESIAN_POINT('Ctrl Pts',(-41.9009942658176,37.4319397931935,38.2941041080132));
#28951=CARTESIAN_POINT('Ctrl Pts',(-41.9057671302699,37.4372497910949,38.2975458547937));
#28952=CARTESIAN_POINT('Ctrl Pts',(-41.9105313622474,37.4425735049638,38.3009783358694));
#28953=CARTESIAN_POINT('Ctrl Pts',(-41.915295594225,37.4478972188327,38.3044108169451));
#28954=CARTESIAN_POINT('Ctrl Pts',(-41.9200511937278,37.4532346486689,38.3078340323158));
#28955=CARTESIAN_POINT('Ctrl Pts',(-41.9247981084754,37.4585857360373,38.3112479444592));
#28956=CARTESIAN_POINT('Ctrl Pts',(-41.9295450232231,37.4639368234058,38.3146618566026));
#28957=CARTESIAN_POINT('Ctrl Pts',(-41.9342832532155,37.4693015683065,38.3180664655185));
#28958=CARTESIAN_POINT('Ctrl Pts',(-41.9390127463574,37.4746799120121,38.321461733883));
#28959=CARTESIAN_POINT('Ctrl Pts',(-41.9437422394994,37.4800582557176,38.3248570022476));
#28960=CARTESIAN_POINT('Ctrl Pts',(-41.9484629957909,37.4854501982279,38.3282429300606));
#28961=CARTESIAN_POINT('Ctrl Pts',(-41.9531749633228,37.4908556805245,38.3316194801973));
#28962=CARTESIAN_POINT('Ctrl Pts',(-41.9578869308548,37.4962611628211,38.3349960303341));
#28963=CARTESIAN_POINT('Ctrl Pts',(-41.9625901096271,37.5016801849039,38.3383632027944));
#28964=CARTESIAN_POINT('Ctrl Pts',(-41.9672844479182,37.5071126874645,38.3417209606536));
#28965=CARTESIAN_POINT('Ctrl Pts',(-41.9719829582679,37.512550018122,38.3450817026954));
#28966=CARTESIAN_POINT('Ctrl Pts',(-41.9766726124154,37.5180008532292,38.3484330133941));
#28967=CARTESIAN_POINT('Ctrl Pts',(-41.98135335869,37.5234651330302,38.3517748559277));
#28968=CARTESIAN_POINT('Ctrl Pts',(-41.7457520939339,37.2725980170017,38.1895431134749));
#28969=CARTESIAN_POINT('Ctrl Pts',(-41.7511511407049,37.278104218446,38.19356073873));
#28970=CARTESIAN_POINT('Ctrl Pts',(-41.7565404115942,37.2836278430274,38.1975676225998));
#28971=CARTESIAN_POINT('Ctrl Pts',(-41.7619198332558,37.2891688155715,38.2015637105522));
#28972=CARTESIAN_POINT('Ctrl Pts',(-41.7672992549175,37.2947097881156,38.2055597985045));
#28973=CARTESIAN_POINT('Ctrl Pts',(-41.7726688273513,37.3002681086224,38.2095450905392));
#28974=CARTESIAN_POINT('Ctrl Pts',(-41.7780284774797,37.3058437014451,38.2135195324181));
#28975=CARTESIAN_POINT('Ctrl Pts',(-41.783388127608,37.3114192942678,38.2174939742969));
#28976=CARTESIAN_POINT('Ctrl Pts',(-41.7887378554306,37.3170121594064,38.2214575660198));
#28977=CARTESIAN_POINT('Ctrl Pts',(-41.7940775881398,37.3226222207441,38.2254102536438));
#28978=CARTESIAN_POINT('Ctrl Pts',(-41.799417320849,37.3282322820818,38.2293629412678));
#28979=CARTESIAN_POINT('Ctrl Pts',(-41.8047470584447,37.3338595396184,38.2333047247928));
#28980=CARTESIAN_POINT('Ctrl Pts',(-41.8100667283911,37.3395039167693,38.2372355505726));
#28981=CARTESIAN_POINT('Ctrl Pts',(-41.8153863983375,37.3451482939202,38.2411663763523));
#28982=CARTESIAN_POINT('Ctrl Pts',(-41.8206960006346,37.3508097906851,38.2450862443869));
#28983=CARTESIAN_POINT('Ctrl Pts',(-41.8259954630207,37.3564883300132,38.2489951013283));
#28984=CARTESIAN_POINT('Ctrl Pts',(-41.8312949254068,37.3621668693414,38.2529039582697));
#28985=CARTESIAN_POINT('Ctrl Pts',(-41.8365842478817,37.3678624512327,38.2568018041178));
#28986=CARTESIAN_POINT('Ctrl Pts',(-41.8418633584599,37.3735749981724,38.2606885858245));
#28987=CARTESIAN_POINT('Ctrl Pts',(-41.8471424690381,37.3792875451122,38.2645753675312));
#28988=CARTESIAN_POINT('Ctrl Pts',(-41.8524113677194,37.3850170571003,38.2684510850964));
#28989=CARTESIAN_POINT('Ctrl Pts',(-41.8576699827962,37.3907634561602,38.2723156857731));
#28990=CARTESIAN_POINT('Ctrl Pts',(-41.8629285978729,37.3965098552201,38.2761802864498));
#28991=CARTESIAN_POINT('Ctrl Pts',(-41.868176929345,37.4022731413517,38.2800337702378));
#28992=CARTESIAN_POINT('Ctrl Pts',(-41.8734149057845,37.408053236119,38.2838760846927));
#28993=CARTESIAN_POINT('Ctrl Pts',(-41.8786528822242,37.4138333308862,38.2877183991477));
#28994=CARTESIAN_POINT('Ctrl Pts',(-41.8838805036312,37.419630234289,38.2915495442695));
#28995=CARTESIAN_POINT('Ctrl Pts',(-41.8890976988597,37.4254438674336,38.2953694679178));
#28996=CARTESIAN_POINT('Ctrl Pts',(-41.8943148940882,37.4312575005782,38.299189391566));
#28997=CARTESIAN_POINT('Ctrl Pts',(-41.8995216631381,37.4370878634646,38.3029980937406));
#28998=CARTESIAN_POINT('Ctrl Pts',(-41.9047179351473,37.4429348767437,38.3067955226066));
#28999=CARTESIAN_POINT('Ctrl Pts',(-41.9099142071565,37.4487818900228,38.3105929514726));
#29000=CARTESIAN_POINT('Ctrl Pts',(-41.9150999821248,37.4546455536944,38.3143791070299));
#29001=CARTESIAN_POINT('Ctrl Pts',(-41.9202751894758,37.4605257879565,38.3181539377503));
#29002=CARTESIAN_POINT('Ctrl Pts',(-41.9254503968269,37.4664060222185,38.3219287684708));
#29003=CARTESIAN_POINT('Ctrl Pts',(-41.9306150365605,37.4723028270709,38.3256922743543));
#29004=CARTESIAN_POINT('Ctrl Pts',(-41.935769038388,37.4782161222602,38.329444404181));
#29005=CARTESIAN_POINT('Ctrl Pts',(-41.9409230402155,37.4841294174496,38.3331965340078));
#29006=CARTESIAN_POINT('Ctrl Pts',(-41.9460664041368,37.4900592029758,38.3369372877777));
#29007=CARTESIAN_POINT('Ctrl Pts',(-41.9511990601526,37.4960053981369,38.3406666145804));
#29008=CARTESIAN_POINT('Ctrl Pts',(-41.9563317161684,37.5019515932978,38.3443959413833));
#29009=CARTESIAN_POINT('Ctrl Pts',(-41.9614536642786,37.5079141980935,38.3481138412189));
#29010=CARTESIAN_POINT('Ctrl Pts',(-41.9665648347755,37.513893131375,38.3518202634881));
#29011=CARTESIAN_POINT('Ctrl Pts',(-41.9716760052724,37.5198720646565,38.3555266857574));
#29012=CARTESIAN_POINT('Ctrl Pts',(-41.9767763981558,37.5258673264238,38.3592216304602));
#29013=CARTESIAN_POINT('Ctrl Pts',(-41.9818659440114,37.5318788350836,38.3629050473097));
#29014=CARTESIAN_POINT('Ctrl Pts',(-41.9869600131636,37.5378956864276,38.366591737769));
#29015=CARTESIAN_POINT('Ctrl Pts',(-41.9920432159987,37.5439288135554,38.3702668798752));
#29016=CARTESIAN_POINT('Ctrl Pts',(-41.9971154832133,37.5499781342127,38.3739304235221));
#29017=CARTESIAN_POINT('Ctrl Pts',(-41.7412556908976,37.2732497013001,38.1946924203304));
#29018=CARTESIAN_POINT('Ctrl Pts',(-41.7471060557576,37.2792470623069,38.1990959835345));
#29019=CARTESIAN_POINT('Ctrl Pts',(-41.7529449143376,37.2852649304657,38.2034869040542));
#29020=CARTESIAN_POINT('Ctrl Pts',(-41.7587721741905,37.2913032105692,38.2078651124785));
#29021=CARTESIAN_POINT('Ctrl Pts',(-41.7645994340434,37.2973414906728,38.2122433209027));
#29022=CARTESIAN_POINT('Ctrl Pts',(-41.7704150951689,37.303400182721,38.2166088172313));
#29023=CARTESIAN_POINT('Ctrl Pts',(-41.7762190654829,37.3094791908675,38.220961532451));
#29024=CARTESIAN_POINT('Ctrl Pts',(-41.782023035797,37.315558199014,38.2253142476706));
#29025=CARTESIAN_POINT('Ctrl Pts',(-41.7878153152994,37.3216575232586,38.2296541817813));
#29026=CARTESIAN_POINT('Ctrl Pts',(-41.793595812272,37.3277770671187,38.2339812661699));
#29027=CARTESIAN_POINT('Ctrl Pts',(-41.7993763092447,37.3338966109788,38.2383083505585));
#29028=CARTESIAN_POINT('Ctrl Pts',(-41.8051450236875,37.3400363744543,38.2426225852248));
#29029=CARTESIAN_POINT('Ctrl Pts',(-41.8109018642511,37.3461962604293,38.2469239019583));
#29030=CARTESIAN_POINT('Ctrl Pts',(-41.8166587048148,37.3523561464043,38.2512252186917));
#29031=CARTESIAN_POINT('Ctrl Pts',(-41.8224036714991,37.3585361548787,38.2555136174921));
#29032=CARTESIAN_POINT('Ctrl Pts',(-41.8281366733266,37.3647361881066,38.259789030553));
#29033=CARTESIAN_POINT('Ctrl Pts',(-41.8338696751542,37.3709362213344,38.2640644436139));
#29034=CARTESIAN_POINT('Ctrl Pts',(-41.8395907121247,37.3771562793155,38.2683268709353));
#29035=CARTESIAN_POINT('Ctrl Pts',(-41.8452996936353,37.3833962636767,38.2725762451173));
#29036=CARTESIAN_POINT('Ctrl Pts',(-41.8510086751459,37.3896362480378,38.2768256192993));
#29037=CARTESIAN_POINT('Ctrl Pts',(-41.8567056011963,37.3958961587788,38.2810619403417));
#29038=CARTESIAN_POINT('Ctrl Pts',(-41.8623903815609,37.4021758969026,38.2852851412534));
#29039=CARTESIAN_POINT('Ctrl Pts',(-41.8680751619256,37.4084556350262,38.2895083421652));
#29040=CARTESIAN_POINT('Ctrl Pts',(-41.8737477966043,37.4147552005324,38.293718422946));
#29041=CARTESIAN_POINT('Ctrl Pts',(-41.8794081957515,37.4210744938026,38.2979153170154));
#29042=CARTESIAN_POINT('Ctrl Pts',(-41.8850685948987,37.4273937870729,38.3021122110849));
#29043=CARTESIAN_POINT('Ctrl Pts',(-41.8907167585142,37.4337328081071,38.3062959184427));
#29044=CARTESIAN_POINT('Ctrl Pts',(-41.8963525971356,37.440091456669,38.3104663729213));
#29045=CARTESIAN_POINT('Ctrl Pts',(-41.901988435757,37.446450105231,38.3146368273998));
#29046=CARTESIAN_POINT('Ctrl Pts',(-41.9076119493839,37.4528283813204,38.3187940289989));
#29047=CARTESIAN_POINT('Ctrl Pts',(-41.9132230489397,37.4592261840861,38.3229379119655));
#29048=CARTESIAN_POINT('Ctrl Pts',(-41.9188341484954,37.4656239868519,38.3270817949321));
#29049=CARTESIAN_POINT('Ctrl Pts',(-41.9244328339797,37.4720413162939,38.331212359266));
#29050=CARTESIAN_POINT('Ctrl Pts',(-41.9300190167042,37.4784780709492,38.3353295396313));
#29051=CARTESIAN_POINT('Ctrl Pts',(-41.9356051994287,37.4849148256045,38.3394467199965));
#29052=CARTESIAN_POINT('Ctrl Pts',(-41.9411788793932,37.4913710054729,38.3435505163928));
#29053=CARTESIAN_POINT('Ctrl Pts',(-41.9467399683006,37.4978465084832,38.3476408639029));
#29054=CARTESIAN_POINT('Ctrl Pts',(-41.952301057208,37.5043220114934,38.351731211413));
#29055=CARTESIAN_POINT('Ctrl Pts',(-41.9578495550581,37.5108168376451,38.3558081100369));
#29056=CARTESIAN_POINT('Ctrl Pts',(-41.9633853739478,37.5173308842615,38.3598714952779));
#29057=CARTESIAN_POINT('Ctrl Pts',(-41.9689211928374,37.523844930878,38.3639348805189));
#29058=CARTESIAN_POINT('Ctrl Pts',(-41.9744443327663,37.530378197959,38.3679847523771));
#29059=CARTESIAN_POINT('Ctrl Pts',(-41.9799547062282,37.5369305822254,38.3720210467789));
#29060=CARTESIAN_POINT('Ctrl Pts',(-41.98546507969,37.5434829664919,38.3760573411807));
#29061=CARTESIAN_POINT('Ctrl Pts',(-41.9909626866845,37.5500544679437,38.3800800581259));
#29062=CARTESIAN_POINT('Ctrl Pts',(-41.9964474401047,37.5566449827026,38.3840891339659));
#29063=CARTESIAN_POINT('Ctrl Pts',(-42.0019370680592,37.5632413547331,38.3881017728427));
#29064=CARTESIAN_POINT('Ctrl Pts',(-42.007413819582,37.5698567738815,38.3921007463564));
#29065=CARTESIAN_POINT('Ctrl Pts',(-42.0128776077367,37.5764911353951,38.3960859911166));
#29066=CARTESIAN_POINT('Ctrl Pts',(-41.7367328459062,37.2738705169503,38.1998157216697));
#29067=CARTESIAN_POINT('Ctrl Pts',(-41.7430280210025,37.2803585765446,38.2046103979808));
#29068=CARTESIAN_POINT('Ctrl Pts',(-41.7493097317734,37.2868706330318,38.209390280178));
#29069=CARTESIAN_POINT('Ctrl Pts',(-41.7555778617687,37.293406565812,38.214155279829));
#29070=CARTESIAN_POINT('Ctrl Pts',(-41.761845991764,37.2999424985921,38.21892027948));
#29071=CARTESIAN_POINT('Ctrl Pts',(-41.7681005409835,37.3065023076648,38.2236703965848));
#29072=CARTESIAN_POINT('Ctrl Pts',(-41.7743413934729,37.3130858715579,38.2284055432544));
#29073=CARTESIAN_POINT('Ctrl Pts',(-41.7805822459624,37.319669435451,38.2331406899241));
#29074=CARTESIAN_POINT('Ctrl Pts',(-41.7868094017216,37.3262767541642,38.2378608661586));
#29075=CARTESIAN_POINT('Ctrl Pts',(-41.7930227452966,37.3329077053572,38.2425659846159));
#29076=CARTESIAN_POINT('Ctrl Pts',(-41.7992360888717,37.3395386565503,38.2472711030733));
#29077=CARTESIAN_POINT('Ctrl Pts',(-41.8054356202623,37.3461932402229,38.2519611637533));
#29078=CARTESIAN_POINT('Ctrl Pts',(-41.8116212245189,37.3528713331714,38.256636079864));
#29079=CARTESIAN_POINT('Ctrl Pts',(-41.8178068287755,37.35954942612,38.2613109959747));
#29080=CARTESIAN_POINT('Ctrl Pts',(-41.8239785058979,37.3662510283441,38.2659707675158));
#29081=CARTESIAN_POINT('Ctrl Pts',(-41.8301361414449,37.3729760157812,38.2706153082483));
#29082=CARTESIAN_POINT('Ctrl Pts',(-41.8362937769919,37.3797010032182,38.2752598489809));
#29083=CARTESIAN_POINT('Ctrl Pts',(-41.8424373709633,37.3864493758679,38.2798891589046));
#29084=CARTESIAN_POINT('Ctrl Pts',(-41.8485668094307,37.3932210088127,38.2845031523365));
#29085=CARTESIAN_POINT('Ctrl Pts',(-41.8546962478981,37.3999926417575,38.2891171457685));
#29086=CARTESIAN_POINT('Ctrl Pts',(-41.8608115308611,37.4067875349973,38.2937158227084));
#29087=CARTESIAN_POINT('Ctrl Pts',(-41.866912544908,37.4136055627644,38.2982990980327));
#29088=CARTESIAN_POINT('Ctrl Pts',(-41.873013558955,37.4204235905314,38.3028823733569));
#29089=CARTESIAN_POINT('Ctrl Pts',(-41.8791003040856,37.4272647528256,38.3074502470652));
#29090=CARTESIAN_POINT('Ctrl Pts',(-41.8851726674089,37.4341289230337,38.3120026345959));
#29091=CARTESIAN_POINT('Ctrl Pts',(-41.8912450307322,37.4409930932418,38.3165550221266));
#29092=CARTESIAN_POINT('Ctrl Pts',(-41.897303012248,37.4478802713635,38.3210919234796));
#29093=CARTESIAN_POINT('Ctrl Pts',(-41.90334649959,37.4547903299445,38.3256132546585));
#29094=CARTESIAN_POINT('Ctrl Pts',(-41.9093899869321,37.4617003885256,38.3301345858374));
#29095=CARTESIAN_POINT('Ctrl Pts',(-41.9154189801002,37.4686333275657,38.3346403468421));
#29096=CARTESIAN_POINT('Ctrl Pts',(-41.9214333672572,37.4755890187741,38.3391304542444));
#29097=CARTESIAN_POINT('Ctrl Pts',(-41.9274477544141,37.4825447099826,38.3436205616467));
#29098=CARTESIAN_POINT('Ctrl Pts',(-41.9334475355597,37.489523153359,38.3480950154465));
#29099=CARTESIAN_POINT('Ctrl Pts',(-41.9394325993895,37.4965242197808,38.352553732787));
#29100=CARTESIAN_POINT('Ctrl Pts',(-41.9454176632194,37.5035252862025,38.3570124501275));
#29101=CARTESIAN_POINT('Ctrl Pts',(-41.9513880097333,37.5105489756694,38.3614554310084));
#29102=CARTESIAN_POINT('Ctrl Pts',(-41.9573435281639,37.5175951582312,38.3658825931472));
#29103=CARTESIAN_POINT('Ctrl Pts',(-41.9632990465945,37.5246413407931,38.370309755286));
#29104=CARTESIAN_POINT('Ctrl Pts',(-41.9692397369415,37.5317100164498,38.3747210986826));
#29105=CARTESIAN_POINT('Ctrl Pts',(-41.9751654889785,37.5388010544286,38.3791165416315));
#29106=CARTESIAN_POINT('Ctrl Pts',(-41.9810912410156,37.5458920924075,38.3835119845804));
#29107=CARTESIAN_POINT('Ctrl Pts',(-41.9870020547423,37.5530054927082,38.3878915270814));
#29108=CARTESIAN_POINT('Ctrl Pts',(-41.9928978204773,37.5601411237404,38.3922550880094));
#29109=CARTESIAN_POINT('Ctrl Pts',(-41.9987935862122,37.5672767547726,38.3966186489373));
#29110=CARTESIAN_POINT('Ctrl Pts',(-42.0046743039551,37.5744346165359,38.400966228292));
#29111=CARTESIAN_POINT('Ctrl Pts',(-42.0105398645732,37.5816145766264,38.4052977455312));
#29112=CARTESIAN_POINT('Ctrl Pts',(-42.0164106381653,37.5888009178539,38.4096331123744));
#29113=CARTESIAN_POINT('Ctrl Pts',(-42.0222662276787,37.5960093967053,38.4139523885391));
#29114=CARTESIAN_POINT('Ctrl Pts',(-42.0281065242439,37.603239879613,38.4182554938557));
#29115=CARTESIAN_POINT('Ctrl Pts',(-41.7321871653721,37.2744646741203,38.2049165643793));
#29116=CARTESIAN_POINT('Ctrl Pts',(-41.7389170723941,37.2814374382853,38.21010180357));
#29117=CARTESIAN_POINT('Ctrl Pts',(-41.7456313608748,37.2884380387103,38.2152698816723));
#29118=CARTESIAN_POINT('Ctrl Pts',(-41.7523298848223,37.2954663231777,38.2204206863142));
#29119=CARTESIAN_POINT('Ctrl Pts',(-41.7590284087698,37.3024946076452,38.2255714909562));
#29120=CARTESIAN_POINT('Ctrl Pts',(-41.7657111681836,37.3095505761549,38.2307050221375));
#29121=CARTESIAN_POINT('Ctrl Pts',(-41.7723780177576,37.3166340752856,38.2358211682374));
#29122=CARTESIAN_POINT('Ctrl Pts',(-41.7790448673315,37.3237175744162,38.2409373143374));
#29123=CARTESIAN_POINT('Ctrl Pts',(-41.785695807065,37.3308286041674,38.2460360753556));
#29124=CARTESIAN_POINT('Ctrl Pts',(-41.7923306923437,37.3379670099207,38.2511173404274));
#29125=CARTESIAN_POINT('Ctrl Pts',(-41.7989655776225,37.345105415674,38.2561986054992));
#29126=CARTESIAN_POINT('Ctrl Pts',(-41.805584408446,37.352271197429,38.2612623746243));
#29127=CARTESIAN_POINT('Ctrl Pts',(-41.8121870408979,37.3594641993769,38.2663085376988));
#29128=CARTESIAN_POINT('Ctrl Pts',(-41.8187896733498,37.3666572013247,38.2713547007732));
#29129=CARTESIAN_POINT('Ctrl Pts',(-41.8253761074299,37.3738774234648,38.2763832577968));
#29130=CARTESIAN_POINT('Ctrl Pts',(-41.831946199926,37.3811247088047,38.2813940994311));
#29131=CARTESIAN_POINT('Ctrl Pts',(-41.8385162924222,37.3883719941445,38.2864049410656));
#29132=CARTESIAN_POINT('Ctrl Pts',(-41.8450700433342,37.3956463426837,38.2913980673105));
#29133=CARTESIAN_POINT('Ctrl Pts',(-41.8516073101607,37.4029475962526,38.2963733695981));
#29134=CARTESIAN_POINT('Ctrl Pts',(-41.8581445769872,37.4102488498215,38.3013486718857));
#29135=CARTESIAN_POINT('Ctrl Pts',(-41.8646653597278,37.4175770084196,38.3063061502157));
#29136=CARTESIAN_POINT('Ctrl Pts',(-41.8711695165982,37.4249319127075,38.3112456967953));
#29137=CARTESIAN_POINT('Ctrl Pts',(-41.8776736734685,37.4322868169954,38.3161852433749));
#29138=CARTESIAN_POINT('Ctrl Pts',(-41.8841612044682,37.4396684669727,38.3211068582038));
#29139=CARTESIAN_POINT('Ctrl Pts',(-41.8906319685359,37.4470767021365,38.3260104342692));
#29140=CARTESIAN_POINT('Ctrl Pts',(-41.8971027326035,37.4544849373004,38.3309140103344));
#29141=CARTESIAN_POINT('Ctrl Pts',(-41.9035567297387,37.4619197576506,38.3357995476358));
#29142=CARTESIAN_POINT('Ctrl Pts',(-41.9099938196092,37.4693810015281,38.3406669399448));
#29143=CARTESIAN_POINT('Ctrl Pts',(-41.9164309094797,37.4768422454057,38.3455343322538));
#29144=CARTESIAN_POINT('Ctrl Pts',(-41.9228510920851,37.4843299128102,38.35038357957));
#29145=CARTESIAN_POINT('Ctrl Pts',(-41.9292542278285,37.491843840934,38.3552145764541));
#29146=CARTESIAN_POINT('Ctrl Pts',(-41.9356573635717,37.4993577690579,38.3600455733381));
#29147=CARTESIAN_POINT('Ctrl Pts',(-41.9420434524526,37.5068979579004,38.3648583197898));
#29148=CARTESIAN_POINT('Ctrl Pts',(-41.9484123556152,37.5144642435118,38.3696527111632));
#29149=CARTESIAN_POINT('Ctrl Pts',(-41.9547812587779,37.5220305291232,38.3744471025367));
#29150=CARTESIAN_POINT('Ctrl Pts',(-41.961132976222,37.5296229115031,38.3792231388316));
#29151=CARTESIAN_POINT('Ctrl Pts',(-41.9674673698392,37.5372412255669,38.3839807162004));
#29152=CARTESIAN_POINT('Ctrl Pts',(-41.9738017634564,37.5448595396305,38.3887382935692));
#29153=CARTESIAN_POINT('Ctrl Pts',(-41.9801188332463,37.5525037853775,38.3934774120117));
#29154=CARTESIAN_POINT('Ctrl Pts',(-41.986418441854,37.5601737965954,38.3981979684829));
#29155=CARTESIAN_POINT('Ctrl Pts',(-41.9927180504617,37.5678438078133,38.4029185249541));
#29156=CARTESIAN_POINT('Ctrl Pts',(-41.9990001978867,37.5755395845017,38.4076205194538));
#29157=CARTESIAN_POINT('Ctrl Pts',(-42.0052647475334,37.5832609593277,38.4123038497444));
#29158=CARTESIAN_POINT('Ctrl Pts',(-42.0115292971802,37.5909823341538,38.416987180035));
#29159=CARTESIAN_POINT('Ctrl Pts',(-42.0177762490482,37.5987293071169,38.4216518461161));
#29160=CARTESIAN_POINT('Ctrl Pts',(-42.0240054673073,37.6065017097712,38.4262977465618));
#29161=CARTESIAN_POINT('Ctrl Pts',(-42.0302402217383,37.6142810200913,38.4309477760174));
#29162=CARTESIAN_POINT('Ctrl Pts',(-42.0364572110247,37.6220858053229,38.4355790064668));
#29163=CARTESIAN_POINT('Ctrl Pts',(-42.0426562997468,37.6299158954619,38.4401913370316));
#29164=CARTESIAN_POINT('Ctrl Pts',(-41.7276414848379,37.2750588312903,38.2100174070889));
#29165=CARTESIAN_POINT('Ctrl Pts',(-41.7348061237857,37.282516300026,38.2155932091592));
#29166=CARTESIAN_POINT('Ctrl Pts',(-41.7419529899762,37.2900054443886,38.2211494831666));
#29167=CARTESIAN_POINT('Ctrl Pts',(-41.7490819078759,37.2975260805435,38.2266860927995));
#29168=CARTESIAN_POINT('Ctrl Pts',(-41.7562108257756,37.3050467166984,38.2322227024323));
#29169=CARTESIAN_POINT('Ctrl Pts',(-41.7633217953838,37.312598844645,38.2377396476902));
#29170=CARTESIAN_POINT('Ctrl Pts',(-41.7704146420422,37.3201822790132,38.2432367932204));
#29171=CARTESIAN_POINT('Ctrl Pts',(-41.7775074887006,37.3277657133814,38.2487339387506));
#29172=CARTESIAN_POINT('Ctrl Pts',(-41.7845822124084,37.3353804541706,38.2542112845526));
#29173=CARTESIAN_POINT('Ctrl Pts',(-41.7916386393909,37.3430263144842,38.2596686962389));
#29174=CARTESIAN_POINT('Ctrl Pts',(-41.7986950663732,37.3506721747979,38.2651261079251));
#29175=CARTESIAN_POINT('Ctrl Pts',(-41.8057331966296,37.3583491546353,38.2705635854952));
#29176=CARTESIAN_POINT('Ctrl Pts',(-41.8127528572769,37.3660570655823,38.2759809955335));
#29177=CARTESIAN_POINT('Ctrl Pts',(-41.8197725179242,37.3737649765293,38.2813984055718));
#29178=CARTESIAN_POINT('Ctrl Pts',(-41.8267737089618,37.3815038185855,38.2867957480777));
#29179=CARTESIAN_POINT('Ctrl Pts',(-41.8337562584072,37.3892734018282,38.292172890614));
#29180=CARTESIAN_POINT('Ctrl Pts',(-41.8407388078525,37.3970429850708,38.2975500331503));
#29181=CARTESIAN_POINT('Ctrl Pts',(-41.847702715705,37.4048433094995,38.3029069757164));
#29182=CARTESIAN_POINT('Ctrl Pts',(-41.8546478108907,37.4126741836924,38.3082435868597));
#29183=CARTESIAN_POINT('Ctrl Pts',(-41.8615929060763,37.4205050578853,38.3135801980029));
#29184=CARTESIAN_POINT('Ctrl Pts',(-41.8685191885945,37.4283664818419,38.3188964777229));
#29185=CARTESIAN_POINT('Ctrl Pts',(-41.8754264882883,37.4362582626507,38.3241922955579));
#29186=CARTESIAN_POINT('Ctrl Pts',(-41.8823337879821,37.4441500434594,38.3294881133929));
#29187=CARTESIAN_POINT('Ctrl Pts',(-41.8892221048508,37.4520721811197,38.3347634693425));
#29188=CARTESIAN_POINT('Ctrl Pts',(-41.8960912696628,37.4600244812394,38.3400182339424));
#29189=CARTESIAN_POINT('Ctrl Pts',(-41.9029604344748,37.4679767813591,38.3452729985423));
#29190=CARTESIAN_POINT('Ctrl Pts',(-41.9098104472295,37.4759592439376,38.3505071717921));
#29191=CARTESIAN_POINT('Ctrl Pts',(-41.9166411396284,37.4839716731117,38.3557206252311));
#29192=CARTESIAN_POINT('Ctrl Pts',(-41.9234718320273,37.4919841022858,38.3609340786701));
#29193=CARTESIAN_POINT('Ctrl Pts',(-41.93028320407,37.5000264980549,38.3661268122979));
#29194=CARTESIAN_POINT('Ctrl Pts',(-41.9370750883997,37.508098663094,38.3712986986637));
#29195=CARTESIAN_POINT('Ctrl Pts',(-41.9438669727293,37.5161708281332,38.3764705850296));
#29196=CARTESIAN_POINT('Ctrl Pts',(-41.9506393693455,37.5242727624417,38.3816216241331));
#29197=CARTESIAN_POINT('Ctrl Pts',(-41.9573921118409,37.5324042672428,38.3867516895395));
#29198=CARTESIAN_POINT('Ctrl Pts',(-41.9641448543364,37.5405357720439,38.3918817549459));
#29199=CARTESIAN_POINT('Ctrl Pts',(-41.9708779427107,37.548696847337,38.3969908466547));
#29200=CARTESIAN_POINT('Ctrl Pts',(-41.9775912115145,37.5568872929024,38.4020788392536));
#29201=CARTESIAN_POINT('Ctrl Pts',(-41.9843044803183,37.5650777384679,38.4071668318524));
#29202=CARTESIAN_POINT('Ctrl Pts',(-41.9909979295511,37.5732975543052,38.4122337253407));
#29203=CARTESIAN_POINT('Ctrl Pts',(-41.9976713947294,37.5815465387622,38.4172793953343));
#29204=CARTESIAN_POINT('Ctrl Pts',(-42.0043448599078,37.5897955232191,38.4223250653279));
#29205=CARTESIAN_POINT('Ctrl Pts',(-42.010998341031,37.5980736762952,38.4273495118262));
#29206=CARTESIAN_POINT('Ctrl Pts',(-42.0176316745896,37.606380794915,38.4323526114794));
#29207=CARTESIAN_POINT('Ctrl Pts',(-42.0242650081481,37.6146879135349,38.4373557111327));
#29208=CARTESIAN_POINT('Ctrl Pts',(-42.0308781941414,37.6230239976979,38.4423374639403));
#29209=CARTESIAN_POINT('Ctrl Pts',(-42.0374710700414,37.6313888429159,38.4472977475925));
#29210=CARTESIAN_POINT('Ctrl Pts',(-42.0440698053114,37.6397611223286,38.4522624396604));
#29211=CARTESIAN_POINT('Ctrl Pts',(-42.0506481943707,37.6481622139406,38.4572056243945));
#29212=CARTESIAN_POINT('Ctrl Pts',(-42.0572060752497,37.6565919113109,38.4621271802075));
#29213=CARTESIAN_POINT('Ctrl Pts',(-41.7230729915867,37.275626356627,38.2150958136178));
#29214=CARTESIAN_POINT('Ctrl Pts',(-41.7306622893052,37.2835625164353,38.2210615920481));
#29215=CARTESIAN_POINT('Ctrl Pts',(-41.7382314646438,37.2915345395025,38.2270052607349));
#29216=CARTESIAN_POINT('Ctrl Pts',(-41.7457803069961,37.299542204158,38.2329266545113));
#29217=CARTESIAN_POINT('Ctrl Pts',(-41.7533291493484,37.3075498688135,38.2388480482876));
#29218=CARTESIAN_POINT('Ctrl Pts',(-41.7608576587077,37.3155931750479,38.2447471671446));
#29219=CARTESIAN_POINT('Ctrl Pts',(-41.7683656255999,37.3236718992408,38.2506238471586));
#29220=CARTESIAN_POINT('Ctrl Pts',(-41.7758735924921,37.3317506234335,38.2565005271726));
#29221=CARTESIAN_POINT('Ctrl Pts',(-41.7833610169126,37.3398647655783,38.2623547683379));
#29222=CARTESIAN_POINT('Ctrl Pts',(-41.790827690507,37.3480141000814,38.2681864079499));
#29223=CARTESIAN_POINT('Ctrl Pts',(-41.7982943641013,37.3561634345845,38.2740180475619));
#29224=CARTESIAN_POINT('Ctrl Pts',(-41.8057402868683,37.3643479614441,38.2798270856192));
#29225=CARTESIAN_POINT('Ctrl Pts',(-41.8131652516029,37.3725674531331,38.2856133606714));
#29226=CARTESIAN_POINT('Ctrl Pts',(-41.8205902163375,37.3807869448222,38.2913996357236));
#29227=CARTESIAN_POINT('Ctrl Pts',(-41.8279942230375,37.3890414013376,38.297163147768));
#29228=CARTESIAN_POINT('Ctrl Pts',(-41.8353770656508,37.3973305932187,38.3029037366049));
#29229=CARTESIAN_POINT('Ctrl Pts',(-41.842759908264,37.4056197850998,38.3086443254418));
#29230=CARTESIAN_POINT('Ctrl Pts',(-41.8501215867896,37.4139437123456,38.3143619910705));
#29231=CARTESIAN_POINT('Ctrl Pts',(-41.8574618963422,37.4223021435787,38.3200565745555));
#29232=CARTESIAN_POINT('Ctrl Pts',(-41.8648022058947,37.4306605748119,38.3257511580404));
#29233=CARTESIAN_POINT('Ctrl Pts',(-41.8721211464735,37.4390535100316,38.3314226593808));
#29234=CARTESIAN_POINT('Ctrl Pts',(-41.8794185143709,37.4474807159566,38.3370709209135));
#29235=CARTESIAN_POINT('Ctrl Pts',(-41.8867158822685,37.4559079218816,38.3427191824463));
#29236=CARTESIAN_POINT('Ctrl Pts',(-41.893991677484,37.464369398511,38.3483442041708));
#29237=CARTESIAN_POINT('Ctrl Pts',(-41.9012456974993,37.4728649106725,38.3539458297051));
#29238=CARTESIAN_POINT('Ctrl Pts',(-41.9084997175147,37.481360422834,38.3595474552394));
#29239=CARTESIAN_POINT('Ctrl Pts',(-41.9157319623291,37.4898899705267,38.3651256845829));
#29240=CARTESIAN_POINT('Ctrl Pts',(-41.9229422306246,37.4984533167,38.3706803626433));
#29241=CARTESIAN_POINT('Ctrl Pts',(-41.9301524989203,37.5070166628732,38.3762350407038));
#29242=CARTESIAN_POINT('Ctrl Pts',(-41.9373407906963,37.5156138075261,38.3817661674807));
#29243=CARTESIAN_POINT('Ctrl Pts',(-41.9445069058461,37.5242445117427,38.38727358918));
#29244=CARTESIAN_POINT('Ctrl Pts',(-41.9516730209959,37.5328752159593,38.3927810108792));
#29245=CARTESIAN_POINT('Ctrl Pts',(-41.9588169595188,37.5415394797386,38.3982647275003));
#29246=CARTESIAN_POINT('Ctrl Pts',(-41.9659385225304,37.5502370623123,38.4037245865559));
#29247=CARTESIAN_POINT('Ctrl Pts',(-41.9730600855419,37.5589346448861,38.4091844456114));
#29248=CARTESIAN_POINT('Ctrl Pts',(-41.9801592730415,37.5676655462534,38.4146204471008));
#29249=CARTESIAN_POINT('Ctrl Pts',(-41.9872358873777,37.5764295238067,38.4200324398517));
#29250=CARTESIAN_POINT('Ctrl Pts',(-41.994312501714,37.5851935013599,38.4254444326026));
#29251=CARTESIAN_POINT('Ctrl Pts',(-42.0013665428862,37.5939905550983,38.4308324166144));
#29252=CARTESIAN_POINT('Ctrl Pts',(-42.0083978144872,37.6028204405884,38.4361962420379));
#29253=CARTESIAN_POINT('Ctrl Pts',(-42.0154290860881,37.6116503260784,38.4415600674614));
#29254=CARTESIAN_POINT('Ctrl Pts',(-42.0224375881171,37.6205130433192,38.446899734296));
#29255=CARTESIAN_POINT('Ctrl Pts',(-42.0294231254213,37.6294083460648,38.4522150940239));
#29256=CARTESIAN_POINT('Ctrl Pts',(-42.0364086627255,37.6383036488102,38.4575304537519));
#29257=CARTESIAN_POINT('Ctrl Pts',(-42.0433712353044,37.6472315370596,38.4628215063726));
#29258=CARTESIAN_POINT('Ctrl Pts',(-42.0503106492707,37.6561917627675,38.4680881047078));
#29259=CARTESIAN_POINT('Ctrl Pts',(-42.0572562305902,37.6651599518102,38.4733593836936));
#29260=CARTESIAN_POINT('Ctrl Pts',(-42.0641786121495,37.6741605358844,38.4786061649633));
#29261=CARTESIAN_POINT('Ctrl Pts',(-42.0710776007528,37.6831932643562,38.4838283021851));
#29262=CARTESIAN_POINT('Ctrl Pts',(-41.7184851250818,37.2761712654004,38.2201551666592));
#29263=CARTESIAN_POINT('Ctrl Pts',(-41.7264872714304,37.2845766395827,38.2265062982766));
#29264=CARTESIAN_POINT('Ctrl Pts',(-41.7344667883464,37.2930223452366,38.2328325654919));
#29265=CARTESIAN_POINT('Ctrl Pts',(-41.7424234244465,37.3015081162923,38.239133769005));
#29266=CARTESIAN_POINT('Ctrl Pts',(-41.7503800605466,37.3099938873479,38.2454349725181));
#29267=CARTESIAN_POINT('Ctrl Pts',(-41.7583138158242,37.3185197237962,38.2517111123206));
#29268=CARTESIAN_POINT('Ctrl Pts',(-41.7662244403479,37.3270853570574,38.2579619907056));
#29269=CARTESIAN_POINT('Ctrl Pts',(-41.7741350648715,37.3356509903186,38.2642128690906));
#29270=CARTESIAN_POINT('Ctrl Pts',(-41.7820225586366,37.3442564203866,38.2704384860526));
#29271=CARTESIAN_POINT('Ctrl Pts',(-41.7898866731567,37.3529013761564,38.2766386454592));
#29272=CARTESIAN_POINT('Ctrl Pts',(-41.7977507876768,37.3615463319261,38.2828388048658));
#29273=CARTESIAN_POINT('Ctrl Pts',(-41.8055915229504,37.3702308133956,38.2890135067153));
#29274=CARTESIAN_POINT('Ctrl Pts',(-41.8134086319691,37.378954546977,38.2951625564871));
#29275=CARTESIAN_POINT('Ctrl Pts',(-41.8212257409878,37.3876782805585,38.3013116062587));
#29276=CARTESIAN_POINT('Ctrl Pts',(-41.8290192237492,37.3964412662486,38.3074350039495));
#29277=CARTESIAN_POINT('Ctrl Pts',(-41.8367888347307,37.4052432279819,38.3135325566508));
#29278=CARTESIAN_POINT('Ctrl Pts',(-41.8445584457122,37.4140451897154,38.319630109352));
#29279=CARTESIAN_POINT('Ctrl Pts',(-41.8523041849128,37.4228861274909,38.3257018170627));
#29280=CARTESIAN_POINT('Ctrl Pts',(-41.860025808314,37.4317657627873,38.3317474885023));
#29281=CARTESIAN_POINT('Ctrl Pts',(-41.8677474317152,37.4406453980838,38.337793159942));
#29282=CARTESIAN_POINT('Ctrl Pts',(-41.875444939316,37.4495637309,38.3438127951099));
#29283=CARTESIAN_POINT('Ctrl Pts',(-41.8831180886173,37.4585204802766,38.3498062043658));
#29284=CARTESIAN_POINT('Ctrl Pts',(-41.8907912379186,37.4674772296532,38.3557996136218));
#29285=CARTESIAN_POINT('Ctrl Pts',(-41.8984400289194,37.476472395589,38.361766796965));
#29286=CARTESIAN_POINT('Ctrl Pts',(-41.9060642206555,37.485505694704,38.367707566408));
#29287=CARTESIAN_POINT('Ctrl Pts',(-41.9136884123916,37.494538993819,38.373648335851));
#29288=CARTESIAN_POINT('Ctrl Pts',(-41.9212880048618,37.5036104261121,38.3795626913929));
#29289=CARTESIAN_POINT('Ctrl Pts',(-41.928862758652,37.5127197058007,38.3854504467104));
#29290=CARTESIAN_POINT('Ctrl Pts',(-41.9364375124421,37.5218289854894,38.3913382020278));
#29291=CARTESIAN_POINT('Ctrl Pts',(-41.9439874275511,37.5309761125723,38.39719935712));
#29292=CARTESIAN_POINT('Ctrl Pts',(-41.9515122661296,37.5401607988822,38.4030337273397));
#29293=CARTESIAN_POINT('Ctrl Pts',(-41.9590371047082,37.5493454851921,38.4088680975593));
#29294=CARTESIAN_POINT('Ctrl Pts',(-41.9665368667552,37.5585677307279,38.4146756829056));
#29295=CARTESIAN_POINT('Ctrl Pts',(-41.9740113160014,37.5678272449558,38.4204563004188));
#29296=CARTESIAN_POINT('Ctrl Pts',(-41.9814857652477,37.5770867591837,38.426236917932));
#29297=CARTESIAN_POINT('Ctrl Pts',(-41.9889349016921,37.5863835421024,38.4319905676113));
#29298=CARTESIAN_POINT('Ctrl Pts',(-41.9963584906603,37.5957173008301,38.4377170681963));
#29299=CARTESIAN_POINT('Ctrl Pts',(-42.0037820796284,37.6050510595578,38.4434435687812));
#29300=CARTESIAN_POINT('Ctrl Pts',(-42.0111801211193,37.6144217940933,38.449142920271));
#29301=CARTESIAN_POINT('Ctrl Pts',(-42.0185523820682,37.6238292092247,38.4548149431157));
#29302=CARTESIAN_POINT('Ctrl Pts',(-42.0259246430171,37.6332366243561,38.4604869659604));
#29303=CARTESIAN_POINT('Ctrl Pts',(-42.033271123423,37.6426807200824,38.4661316601591));
#29304=CARTESIAN_POINT('Ctrl Pts',(-42.0405915918455,37.6521611988806,38.471748847884));
#29305=CARTESIAN_POINT('Ctrl Pts',(-42.0479120602679,37.6616416776789,38.4773660356088));
#29306=CARTESIAN_POINT('Ctrl Pts',(-42.055206516706,37.6711585395479,38.482955716859));
#29307=CARTESIAN_POINT('Ctrl Pts',(-42.0624747313583,37.6807114846723,38.4885177155396));
#29308=CARTESIAN_POINT('Ctrl Pts',(-42.0697494055828,37.6902729199067,38.4940846574055));
#29309=CARTESIAN_POINT('Ctrl Pts',(-42.0769977913877,37.6998705026253,38.499623867526));
#29310=CARTESIAN_POINT('Ctrl Pts',(-42.084219659952,37.7095039298065,38.5051351709817));
#29311=CARTESIAN_POINT('Ctrl Pts',(-41.7138972585769,37.2767161741738,38.2252145197005));
#29312=CARTESIAN_POINT('Ctrl Pts',(-41.7223122535556,37.2855907627301,38.2319510045052));
#29313=CARTESIAN_POINT('Ctrl Pts',(-41.730702112049,37.2945101509708,38.2386598702489));
#29314=CARTESIAN_POINT('Ctrl Pts',(-41.7390665418968,37.3034740284267,38.2453408834987));
#29315=CARTESIAN_POINT('Ctrl Pts',(-41.7474309717446,37.3124379058824,38.2520218967486));
#29316=CARTESIAN_POINT('Ctrl Pts',(-41.7557699729406,37.3214462725444,38.2586750574966));
#29317=CARTESIAN_POINT('Ctrl Pts',(-41.7640832550958,37.3304988148741,38.2653001342526));
#29318=CARTESIAN_POINT('Ctrl Pts',(-41.7723965372509,37.3395513572038,38.2719252110086));
#29319=CARTESIAN_POINT('Ctrl Pts',(-41.7806841003605,37.3486480751949,38.2785222037673));
#29320=CARTESIAN_POINT('Ctrl Pts',(-41.7889456558064,37.3577886522314,38.2850908829684));
#29321=CARTESIAN_POINT('Ctrl Pts',(-41.7972072112522,37.3669292292677,38.2916595621696));
#29322=CARTESIAN_POINT('Ctrl Pts',(-41.8054427590326,37.3761136653472,38.2981999278115));
#29323=CARTESIAN_POINT('Ctrl Pts',(-41.8136520123354,37.3853416408209,38.3047117523027));
#29324=CARTESIAN_POINT('Ctrl Pts',(-41.8218612656381,37.3945696162947,38.3112235767938));
#29325=CARTESIAN_POINT('Ctrl Pts',(-41.8300442244608,37.4038411311594,38.3177068601312));
#29326=CARTESIAN_POINT('Ctrl Pts',(-41.8382006038106,37.4131558627451,38.3241613766967));
#29327=CARTESIAN_POINT('Ctrl Pts',(-41.8463569831605,37.4224705943309,38.3306158932622));
#29328=CARTESIAN_POINT('Ctrl Pts',(-41.8544867830361,37.4318285426362,38.3370416430548));
#29329=CARTESIAN_POINT('Ctrl Pts',(-41.8625897202859,37.4412293819959,38.3434384024493));
#29330=CARTESIAN_POINT('Ctrl Pts',(-41.8706926575358,37.4506302213557,38.3498351618437));
#29331=CARTESIAN_POINT('Ctrl Pts',(-41.8787687321586,37.4600739517684,38.3562029308389));
#29332=CARTESIAN_POINT('Ctrl Pts',(-41.8868176628637,37.4695602445966,38.3625414878181));
#29333=CARTESIAN_POINT('Ctrl Pts',(-41.8948665935688,37.4790465374248,38.3688800447972));
#29334=CARTESIAN_POINT('Ctrl Pts',(-41.9028883803549,37.488575392667,38.3751893897593));
#29335=CARTESIAN_POINT('Ctrl Pts',(-41.9108827438117,37.4981464787355,38.381469303111));
#29336=CARTESIAN_POINT('Ctrl Pts',(-41.9188771072685,37.507717564804,38.3877492164627));
#29337=CARTESIAN_POINT('Ctrl Pts',(-41.9268440473946,37.5173308816975,38.393999698203));
#29338=CARTESIAN_POINT('Ctrl Pts',(-41.9347832866793,37.5269860949015,38.4002205307774));
#29339=CARTESIAN_POINT('Ctrl Pts',(-41.942722525964,37.5366413081055,38.4064413633518));
#29340=CARTESIAN_POINT('Ctrl Pts',(-41.950634064406,37.5463384176184,38.4126325467594));
#29341=CARTESIAN_POINT('Ctrl Pts',(-41.9585176264132,37.5560770860217,38.4187938654994));
#29342=CARTESIAN_POINT('Ctrl Pts',(-41.9664011884204,37.565815754425,38.4249551842394));
#29343=CARTESIAN_POINT('Ctrl Pts',(-41.9742567739916,37.5755959817172,38.4310866383109));
#29344=CARTESIAN_POINT('Ctrl Pts',(-41.9820841094725,37.5854174275992,38.4371880142817));
#29345=CARTESIAN_POINT('Ctrl Pts',(-41.9899114449534,37.5952388734812,38.4432893902526));
#29346=CARTESIAN_POINT('Ctrl Pts',(-41.9977105303427,37.6051015379515,38.4493606881218));
#29347=CARTESIAN_POINT('Ctrl Pts',(-42.0054810939427,37.6150050778536,38.4554016965408));
#29348=CARTESIAN_POINT('Ctrl Pts',(-42.0132516575428,37.6249086177557,38.4614427049598));
#29349=CARTESIAN_POINT('Ctrl Pts',(-42.0209936993524,37.6348530330882,38.4674534239276));
#29350=CARTESIAN_POINT('Ctrl Pts',(-42.0287069496492,37.644837977861,38.4734336441935));
#29351=CARTESIAN_POINT('Ctrl Pts',(-42.0364201999461,37.6548229226339,38.4794138644593));
#29352=CARTESIAN_POINT('Ctrl Pts',(-42.044104658729,37.6648483968455,38.4853635860223));
#29353=CARTESIAN_POINT('Ctrl Pts',(-42.0517600582697,37.6749140516966,38.491282601744));
#29354=CARTESIAN_POINT('Ctrl Pts',(-42.0594154578104,37.6849797065475,38.4972016174658));
#29355=CARTESIAN_POINT('Ctrl Pts',(-42.0670417981077,37.6950855420361,38.5030899273454));
#29356=CARTESIAN_POINT('Ctrl Pts',(-42.0746388134458,37.7052312065772,38.5089473263713));
#29357=CARTESIAN_POINT('Ctrl Pts',(-42.0822425805756,37.7153858880031,38.5148099311175));
#29358=CARTESIAN_POINT('Ctrl Pts',(-42.0898169706259,37.725580469366,38.5206415700889));
#29359=CARTESIAN_POINT('Ctrl Pts',(-42.0973617191512,37.7358145952567,38.5264420397782));
#29360=CARTESIAN_POINT('Ctrl Pts',(-41.7092900287824,37.2772384780159,38.2302548290539));
#29361=CARTESIAN_POINT('Ctrl Pts',(-41.7181061010845,37.2865728382894,38.2373720637469));
#29362=CARTESIAN_POINT('Ctrl Pts',(-41.7268943728444,37.2959567462818,38.2444587522097));
#29363=CARTESIAN_POINT('Ctrl Pts',(-41.7356545054327,37.3053898405726,38.2515146216083));
#29364=CARTESIAN_POINT('Ctrl Pts',(-41.7444146380209,37.3148229348634,38.2585704910069));
#29365=CARTESIAN_POINT('Ctrl Pts',(-41.7531466314358,37.3243052154509,38.2655955413399));
#29366=CARTESIAN_POINT('Ctrl Pts',(-41.7618501492037,37.3338363171455,38.2725895021348));
#29367=CARTESIAN_POINT('Ctrl Pts',(-41.7705536669717,37.3433674188402,38.2795834629297));
#29368=CARTESIAN_POINT('Ctrl Pts',(-41.7792287090911,37.35294734164,38.2865463341851));
#29369=CARTESIAN_POINT('Ctrl Pts',(-41.7878749412702,37.3625757166143,38.2934778478106));
#29370=CARTESIAN_POINT('Ctrl Pts',(-41.7965211734494,37.3722040915885,38.3004093614361));
#29371=CARTESIAN_POINT('Ctrl Pts',(-41.8051385956866,37.3818809187351,38.3073095174303));
#29372=CARTESIAN_POINT('Ctrl Pts',(-41.8137268758974,37.39160582541,38.3141780501053));
#29373=CARTESIAN_POINT('Ctrl Pts',(-41.8223151561082,37.4013307320849,38.3210465827803));
#29374=CARTESIAN_POINT('Ctrl Pts',(-41.8308742942908,37.4111037182862,38.3278834921346));
#29375=CARTESIAN_POINT('Ctrl Pts',(-41.8394039605935,37.4209244076846,38.3346885149031));
#29376=CARTESIAN_POINT('Ctrl Pts',(-41.8479336268961,37.4307450970831,38.3414935376716));
#29377=CARTESIAN_POINT('Ctrl Pts',(-41.8564338213171,37.4406134896769,38.3482666738529));
#29378=CARTESIAN_POINT('Ctrl Pts',(-41.8649042162621,37.4505292054806,38.3550076626245));
#29379=CARTESIAN_POINT('Ctrl Pts',(-41.8733746112071,37.4604449212843,38.361748651396));
#29380=CARTESIAN_POINT('Ctrl Pts',(-41.8818152066744,37.4704079602961,38.3684574927564));
#29381=CARTESIAN_POINT('Ctrl Pts',(-41.8902256773526,37.4804179389031,38.3751339283459));
#29382=CARTESIAN_POINT('Ctrl Pts',(-41.8986361480308,37.4904279175102,38.3818103639354));
#29383=CARTESIAN_POINT('Ctrl Pts',(-41.9070164939181,37.5004848357108,38.3884543937525));
#29384=CARTESIAN_POINT('Ctrl Pts',(-41.9153663920104,37.5105883062938,38.3950657619197));
#29385=CARTESIAN_POINT('Ctrl Pts',(-41.9237162901027,37.520691776877,38.401677130087));
#29386=CARTESIAN_POINT('Ctrl Pts',(-41.9320357409245,37.530841800794,38.4082558374545));
#29387=CARTESIAN_POINT('Ctrl Pts',(-41.9403244227673,37.5410379853954,38.4148016289715));
#29388=CARTESIAN_POINT('Ctrl Pts',(-41.9486131046101,37.5512341699968,38.4213474204885));
#29389=CARTESIAN_POINT('Ctrl Pts',(-41.9568710179807,37.5614765161947,38.4278602969742));
#29390=CARTESIAN_POINT('Ctrl Pts',(-41.9650978445669,37.5717646296768,38.4343400075791));
#29391=CARTESIAN_POINT('Ctrl Pts',(-41.9733246711531,37.5820527431589,38.4408197181839));
#29392=CARTESIAN_POINT('Ctrl Pts',(-41.9815204109533,37.5923866239237,38.447266262907));
#29393=CARTESIAN_POINT('Ctrl Pts',(-41.9896847480295,37.6027658741374,38.453679393428));
#29394=CARTESIAN_POINT('Ctrl Pts',(-41.9978490851056,37.6131451243512,38.4600925239489));
#29395=CARTESIAN_POINT('Ctrl Pts',(-42.0059820194561,37.6235697440116,38.4664722402663));
#29396=CARTESIAN_POINT('Ctrl Pts',(-42.0140832375544,37.6340393318199,38.4728182966305));
#29397=CARTESIAN_POINT('Ctrl Pts',(-42.0221844556527,37.6445089196283,38.4791643529947));
#29398=CARTESIAN_POINT('Ctrl Pts',(-42.0302539574975,37.6550234755828,38.4854767494049));
#29399=CARTESIAN_POINT('Ctrl Pts',(-42.038291431984,37.6655825949225,38.4917552426768));
#29400=CARTESIAN_POINT('Ctrl Pts',(-42.0463289064706,37.6761417142622,38.4980337359487));
#29401=CARTESIAN_POINT('Ctrl Pts',(-42.0543343535991,37.6867453969885,38.5042783260844));
#29402=CARTESIAN_POINT('Ctrl Pts',(-42.0623074647211,37.6973932349308,38.5104887725025));
#29403=CARTESIAN_POINT('Ctrl Pts',(-42.070280575843,37.7080410728731,38.5166992189205));
#29404=CARTESIAN_POINT('Ctrl Pts',(-42.0782213509548,37.7187330660247,38.5228755216161));
#29405=CARTESIAN_POINT('Ctrl Pts',(-42.0861294838881,37.7294688028375,38.5290174426298));
#29406=CARTESIAN_POINT('Ctrl Pts',(-42.0940446451165,37.7402140809574,38.5351648222307));
#29407=CARTESIAN_POINT('Ctrl Pts',(-42.1019271052873,37.7510031787688,38.5412777575933));
#29408=CARTESIAN_POINT('Ctrl Pts',(-42.1097765615633,37.7618356837186,38.5473560155564));
#29409=CARTESIAN_POINT('Ctrl Pts',(-41.7046664632442,37.2777417113195,38.2352790722939));
#29410=CARTESIAN_POINT('Ctrl Pts',(-41.7138715660119,37.2875248501967,38.242770189431));
#29411=CARTESIAN_POINT('Ctrl Pts',(-41.7230460825938,37.2973625015263,38.2502276995733));
#29412=CARTESIAN_POINT('Ctrl Pts',(-41.7321896223355,37.3072542464174,38.2576512851773));
#29413=CARTESIAN_POINT('Ctrl Pts',(-41.7413331620773,37.3171459913084,38.2650748707813));
#29414=CARTESIAN_POINT('Ctrl Pts',(-41.7504457249767,37.3270918297587,38.2724645318453));
#29415=CARTESIAN_POINT('Ctrl Pts',(-41.7595269230176,37.3370913382707,38.2798199537147));
#29416=CARTESIAN_POINT('Ctrl Pts',(-41.7686081210585,37.3470908467828,38.2871753755842));
#29417=CARTESIAN_POINT('Ctrl Pts',(-41.7776579542388,37.3571440253542,38.2944965582575));
#29418=CARTESIAN_POINT('Ctrl Pts',(-41.7866760372132,37.3672504459171,38.3017831899959));
#29419=CARTESIAN_POINT('Ctrl Pts',(-41.7956941201876,37.37735686648,38.3090698217343));
#29420=CARTESIAN_POINT('Ctrl Pts',(-41.8046804529541,37.3875165290319,38.3163219025361));
#29421=CARTESIAN_POINT('Ctrl Pts',(-41.8136346528712,37.3977290009708,38.3235391236051));
#29422=CARTESIAN_POINT('Ctrl Pts',(-41.8225888527884,37.4079414729097,38.3307563446742));
#29423=CARTESIAN_POINT('Ctrl Pts',(-41.8315109198541,37.4182067542331,38.3379387060087));
#29424=CARTESIAN_POINT('Ctrl Pts',(-41.8404004741637,37.4285244078417,38.3450859017813));
#29425=CARTESIAN_POINT('Ctrl Pts',(-41.8492900284732,37.4388420614502,38.3522330975538));
#29426=CARTESIAN_POINT('Ctrl Pts',(-41.8581470700244,37.4492120873415,38.3593451277626));
#29427=CARTESIAN_POINT('Ctrl Pts',(-41.8669712216812,37.4596340439559,38.3664216895748));
#29428=CARTESIAN_POINT('Ctrl Pts',(-41.875795373338,37.4700560005704,38.3734982513871));
#29429=CARTESIAN_POINT('Ctrl Pts',(-41.8845866350983,37.4805298879057,38.380539344801));
#29430=CARTESIAN_POINT('Ctrl Pts',(-41.8933446326271,37.4910552599798,38.3875446700045));
#29431=CARTESIAN_POINT('Ctrl Pts',(-41.9021026301559,37.5015806320539,38.394549995208));
#29432=CARTESIAN_POINT('Ctrl Pts',(-41.910827363451,37.5121574888643,38.4015195521993));
#29433=CARTESIAN_POINT('Ctrl Pts',(-41.9195184610102,37.5227853800447,38.4084530442122));
#29434=CARTESIAN_POINT('Ctrl Pts',(-41.9282095585694,37.5334132712252,38.415386536225));
#29435=CARTESIAN_POINT('Ctrl Pts',(-41.9368670208726,37.5440921976628,38.4222839640525));
#29436=CARTESIAN_POINT('Ctrl Pts',(-41.9454904783322,37.5548217028996,38.4291450324364));
#29437=CARTESIAN_POINT('Ctrl Pts',(-41.9541139357918,37.5655512081365,38.4360061008203));
#29438=CARTESIAN_POINT('Ctrl Pts',(-41.9627033888718,37.5763312930231,38.4428308105248));
#29439=CARTESIAN_POINT('Ctrl Pts',(-41.9712584718331,37.5871614985452,38.4496188709562));
#29440=CARTESIAN_POINT('Ctrl Pts',(-41.9798135547945,37.5979917040673,38.4564069313877));
#29441=CARTESIAN_POINT('Ctrl Pts',(-41.9883342676352,37.6088720302228,38.4631583425448));
#29442=CARTESIAN_POINT('Ctrl Pts',(-41.9968202475373,37.6198020137172,38.4698728169447));
#29443=CARTESIAN_POINT('Ctrl Pts',(-42.0053062274393,37.6307319972116,38.4765872913445));
#29444=CARTESIAN_POINT('Ctrl Pts',(-42.0137574744005,37.6417116380421,38.4832648289854));
#29445=CARTESIAN_POINT('Ctrl Pts',(-42.022173628567,37.6527404686982,38.4899051455408));
#29446=CARTESIAN_POINT('Ctrl Pts',(-42.0305897827335,37.6637692993541,38.4965454620962));
#29447=CARTESIAN_POINT('Ctrl Pts',(-42.0389708441033,37.6748473198335,38.5031485575649));
#29448=CARTESIAN_POINT('Ctrl Pts',(-42.0473164558045,37.6859740584228,38.5097141507787));
#29449=CARTESIAN_POINT('Ctrl Pts',(-42.0556620675058,37.6971007970122,38.5162797439925));
#29450=CARTESIAN_POINT('Ctrl Pts',(-42.063972229538,37.7082762537124,38.5228078349527));
#29451=CARTESIAN_POINT('Ctrl Pts',(-42.0722465880516,37.7194999526687,38.529298145691));
#29452=CARTESIAN_POINT('Ctrl Pts',(-42.0805209465652,37.7307236516249,38.5357884564294));
#29453=CARTESIAN_POINT('Ctrl Pts',(-42.0887595015562,37.7419955928303,38.5422409869407));
#29454=CARTESIAN_POINT('Ctrl Pts',(-42.0969619022279,37.7533152963297,38.5486554624809));
#29455=CARTESIAN_POINT('Ctrl Pts',(-42.105171592723,37.7646450601323,38.5550756388391));
#29456=CARTESIAN_POINT('Ctrl Pts',(-42.1133450638489,37.7760226695206,38.5614576912358));
#29457=CARTESIAN_POINT('Ctrl Pts',(-42.1214819684532,37.7874476424097,38.5678013500418));
#29458=CARTESIAN_POINT('Ctrl Pts',(-41.700042897706,37.278244944623,38.2403033155339));
#29459=CARTESIAN_POINT('Ctrl Pts',(-41.7096370309394,37.288476862104,38.2481683151151));
#29460=CARTESIAN_POINT('Ctrl Pts',(-41.7191977923432,37.2987682567707,38.2559966469369));
#29461=CARTESIAN_POINT('Ctrl Pts',(-41.7287247392384,37.309118652262,38.2637879487463));
#29462=CARTESIAN_POINT('Ctrl Pts',(-41.7382516861337,37.3194690477533,38.2715792505558));
#29463=CARTESIAN_POINT('Ctrl Pts',(-41.7477448185176,37.3298784440664,38.2793335223506));
#29464=CARTESIAN_POINT('Ctrl Pts',(-41.7572036968316,37.3403463593958,38.2870504052947));
#29465=CARTESIAN_POINT('Ctrl Pts',(-41.7666625751455,37.3508142747253,38.2947672882388));
#29466=CARTESIAN_POINT('Ctrl Pts',(-41.7760871993865,37.3613407090683,38.3024467823298));
#29467=CARTESIAN_POINT('Ctrl Pts',(-41.7854771331562,37.37192517522,38.3100885321811));
#29468=CARTESIAN_POINT('Ctrl Pts',(-41.7948670669259,37.3825096413715,38.3177302820325));
#29469=CARTESIAN_POINT('Ctrl Pts',(-41.8042223102216,37.3931521393287,38.3253342876419));
#29470=CARTESIAN_POINT('Ctrl Pts',(-41.8135424298451,37.4038521765317,38.332900197105));
#29471=CARTESIAN_POINT('Ctrl Pts',(-41.8228625494686,37.4145522137346,38.3404661065682));
#29472=CARTESIAN_POINT('Ctrl Pts',(-41.8321475454174,37.4253097901801,38.3479939198828));
#29473=CARTESIAN_POINT('Ctrl Pts',(-41.8413969877339,37.4361244079988,38.3554832886594));
#29474=CARTESIAN_POINT('Ctrl Pts',(-41.8506464300503,37.4469390258174,38.3629726574359));
#29475=CARTESIAN_POINT('Ctrl Pts',(-41.8598603187317,37.4578106850061,38.3704235816722));
#29476=CARTESIAN_POINT('Ctrl Pts',(-41.8690382271003,37.4687388824313,38.3778357165252));
#29477=CARTESIAN_POINT('Ctrl Pts',(-41.8782161354689,37.4796670798566,38.3852478513781));
#29478=CARTESIAN_POINT('Ctrl Pts',(-41.8873580635222,37.4906518155152,38.3926211968457));
#29479=CARTESIAN_POINT('Ctrl Pts',(-41.8964635879016,37.5016925810564,38.3999554116631));
#29480=CARTESIAN_POINT('Ctrl Pts',(-41.905569112281,37.5127333465975,38.4072896264807));
#29481=CARTESIAN_POINT('Ctrl Pts',(-41.9146382329839,37.5238301420179,38.4145847106461));
#29482=CARTESIAN_POINT('Ctrl Pts',(-41.92367053001,37.5349824537957,38.4218403265046));
#29483=CARTESIAN_POINT('Ctrl Pts',(-41.932702827036,37.5461347655735,38.4290959423631));
#29484=CARTESIAN_POINT('Ctrl Pts',(-41.9416983008208,37.5573425945316,38.4363120906505));
#29485=CARTESIAN_POINT('Ctrl Pts',(-41.9506565338972,37.5686054204039,38.4434884359012));
#29486=CARTESIAN_POINT('Ctrl Pts',(-41.9596147669736,37.5798682462761,38.450664781152));
#29487=CARTESIAN_POINT('Ctrl Pts',(-41.9685357597629,37.5911860698514,38.4578013240754));
#29488=CARTESIAN_POINT('Ctrl Pts',(-41.9774190990994,37.6025583674136,38.4648977343334));
#29489=CARTESIAN_POINT('Ctrl Pts',(-41.9863024384359,37.6139306649757,38.4719941445915));
#29490=CARTESIAN_POINT('Ctrl Pts',(-41.9951481243171,37.6253574365218,38.4790504221826));
#29491=CARTESIAN_POINT('Ctrl Pts',(-42.003955747045,37.636838153297,38.4860662404613));
#29492=CARTESIAN_POINT('Ctrl Pts',(-42.0127633697729,37.6483188700721,38.4930820587401));
#29493=CARTESIAN_POINT('Ctrl Pts',(-42.0215329293449,37.6598535320727,38.5000574177044));
#29494=CARTESIAN_POINT('Ctrl Pts',(-42.0302640195796,37.6714416055764,38.506991994451));
#29495=CARTESIAN_POINT('Ctrl Pts',(-42.0389951098142,37.6830296790801,38.5139265711977));
#29496=CARTESIAN_POINT('Ctrl Pts',(-42.0476877307091,37.6946711640841,38.5208203657249));
#29497=CARTESIAN_POINT('Ctrl Pts',(-42.056341479625,37.7063655219231,38.5276730588806));
#29498=CARTESIAN_POINT('Ctrl Pts',(-42.0649952285409,37.7180598797622,38.5345257520362));
#29499=CARTESIAN_POINT('Ctrl Pts',(-42.0736101054769,37.7298071104363,38.541337343821));
#29500=CARTESIAN_POINT('Ctrl Pts',(-42.0821857113822,37.7416066704065,38.5481075188797));
#29501=CARTESIAN_POINT('Ctrl Pts',(-42.0907613172874,37.7534062303768,38.5548776939382));
#29502=CARTESIAN_POINT('Ctrl Pts',(-42.0992976521577,37.7652581196358,38.5616064522654));
#29503=CARTESIAN_POINT('Ctrl Pts',(-42.1077943205678,37.7771617898219,38.568293482332));
#29504=CARTESIAN_POINT('Ctrl Pts',(-42.1162985403295,37.7890760393073,38.5749864554474));
#29505=CARTESIAN_POINT('Ctrl Pts',(-42.1247630224106,37.8010421602726,38.5816376248783));
#29506=CARTESIAN_POINT('Ctrl Pts',(-42.1331873753432,37.8130596011009,38.5882466845272));
#29507=CARTESIAN_POINT('Ctrl Pts',(-41.6954029970919,37.2787291081676,38.2453114933174));
#29508=CARTESIAN_POINT('Ctrl Pts',(-41.705374151905,37.2893988547556,38.2535435440881));
#29509=CARTESIAN_POINT('Ctrl Pts',(-41.7153090277789,37.3001332597734,38.2617357328736));
#29510=CARTESIAN_POINT('Ctrl Pts',(-41.7252071244471,37.3109317828591,38.269887647392));
#29511=CARTESIAN_POINT('Ctrl Pts',(-41.7351052211153,37.3217303059448,38.2780395619104));
#29512=CARTESIAN_POINT('Ctrl Pts',(-41.7449665385822,37.3325929471042,38.2861512021675));
#29513=CARTESIAN_POINT('Ctrl Pts',(-41.7547905802872,37.3435191595641,38.2942221599408));
#29514=CARTESIAN_POINT('Ctrl Pts',(-41.7646146219922,37.354445372024,38.302293117714));
#29515=CARTESIAN_POINT('Ctrl Pts',(-41.7744013879321,37.3654351557807,38.3103233930009));
#29516=CARTESIAN_POINT('Ctrl Pts',(-41.7841503852857,37.3764879576831,38.3183125816596));
#29517=CARTESIAN_POINT('Ctrl Pts',(-41.7938993826392,37.3875407595854,38.3263017703184));
#29518=CARTESIAN_POINT('Ctrl Pts',(-41.8036106114032,37.3986565796297,38.3342498723465));
#29519=CARTESIAN_POINT('Ctrl Pts',(-41.8132835825446,37.4098348583421,38.3421564877236));
#29520=CARTESIAN_POINT('Ctrl Pts',(-41.8229565536861,37.4210131370545,38.3500631031007));
#29521=CARTESIAN_POINT('Ctrl Pts',(-41.8325912672018,37.4322538744313,38.3579282318242));
#29522=CARTESIAN_POINT('Ctrl Pts',(-41.8421872378963,37.443556504732,38.365751478035));
#29523=CARTESIAN_POINT('Ctrl Pts',(-41.8517832085907,37.4548591350325,38.3735747242459));
#29524=CARTESIAN_POINT('Ctrl Pts',(-41.8613404364607,37.4662236582531,38.3813560879416));
#29525=CARTESIAN_POINT('Ctrl Pts',(-41.8708584401965,37.4776495024429,38.3890951774638));
#29526=CARTESIAN_POINT('Ctrl Pts',(-41.8803764439323,37.4890753466328,38.3968342669861));
#29527=CARTESIAN_POINT('Ctrl Pts',(-41.8898552235308,37.5005625117879,38.4045310823324));
#29528=CARTESIAN_POINT('Ctrl Pts',(-41.899294301616,37.5121104198047,38.4121852360844));
#29529=CARTESIAN_POINT('Ctrl Pts',(-41.9087333797013,37.5236583278214,38.4198393898364));
#29530=CARTESIAN_POINT('Ctrl Pts',(-41.9181327562374,37.5352669786346,38.4274508819364));
#29531=CARTESIAN_POINT('Ctrl Pts',(-41.9274919578949,37.5469357881649,38.4350193293532));
#29532=CARTESIAN_POINT('Ctrl Pts',(-41.9368511595524,37.5586045976952,38.4425877767701));
#29533=CARTESIAN_POINT('Ctrl Pts',(-41.9461701862917,37.570333565871,38.4501131794401));
#29534=CARTESIAN_POINT('Ctrl Pts',(-41.9554485687568,37.5821221024738,38.4575951585563));
#29535=CARTESIAN_POINT('Ctrl Pts',(-41.964726951222,37.5939106390765,38.4650771376724));
#29536=CARTESIAN_POINT('Ctrl Pts',(-41.9739646894053,37.6057587440936,38.4725156932246));
#29537=CARTESIAN_POINT('Ctrl Pts',(-41.9831613180177,37.6176658213109,38.4799104507449));
#29538=CARTESIAN_POINT('Ctrl Pts',(-41.9923579466302,37.6295728985282,38.4873052082651));
#29539=CARTESIAN_POINT('Ctrl Pts',(-42.0015134656686,37.6415389479416,38.494656167751));
#29540=CARTESIAN_POINT('Ctrl Pts',(-42.0106274139663,37.6535633674186,38.501962959127));
#29541=CARTESIAN_POINT('Ctrl Pts',(-42.019741362264,37.6655877868956,38.5092697505029));
#29542=CARTESIAN_POINT('Ctrl Pts',(-42.028813739818,37.6776705764321,38.5165323737665));
#29543=CARTESIAN_POINT('Ctrl Pts',(-42.0378440896301,37.6898111280371,38.5237504632711));
#29544=CARTESIAN_POINT('Ctrl Pts',(-42.0468744394422,37.7019516796421,38.5309685527758));
#29545=CARTESIAN_POINT('Ctrl Pts',(-42.0558627615093,37.7141499933116,38.5381421085192));
#29546=CARTESIAN_POINT('Ctrl Pts',(-42.0648086030478,37.726405455257,38.5452707693207));
#29547=CARTESIAN_POINT('Ctrl Pts',(-42.0737544445863,37.7386609172024,38.5523994301222));
#29548=CARTESIAN_POINT('Ctrl Pts',(-42.0826578055931,37.7509735274196,38.5594831959794));
#29549=CARTESIAN_POINT('Ctrl Pts',(-42.0915182375439,37.7633426663837,38.5665217102134));
#29550=CARTESIAN_POINT('Ctrl Pts',(-42.1003786694947,37.7757118053479,38.5735602244475));
#29551=CARTESIAN_POINT('Ctrl Pts',(-42.1091961723865,37.7881374730549,38.580553487056));
#29552=CARTESIAN_POINT('Ctrl Pts',(-42.1179703019997,37.8006190443054,38.5875011458977));
#29553=CARTESIAN_POINT('Ctrl Pts',(-42.126752229556,37.8131117084607,38.5944549794202));
#29554=CARTESIAN_POINT('Ctrl Pts',(-42.1354907067083,37.8256603755839,38.6013631280908));
#29555=CARTESIAN_POINT('Ctrl Pts',(-42.1441852923974,37.8382644131475,38.608225243387));
#29556=CARTESIAN_POINT('Ctrl Pts',(-41.6907493022857,37.2791971682105,38.2503061045895));
#29557=CARTESIAN_POINT('Ctrl Pts',(-41.7010860575057,37.2902935419084,38.2588974308395));
#29558=CARTESIAN_POINT('Ctrl Pts',(-41.7113835341543,37.3014599201502,38.2674455992172));
#29559=CARTESIAN_POINT('Ctrl Pts',(-41.7216411691384,37.3126956923255,38.2759501422807));
#29560=CARTESIAN_POINT('Ctrl Pts',(-41.7318988041226,37.3239314645008,38.2844546853442));
#29561=CARTESIAN_POINT('Ctrl Pts',(-41.7421165974454,37.3352366306143,38.2929156030983));
#29562=CARTESIAN_POINT('Ctrl Pts',(-41.7522939903866,37.3466105724872,38.3013324328907));
#29563=CARTESIAN_POINT('Ctrl Pts',(-41.7624713833279,37.35798451436,38.3097492626831));
#29564=CARTESIAN_POINT('Ctrl Pts',(-41.7726083758836,37.3694272319876,38.3181220045104));
#29565=CARTESIAN_POINT('Ctrl Pts',(-41.7827044137518,37.3809380996695,38.3264502005419));
#29566=CARTESIAN_POINT('Ctrl Pts',(-41.7928004516199,37.3924489673513,38.3347783965733));
#29567=CARTESIAN_POINT('Ctrl Pts',(-41.8028555347964,37.4040279850829,38.3430620468056));
#29568=CARTESIAN_POINT('Ctrl Pts',(-41.8128691134583,37.4156745197107,38.3513006982795));
#29569=CARTESIAN_POINT('Ctrl Pts',(-41.8228826921201,37.4273210543384,38.3595393497535));
#29570=CARTESIAN_POINT('Ctrl Pts',(-41.8328547662634,37.4390351058577,38.3677330024657));
#29571=CARTESIAN_POINT('Ctrl Pts',(-41.8427847906039,37.4508160337313,38.3758812083785));
#29572=CARTESIAN_POINT('Ctrl Pts',(-41.8527148149444,37.4625969616049,38.3840294142911));
#29573=CARTESIAN_POINT('Ctrl Pts',(-41.8626027894783,37.4744447658281,38.392132173401));
#29574=CARTESIAN_POINT('Ctrl Pts',(-41.8724481735202,37.4863587985498,38.4001890426401));
#29575=CARTESIAN_POINT('Ctrl Pts',(-41.8822935575621,37.4982728312715,38.4082459118793));
#29576=CARTESIAN_POINT('Ctrl Pts',(-41.892096351108,37.5102530924869,38.4162568912445));
#29577=CARTESIAN_POINT('Ctrl Pts',(-41.9018560181304,37.5222989271022,38.4242215426866));
#29578=CARTESIAN_POINT('Ctrl Pts',(-41.9116156851527,37.5343447617176,38.4321861941288));
#29579=CARTESIAN_POINT('Ctrl Pts',(-41.9213322256173,37.5464561696706,38.4401045175926));
#29580=CARTESIAN_POINT('Ctrl Pts',(-41.9310051082727,37.5586324888085,38.4479760801976));
#29581=CARTESIAN_POINT('Ctrl Pts',(-41.9406779909281,37.5708088079463,38.4558476428027));
#29582=CARTESIAN_POINT('Ctrl Pts',(-41.9503072157368,37.5830500382009,38.463672444488));
#29583=CARTESIAN_POINT('Ctrl Pts',(-41.9598922561705,37.5953555102244,38.4714500573998));
#29584=CARTESIAN_POINT('Ctrl Pts',(-41.9694772966042,37.6076609822479,38.4792276703115));
#29585=CARTESIAN_POINT('Ctrl Pts',(-41.9790181526549,37.6200306960276,38.4869580944392));
#29586=CARTESIAN_POINT('Ctrl Pts',(-41.9885143026182,37.6324639751736,38.4946409070749));
#29587=CARTESIAN_POINT('Ctrl Pts',(-41.9980104525814,37.6448972543196,38.5023237197104));
#29588=CARTESIAN_POINT('Ctrl Pts',(-42.0074618964534,37.6573940988272,38.5099589208508));
#29589=CARTESIAN_POINT('Ctrl Pts',(-42.0168681174187,37.6699538253549,38.5175460929948));
#29590=CARTESIAN_POINT('Ctrl Pts',(-42.026274338384,37.6825135518827,38.5251332651387));
#29591=CARTESIAN_POINT('Ctrl Pts',(-42.0356353364388,37.6951361604256,38.5326724082832));
#29592=CARTESIAN_POINT('Ctrl Pts',(-42.0449505997135,37.7078209607656,38.5401631101795));
#29593=CARTESIAN_POINT('Ctrl Pts',(-42.0542658629882,37.7205057611056,38.5476538120758));
#29594=CARTESIAN_POINT('Ctrl Pts',(-42.063535391479,37.7332527532376,38.555096072721));
#29595=CARTESIAN_POINT('Ctrl Pts',(-42.0727586783179,37.7460612401418,38.562489485164));
#29596=CARTESIAN_POINT('Ctrl Pts',(-42.0819819651568,37.7588697270461,38.569882897607));
#29597=CARTESIAN_POINT('Ctrl Pts',(-42.0911590103401,37.7717397087176,38.5772274618448));
#29598=CARTESIAN_POINT('Ctrl Pts',(-42.1002893120568,37.7846704814115,38.5845227762687));
#29599=CARTESIAN_POINT('Ctrl Pts',(-42.1094196137735,37.7976012541054,38.5918180906926));
#29600=CARTESIAN_POINT('Ctrl Pts',(-42.1185031720199,37.8105928178165,38.5990641552995));
#29601=CARTESIAN_POINT('Ctrl Pts',(-42.1275394900971,37.8236444621519,38.6062605738666));
#29602=CARTESIAN_POINT('Ctrl Pts',(-42.1365838391356,37.8367077060402,38.6134633881979));
#29603=CARTESIAN_POINT('Ctrl Pts',(-42.1455808640018,37.8498311374031,38.6206164682147));
#29604=CARTESIAN_POINT('Ctrl Pts',(-42.1545300718383,37.8630140373325,38.627719422056));
#29605=CARTESIAN_POINT('Ctrl Pts',(-41.6814419126733,37.2801332882965,38.2602953271335));
#29606=CARTESIAN_POINT('Ctrl Pts',(-41.692509868707,37.2920829162141,38.2696052043424));
#29607=CARTESIAN_POINT('Ctrl Pts',(-41.7035325469051,37.3041132409037,38.2788653319044));
#29608=CARTESIAN_POINT('Ctrl Pts',(-41.7145092585211,37.3162235112583,38.2880751320582));
#29609=CARTESIAN_POINT('Ctrl Pts',(-41.7254859701371,37.3283337816128,38.2972849322119));
#29610=CARTESIAN_POINT('Ctrl Pts',(-41.7364167151718,37.3405239976348,38.30644440496));
#29611=CARTESIAN_POINT('Ctrl Pts',(-41.7473008105857,37.3527933983334,38.3155529787907));
#29612=CARTESIAN_POINT('Ctrl Pts',(-41.7581849059995,37.3650627990321,38.3246615526213));
#29613=CARTESIAN_POINT('Ctrl Pts',(-41.7690223517866,37.3774113844015,38.3337192275295));
#29614=CARTESIAN_POINT('Ctrl Pts',(-41.7798124706839,37.3898383836423,38.3427254383063));
#29615=CARTESIAN_POINT('Ctrl Pts',(-41.7906025895811,37.4022653828832,38.3517316490831));
#29616=CARTESIAN_POINT('Ctrl Pts',(-41.8013453815828,37.4147707959893,38.3606863957238));
#29617=CARTESIAN_POINT('Ctrl Pts',(-41.8120401752855,37.4273538424477,38.3695891193914));
#29618=CARTESIAN_POINT('Ctrl Pts',(-41.8227349689883,37.4399368889061,38.378491843059));
#29619=CARTESIAN_POINT('Ctrl Pts',(-41.8333817643865,37.4525975687106,38.3873425437489));
#29620=CARTESIAN_POINT('Ctrl Pts',(-41.8439798960192,37.4653350917302,38.3961406690652));
#29621=CARTESIAN_POINT('Ctrl Pts',(-41.8545780276519,37.4780726147497,38.4049387943816));
#29622=CARTESIAN_POINT('Ctrl Pts',(-41.8651274955135,37.4908869809781,38.4136843443197));
#29623=CARTESIAN_POINT('Ctrl Pts',(-41.8756276401675,37.5037773907635,38.4223767729926));
#29624=CARTESIAN_POINT('Ctrl Pts',(-41.8861277848215,37.516667800549,38.4310692016655));
#29625=CARTESIAN_POINT('Ctrl Pts',(-41.8965786062624,37.529634253885,38.4397085090687));
#29626=CARTESIAN_POINT('Ctrl Pts',(-41.906979451159,37.5426759416976,38.448294155891));
#29627=CARTESIAN_POINT('Ctrl Pts',(-41.9173802960555,37.5557176295101,38.4568798027133));
#29628=CARTESIAN_POINT('Ctrl Pts',(-41.9277311643771,37.5688345517426,38.4654117889052));
#29629=CARTESIAN_POINT('Ctrl Pts',(-41.9380314090283,37.5820258900957,38.4738895818864));
#29630=CARTESIAN_POINT('Ctrl Pts',(-41.9483316536795,37.5952172284488,38.4823673748677));
#29631=CARTESIAN_POINT('Ctrl Pts',(-41.958581274627,37.6084829828606,38.4907909745839));
#29632=CARTESIAN_POINT('Ctrl Pts',(-41.9687796309978,37.6218223257258,38.4991598550868));
#29633=CARTESIAN_POINT('Ctrl Pts',(-41.9789779873686,37.6351616685908,38.5075287355896));
#29634=CARTESIAN_POINT('Ctrl Pts',(-41.9891250791542,37.6485745998954,38.5158428968686));
#29635=CARTESIAN_POINT('Ctrl Pts',(-41.9992202718191,37.6620602828989,38.5241018197348));
#29636=CARTESIAN_POINT('Ctrl Pts',(-42.0093154644839,37.6755459659026,38.532360742601));
#29637=CARTESIAN_POINT('Ctrl Pts',(-42.019358758023,37.6891044005982,38.5405644270504));
#29638=CARTESIAN_POINT('Ctrl Pts',(-42.0293495243234,37.7027347412276,38.5487123607303));
#29639=CARTESIAN_POINT('Ctrl Pts',(-42.0393402906239,37.7163650818568,38.5568602944103));
#29640=CARTESIAN_POINT('Ctrl Pts',(-42.0492785296805,37.7300673284127,38.5649524773167));
#29641=CARTESIAN_POINT('Ctrl Pts',(-42.0591636198804,37.7438406262226,38.5729884039963));
#29642=CARTESIAN_POINT('Ctrl Pts',(-42.0690487100803,37.7576139240325,38.5810243306759));
#29643=CARTESIAN_POINT('Ctrl Pts',(-42.0788806514184,37.7714582730893,38.5890040011246));
#29644=CARTESIAN_POINT('Ctrl Pts',(-42.0886588288581,37.7853728099114,38.5969269168506));
#29645=CARTESIAN_POINT('Ctrl Pts',(-42.0984370062978,37.7992873467335,38.6048498325766));
#29646=CARTESIAN_POINT('Ctrl Pts',(-42.1081614198342,37.8132720713135,38.6127159935759));
#29647=CARTESIAN_POINT('Ctrl Pts',(-42.1178314610826,37.8273261114669,38.6205249083793));
#29648=CARTESIAN_POINT('Ctrl Pts',(-42.127501502331,37.8413801516203,38.6283338231828));
#29649=CARTESIAN_POINT('Ctrl Pts',(-42.1371171712866,37.8555035073398,38.6360854917864));
#29650=CARTESIAN_POINT('Ctrl Pts',(-42.1466778662919,37.8696952978447,38.6437794298044));
#29651=CARTESIAN_POINT('Ctrl Pts',(-42.1562470582947,37.8838997011991,38.6514802057533));
#29652=CARTESIAN_POINT('Ctrl Pts',(-42.1657611785889,37.8981726610412,38.6591231484625));
#29653=CARTESIAN_POINT('Ctrl Pts',(-42.1752196307201,37.9125132857024,38.6667077793939));
#29654=CARTESIAN_POINT('Ctrl Pts',(-41.6720797281154,37.281005440121,38.2702306591526));
#29655=CARTESIAN_POINT('Ctrl Pts',(-41.6838331847125,37.2937633030351,38.2802276560053));
#29656=CARTESIAN_POINT('Ctrl Pts',(-41.6955349997854,37.3066132044251,38.2901679110195));
#29657=CARTESIAN_POINT('Ctrl Pts',(-41.707184337945,37.3195542276318,38.3000507155175));
#29658=CARTESIAN_POINT('Ctrl Pts',(-41.7188336761045,37.3324952508385,38.3099335200156));
#29659=CARTESIAN_POINT('Ctrl Pts',(-41.7304305373428,37.3455273958532,38.319758873991));
#29660=CARTESIAN_POINT('Ctrl Pts',(-41.7419740936924,37.3586497331262,38.3295260768912));
#29661=CARTESIAN_POINT('Ctrl Pts',(-41.753517650042,37.3717720703992,38.3392932797915));
#29662=CARTESIAN_POINT('Ctrl Pts',(-41.7650079014953,37.3849845999216,38.3490023316102));
#29663=CARTESIAN_POINT('Ctrl Pts',(-41.7764440276226,37.3982863793831,38.3586525400184));
#29664=CARTESIAN_POINT('Ctrl Pts',(-41.78788015375,37.4115881588446,38.3683027484267));
#29665=CARTESIAN_POINT('Ctrl Pts',(-41.7992621545438,37.4249791882362,38.377894113418));
#29666=CARTESIAN_POINT('Ctrl Pts',(-41.8105892172277,37.438458512619,38.387425950984));
#29667=CARTESIAN_POINT('Ctrl Pts',(-41.8219162799116,37.4519378370016,38.3969577885501));
#29668=CARTESIAN_POINT('Ctrl Pts',(-41.833188404478,37.4655054563663,38.4064300986844));
#29669=CARTESIAN_POINT('Ctrl Pts',(-41.8444047859174,37.479160403279,38.4158422057947));
#29670=CARTESIAN_POINT('Ctrl Pts',(-41.8556211673568,37.4928153501917,38.425254312905));
#29671=CARTESIAN_POINT('Ctrl Pts',(-41.8667818056617,37.5065576246432,38.4346062169849));
#29672=CARTESIAN_POINT('Ctrl Pts',(-41.8778859037026,37.5203862468399,38.4438972509529));
#29673=CARTESIAN_POINT('Ctrl Pts',(-41.8889900017434,37.5342148690365,38.4531882849209));
#29674=CARTESIAN_POINT('Ctrl Pts',(-41.9000375595128,37.5481298389691,38.4624184487706));
#29675=CARTESIAN_POINT('Ctrl Pts',(-41.9110277878729,37.5621301646213,38.4715870840247));
#29676=CARTESIAN_POINT('Ctrl Pts',(-41.9220180162329,37.5761304902734,38.4807557192787));
#29677=CARTESIAN_POINT('Ctrl Pts',(-41.9329509151763,37.5902161716359,38.489862825931));
#29678=CARTESIAN_POINT('Ctrl Pts',(-41.9438257036674,37.6043862046088,38.4989077542001));
#29679=CARTESIAN_POINT('Ctrl Pts',(-41.9547004921585,37.6185562375817,38.5079526824692));
#29680=CARTESIAN_POINT('Ctrl Pts',(-41.9655171701902,37.6328106221554,38.5169354323492));
#29681=CARTESIAN_POINT('Ctrl Pts',(-41.9762749649388,37.647148342287,38.5258553628462));
#29682=CARTESIAN_POINT('Ctrl Pts',(-41.9870327596873,37.6614860624186,38.5347752933432));
#29683=CARTESIAN_POINT('Ctrl Pts',(-41.9977316711457,37.6759071180982,38.5436324044513));
#29684=CARTESIAN_POINT('Ctrl Pts',(-42.0083709348107,37.6904104814819,38.5524260640536));
#29685=CARTESIAN_POINT('Ctrl Pts',(-42.0190101984756,37.7049138448655,38.561219723656));
#29686=CARTESIAN_POINT('Ctrl Pts',(-42.0295898143401,37.7194995159433,38.5699499317467));
#29687=CARTESIAN_POINT('Ctrl Pts',(-42.0401090263286,37.7341664552137,38.5786160651747));
#29688=CARTESIAN_POINT('Ctrl Pts',(-42.0506282383171,37.7488333944841,38.5872821986028));
#29689=CARTESIAN_POINT('Ctrl Pts',(-42.0610870464226,37.7635816019373,38.5958842573624));
#29690=CARTESIAN_POINT('Ctrl Pts',(-42.0714847031035,37.7784100265598,38.6044216273555));
#29691=CARTESIAN_POINT('Ctrl Pts',(-42.0818823597843,37.7932384511822,38.6129589973486));
#29692=CARTESIAN_POINT('Ctrl Pts',(-42.0922188650336,37.808147092964,38.6214316785695));
#29693=CARTESIAN_POINT('Ctrl Pts',(-42.1024934799483,37.8231348895265,38.6298390660592));
#29694=CARTESIAN_POINT('Ctrl Pts',(-42.1127680948631,37.838122686089,38.6382464535489));
#29695=CARTESIAN_POINT('Ctrl Pts',(-42.1229808194365,37.8531896374223,38.6465885473018));
#29696=CARTESIAN_POINT('Ctrl Pts',(-42.1331309235081,37.8683346699313,38.654864751583));
#29697=CARTESIAN_POINT('Ctrl Pts',(-42.1432810275798,37.8834797024403,38.6631409558641));
#29698=CARTESIAN_POINT('Ctrl Pts',(-42.1533685111429,37.898702816115,38.6713512706679));
#29699=CARTESIAN_POINT('Ctrl Pts',(-42.1633926528822,37.9140029262941,38.6794951095668));
#29700=CARTESIAN_POINT('Ctrl Pts',(-42.1734257035038,37.9293166343336,38.6876461862427));
#29701=CARTESIAN_POINT('Ctrl Pts',(-42.1833952996557,37.9447074757883,38.6957306687958));
#29702=CARTESIAN_POINT('Ctrl Pts',(-42.1933007270679,37.9601743521583,38.7037479786483));
#29703=CARTESIAN_POINT('Ctrl Pts',(-41.6626778025171,37.2818311977891,38.2801269060787));
#29704=CARTESIAN_POINT('Ctrl Pts',(-41.6750793521725,37.2953573955639,38.2907803473701));
#29705=CARTESIAN_POINT('Ctrl Pts',(-41.6874226859157,37.3089873490621,38.3013698231234));
#29706=CARTESIAN_POINT('Ctrl Pts',(-41.6997068034004,37.3227199536653,38.3118944751311));
#29707=CARTESIAN_POINT('Ctrl Pts',(-41.7119909208852,37.3364525582684,38.3224191271388));
#29708=CARTESIAN_POINT('Ctrl Pts',(-41.7242158221008,37.3502878139645,38.3328789553917));
#29709=CARTESIAN_POINT('Ctrl Pts',(-41.7363805162991,37.3642245994969,38.3432731121893));
#29710=CARTESIAN_POINT('Ctrl Pts',(-41.7485452104974,37.3781613850294,38.353667268987));
#29711=CARTESIAN_POINT('Ctrl Pts',(-41.7606496976679,37.3921997003858,38.3639957543202));
#29712=CARTESIAN_POINT('Ctrl Pts',(-41.7726929968212,37.406338407853,38.3742577311332));
#29713=CARTESIAN_POINT('Ctrl Pts',(-41.7847362959746,37.4204771153202,38.3845197079461));
#29714=CARTESIAN_POINT('Ctrl Pts',(-41.7967184071002,37.4347162148858,38.3947151762297));
#29715=CARTESIAN_POINT('Ctrl Pts',(-41.8086383591267,37.4490545525641,38.4048433097082));
#29716=CARTESIAN_POINT('Ctrl Pts',(-41.8205583111532,37.4633928902424,38.4149714431867));
#29717=CARTESIAN_POINT('Ctrl Pts',(-41.8324161040701,37.4778304660209,38.4250322418513));
#29718=CARTESIAN_POINT('Ctrl Pts',(-41.844210776881,37.4923661098289,38.43502489034));
#29719=CARTESIAN_POINT('Ctrl Pts',(-41.856005449692,37.5069017536367,38.4450175388289));
#29720=CARTESIAN_POINT('Ctrl Pts',(-41.8677370023867,37.5215354654614,38.4549420371332));
#29721=CARTESIAN_POINT('Ctrl Pts',(-41.8794044841998,37.5362660593363,38.4647975809376));
#29722=CARTESIAN_POINT('Ctrl Pts',(-41.8910719660129,37.5509966532113,38.474653124742));
#29723=CARTESIAN_POINT('Ctrl Pts',(-41.9026753769342,37.5658241291238,38.4844397140379));
#29724=CARTESIAN_POINT('Ctrl Pts',(-41.9142137765834,37.580747285404,38.4941565556864));
#29725=CARTESIAN_POINT('Ctrl Pts',(-41.9257521762325,37.5956704416843,38.5038733973348));
#29726=CARTESIAN_POINT('Ctrl Pts',(-41.9372255645993,37.6106892783193,38.5135204913274));
#29727=CARTESIAN_POINT('Ctrl Pts',(-41.9486330118411,37.6258025781309,38.5230970558303));
#29728=CARTESIAN_POINT('Ctrl Pts',(-41.9600404590829,37.6409158779426,38.5326736203333));
#29729=CARTESIAN_POINT('Ctrl Pts',(-41.9713819651896,37.6561236409176,38.5421796553383));
#29730=CARTESIAN_POINT('Ctrl Pts',(-41.9826566110065,37.6714246345665,38.5516143904435));
#29731=CARTESIAN_POINT('Ctrl Pts',(-41.9939312568235,37.6867256282154,38.5610491255488));
#29732=CARTESIAN_POINT('Ctrl Pts',(-42.0051390423408,37.702119852525,38.570412560746));
#29733=CARTESIAN_POINT('Ctrl Pts',(-42.016279059241,37.7176060598942,38.5797039371903));
#29734=CARTESIAN_POINT('Ctrl Pts',(-42.0274190761412,37.7330922672635,38.5889953136346));
#29735=CARTESIAN_POINT('Ctrl Pts',(-42.0384913244147,37.7486704576788,38.5982146313178));
#29736=CARTESIAN_POINT('Ctrl Pts',(-42.0494949067281,37.7643393686301,38.6073611430746));
#29737=CARTESIAN_POINT('Ctrl Pts',(-42.0604984890416,37.7800082795815,38.6165076548315));
#29738=CARTESIAN_POINT('Ctrl Pts',(-42.0714334053855,37.7957679110552,38.625581360654));
#29739=CARTESIAN_POINT('Ctrl Pts',(-42.0822987695567,37.8116169858364,38.6345815251779));
#29740=CARTESIAN_POINT('Ctrl Pts',(-42.0931641337279,37.8274660606176,38.6435816897018));
#29741=CARTESIAN_POINT('Ctrl Pts',(-42.1039599457167,37.8434045786925,38.6525083129191));
#29742=CARTESIAN_POINT('Ctrl Pts',(-42.1146853305936,37.8594312483488,38.6613606713857));
#29743=CARTESIAN_POINT('Ctrl Pts',(-42.1254107154704,37.8754579180051,38.6702130298523));
#29744=CARTESIAN_POINT('Ctrl Pts',(-42.1360656732259,37.8915727392288,38.6789911235603));
#29745=CARTESIAN_POINT('Ctrl Pts',(-42.1466493403455,37.9077744060193,38.6876942411029));
#29746=CARTESIAN_POINT('Ctrl Pts',(-42.1572330074652,37.9239760728097,38.6963973586456));
#29747=CARTESIAN_POINT('Ctrl Pts',(-42.1677453839397,37.9402645851528,38.7050255000152));
#29748=CARTESIAN_POINT('Ctrl Pts',(-42.17818561781,37.9566386229715,38.7135779659575));
#29749=CARTESIAN_POINT('Ctrl Pts',(-42.1886351303615,37.973027213096,38.7221380328411));
#29750=CARTESIAN_POINT('Ctrl Pts',(-42.1990123720102,37.9895014807696,38.7306222897181));
#29751=CARTESIAN_POINT('Ctrl Pts',(-42.209316500248,38.0060600884928,38.7390300477671));
#29752=CARTESIAN_POINT('Ctrl Pts',(-41.6532758769187,37.2826569554572,38.2900231530048));
#29753=CARTESIAN_POINT('Ctrl Pts',(-41.6663255196325,37.2969514880927,38.3013330387349));
#29754=CARTESIAN_POINT('Ctrl Pts',(-41.6793103720459,37.3113614936992,38.3125717352273));
#29755=CARTESIAN_POINT('Ctrl Pts',(-41.6922292688559,37.3258856796987,38.3237382347446));
#29756=CARTESIAN_POINT('Ctrl Pts',(-41.7051481656659,37.3404098656984,38.3349047342619));
#29757=CARTESIAN_POINT('Ctrl Pts',(-41.7180011068587,37.3550482320758,38.3459990367924));
#29758=CARTESIAN_POINT('Ctrl Pts',(-41.7307869389058,37.3697994658677,38.3570201474874));
#29759=CARTESIAN_POINT('Ctrl Pts',(-41.7435727709529,37.3845506996595,38.3680412581824));
#29760=CARTESIAN_POINT('Ctrl Pts',(-41.7562914938406,37.39941480085,38.3789891770303));
#29761=CARTESIAN_POINT('Ctrl Pts',(-41.7689419660199,37.4143904363229,38.3898629222479));
#29762=CARTESIAN_POINT('Ctrl Pts',(-41.7815924381992,37.4293660717959,38.4007366674656));
#29763=CARTESIAN_POINT('Ctrl Pts',(-41.7941746596566,37.4444532415353,38.4115362390414));
#29764=CARTESIAN_POINT('Ctrl Pts',(-41.8066875010257,37.4596505925093,38.4222606684324));
#29765=CARTESIAN_POINT('Ctrl Pts',(-41.8192003423948,37.4748479434832,38.4329850978234));
#29766=CARTESIAN_POINT('Ctrl Pts',(-41.8316438036622,37.4901554756755,38.4436343850181));
#29767=CARTESIAN_POINT('Ctrl Pts',(-41.8440167678447,37.5055718163786,38.4542075748854));
#29768=CARTESIAN_POINT('Ctrl Pts',(-41.8563897320273,37.5209881570818,38.4647807647527));
#29769=CARTESIAN_POINT('Ctrl Pts',(-41.8686921991118,37.5365133062795,38.4752778572815));
#29770=CARTESIAN_POINT('Ctrl Pts',(-41.8809230646971,37.5521458718328,38.4856979109224));
#29771=CARTESIAN_POINT('Ctrl Pts',(-41.8931539302824,37.5677784373861,38.4961179645632));
#29772=CARTESIAN_POINT('Ctrl Pts',(-41.9053131943556,37.5835184192784,38.5064609793052));
#29773=CARTESIAN_POINT('Ctrl Pts',(-41.9173997652938,37.5993644061868,38.516726027348));
#29774=CARTESIAN_POINT('Ctrl Pts',(-41.929486336232,37.6152103930952,38.5269910753909));
#29775=CARTESIAN_POINT('Ctrl Pts',(-41.9415002140224,37.6311623850027,38.5371781567238));
#29776=CARTESIAN_POINT('Ctrl Pts',(-41.9534403200148,37.6472189516531,38.5472863574605));
#29777=CARTESIAN_POINT('Ctrl Pts',(-41.9653804260072,37.6632755183035,38.5573945581973));
#29778=CARTESIAN_POINT('Ctrl Pts',(-41.9772467601889,37.6794366596797,38.5674238783273));
#29779=CARTESIAN_POINT('Ctrl Pts',(-41.9890382570742,37.695700926846,38.5773734180408));
#29780=CARTESIAN_POINT('Ctrl Pts',(-42.0008297539595,37.7119651940124,38.5873229577543));
#29781=CARTESIAN_POINT('Ctrl Pts',(-42.0125464135358,37.7283325869518,38.5971927170407));
#29782=CARTESIAN_POINT('Ctrl Pts',(-42.0241871836713,37.7448016383066,38.606981810327));
#29783=CARTESIAN_POINT('Ctrl Pts',(-42.0358279538069,37.7612706896614,38.6167709036133));
#29784=CARTESIAN_POINT('Ctrl Pts',(-42.0473928344892,37.7778413994143,38.6264793308889));
#29785=CARTESIAN_POINT('Ctrl Pts',(-42.0588807871277,37.7945122820466,38.6361062209745));
#29786=CARTESIAN_POINT('Ctrl Pts',(-42.0703687397661,37.8111831646789,38.6457331110602));
#29787=CARTESIAN_POINT('Ctrl Pts',(-42.0817797643485,37.827954220173,38.6552784639456));
#29788=CARTESIAN_POINT('Ctrl Pts',(-42.0931128360099,37.844823945113,38.6647414230003));
#29789=CARTESIAN_POINT('Ctrl Pts',(-42.1044459076713,37.8616936700531,38.6742043820549));
#29790=CARTESIAN_POINT('Ctrl Pts',(-42.1157010263998,37.8786620644211,38.6835849472687));
#29791=CARTESIAN_POINT('Ctrl Pts',(-42.1268771812388,37.8957276071712,38.6928822767122));
#29792=CARTESIAN_POINT('Ctrl Pts',(-42.1380533360778,37.9127931499213,38.7021796061556));
#29793=CARTESIAN_POINT('Ctrl Pts',(-42.1491505270153,37.9299558410353,38.7113936998188));
#29794=CARTESIAN_POINT('Ctrl Pts',(-42.1601677571829,37.9472141421073,38.7205237306229));
#29795=CARTESIAN_POINT('Ctrl Pts',(-42.1711849873505,37.9644724431792,38.729653761427));
#29796=CARTESIAN_POINT('Ctrl Pts',(-42.1821222567365,37.9818263541906,38.7386997293624));
#29797=CARTESIAN_POINT('Ctrl Pts',(-42.1929785827378,37.9992743196491,38.7476608223481));
#29798=CARTESIAN_POINT('Ctrl Pts',(-42.2038445572192,38.0167377918585,38.7566298794394));
#29799=CARTESIAN_POINT('Ctrl Pts',(-42.2146294443647,38.034295485751,38.7655139106404));
#29800=CARTESIAN_POINT('Ctrl Pts',(-42.2253322734281,38.0519458248273,38.7743121168858));
#29801=CARTESIAN_POINT('Ctrl Pts',(-41.6438340612598,37.2834361450012,38.2998801682775));
#29802=CARTESIAN_POINT('Ctrl Pts',(-41.6574945992981,37.2984594669515,38.3118162074907));
#29803=CARTESIAN_POINT('Ctrl Pts',(-41.6710835592186,37.3136103595045,38.3236735992583));
#29804=CARTESIAN_POINT('Ctrl Pts',(-41.6845995924923,37.3288873197827,38.3354511677636));
#29805=CARTESIAN_POINT('Ctrl Pts',(-41.6981156257661,37.3441642800609,38.3472287362689));
#29806=CARTESIAN_POINT('Ctrl Pts',(-41.7115587323755,37.3595673080445,38.3589264814965));
#29807=CARTESIAN_POINT('Ctrl Pts',(-41.7249275781878,37.3750948759654,38.3705432433879));
#29808=CARTESIAN_POINT('Ctrl Pts',(-41.738296424,37.3906224438864,38.3821600052791));
#29809=CARTESIAN_POINT('Ctrl Pts',(-41.7515910089977,37.4062745517245,38.3936957838189));
#29810=CARTESIAN_POINT('Ctrl Pts',(-41.7648100137066,37.4220496471208,38.405149434934));
#29811=CARTESIAN_POINT('Ctrl Pts',(-41.7780290184155,37.4378247425171,38.416603086049));
#29812=CARTESIAN_POINT('Ctrl Pts',(-41.7911724428184,37.4537228254511,38.4279746097245));
#29813=CARTESIAN_POINT('Ctrl Pts',(-41.8042389823588,37.4697423192777,38.4392628780974));
#29814=CARTESIAN_POINT('Ctrl Pts',(-41.8173055218992,37.4857618131042,38.4505511464703));
#29815=CARTESIAN_POINT('Ctrl Pts',(-41.83029517656,37.5019027178025,38.461756159526));
#29816=CARTESIAN_POINT('Ctrl Pts',(-41.8432066569589,37.5181634327507,38.472876805833));
#29817=CARTESIAN_POINT('Ctrl Pts',(-41.8561181373577,37.5344241476989,38.48399745214));
#29818=CARTESIAN_POINT('Ctrl Pts',(-41.8689514434778,37.5508046728759,38.4950337316839));
#29819=CARTESIAN_POINT('Ctrl Pts',(-41.8817053013641,37.5673033839973,38.5059845496832));
#29820=CARTESIAN_POINT('Ctrl Pts',(-41.8944591592503,37.5838020951187,38.5169353676825));
#29821=CARTESIAN_POINT('Ctrl Pts',(-41.9071335688862,37.6004189921631,38.5278007241229));
#29822=CARTESIAN_POINT('Ctrl Pts',(-41.9197272719944,37.6171524275023,38.5385795410877));
#29823=CARTESIAN_POINT('Ctrl Pts',(-41.9323209751025,37.6338858628415,38.5493583580525));
#29824=CARTESIAN_POINT('Ctrl Pts',(-41.9448339716667,37.6507358364539,38.5600506355277));
#29825=CARTESIAN_POINT('Ctrl Pts',(-41.9572650193348,37.6677006776908,38.5706553126729));
#29826=CARTESIAN_POINT('Ctrl Pts',(-41.9696960670028,37.6846655189277,38.5812599898182));
#29827=CARTESIAN_POINT('Ctrl Pts',(-41.982045165719,37.7017452276741,38.591777066537));
#29828=CARTESIAN_POINT('Ctrl Pts',(-41.9943110893787,37.7189381107715,38.6022054994369));
#29829=CARTESIAN_POINT('Ctrl Pts',(-42.0065770130384,37.7361309938689,38.6126339323367));
#29830=CARTESIAN_POINT('Ctrl Pts',(-42.018759761582,37.7534370511925,38.6229737213125));
#29831=CARTESIAN_POINT('Ctrl Pts',(-42.030858125247,37.7708545670661,38.6332238403209));
#29832=CARTESIAN_POINT('Ctrl Pts',(-42.0429564889119,37.7882720829396,38.6434739593292));
#29833=CARTESIAN_POINT('Ctrl Pts',(-42.0549704676829,37.8058010573424,38.6536344083581));
#29834=CARTESIAN_POINT('Ctrl Pts',(-42.0668988684252,37.8234397525212,38.6637041790089));
#29835=CARTESIAN_POINT('Ctrl Pts',(-42.0788272691675,37.8410784477,38.6737739496597));
#29836=CARTESIAN_POINT('Ctrl Pts',(-42.0906700918649,37.8588268636301,38.6837530419181));
#29837=CARTESIAN_POINT('Ctrl Pts',(-42.1024261602874,37.8766832409345,38.6936404653252));
#29838=CARTESIAN_POINT('Ctrl Pts',(-42.11418222871,37.8945396182387,38.7035278887324));
#29839=CARTESIAN_POINT('Ctrl Pts',(-42.1258515428427,37.9125039568964,38.7133236432767));
#29840=CARTESIAN_POINT('Ctrl Pts',(-42.1374329435463,37.9305744761275,38.7230267565294));
#29841=CARTESIAN_POINT('Ctrl Pts',(-42.1490143442499,37.9486449953587,38.7327298697821));
#29842=CARTESIAN_POINT('Ctrl Pts',(-42.1605078315089,37.9668216951379,38.7423403417292));
#29843=CARTESIAN_POINT('Ctrl Pts',(-42.1719122635506,37.9851027737687,38.751857218275));
#29844=CARTESIAN_POINT('Ctrl Pts',(-42.1833166955923,38.0033838523996,38.7613740948208));
#29845=CARTESIAN_POINT('Ctrl Pts',(-42.1946320723956,38.0217693098399,38.7707973759381));
#29846=CARTESIAN_POINT('Ctrl Pts',(-42.2058572697418,38.0402573237214,38.7801261259639));
#29847=CARTESIAN_POINT('Ctrl Pts',(-42.2170924433998,38.0587617686893,38.7894631668478));
#29848=CARTESIAN_POINT('Ctrl Pts',(-42.2282372772824,38.0773689526413,38.7987055086735));
#29849=CARTESIAN_POINT('Ctrl Pts',(-42.2392906618862,38.0960770276315,38.8078522316841));
#29850=CARTESIAN_POINT('Ctrl Pts',(-41.6343622916671,37.2841803659718,38.3097077240225));
#29851=CARTESIAN_POINT('Ctrl Pts',(-41.6486044484638,37.2998999854371,38.3222438581765));
#29852=CARTESIAN_POINT('Ctrl Pts',(-41.6627681091417,37.3157595051562,38.334693743636));
#29853=CARTESIAN_POINT('Ctrl Pts',(-41.6768517259748,37.3317571920888,38.3470560199468));
#29854=CARTESIAN_POINT('Ctrl Pts',(-41.690935342808,37.3477548790215,38.3594182962576));
#29855=CARTESIAN_POINT('Ctrl Pts',(-41.7049389157739,37.3638907331423,38.3716929633999));
#29856=CARTESIAN_POINT('Ctrl Pts',(-41.7188609146401,37.3801629912147,38.3838786800665));
#29857=CARTESIAN_POINT('Ctrl Pts',(-41.7327829135062,37.3964352492871,38.396064396733));
#29858=CARTESIAN_POINT('Ctrl Pts',(-41.7466233382503,37.4128439112853,38.4081611629044));
#29859=CARTESIAN_POINT('Ctrl Pts',(-41.7603806764678,37.429387184162,38.4201676567132));
#29860=CARTESIAN_POINT('Ctrl Pts',(-41.7741380146853,37.4459304570387,38.4321741505219));
#29861=CARTESIAN_POINT('Ctrl Pts',(-41.7878122663543,37.4626083407673,38.4440903719491));
#29862=CARTESIAN_POINT('Ctrl Pts',(-41.8014019372285,37.4794190128817,38.4559150188561));
#29863=CARTESIAN_POINT('Ctrl Pts',(-41.8149916081027,37.4962296849961,38.4677396657631));
#29864=CARTESIAN_POINT('Ctrl Pts',(-41.8284966981604,37.5131731454694,38.4794727381312));
#29865=CARTESIAN_POINT('Ctrl Pts',(-41.8419157316407,37.5302475428145,38.4911129538354));
#29866=CARTESIAN_POINT('Ctrl Pts',(-41.855334765121,37.5473219401595,38.5027531695397));
#29867=CARTESIAN_POINT('Ctrl Pts',(-41.8686677420024,37.5645272743491,38.5143005285616));
#29868=CARTESIAN_POINT('Ctrl Pts',(-41.8819132053312,37.58186166528,38.5257537690699));
#29869=CARTESIAN_POINT('Ctrl Pts',(-41.8951586686601,37.5991960562109,38.5372070095782));
#29870=CARTESIAN_POINT('Ctrl Pts',(-41.9083166184154,37.6166595038555,38.5485661315547));
#29871=CARTESIAN_POINT('Ctrl Pts',(-41.9213856167695,37.6342500999053,38.5598298937377));
#29872=CARTESIAN_POINT('Ctrl Pts',(-41.9344546151236,37.6518406959551,38.5710936559207));
#29873=CARTESIAN_POINT('Ctrl Pts',(-41.9474346620557,37.6695584403821,38.5822620582923));
#29874=CARTESIAN_POINT('Ctrl Pts',(-41.9603243391784,37.6874013970898,38.5933338804314));
#29875=CARTESIAN_POINT('Ctrl Pts',(-41.9732140163012,37.7052443537974,38.6044057025707));
#29876=CARTESIAN_POINT('Ctrl Pts',(-41.9860133235591,37.7232125226721,38.6153809443842));
#29877=CARTESIAN_POINT('Ctrl Pts',(-41.9987208623842,37.7413039404193,38.6262584067077));
#29878=CARTESIAN_POINT('Ctrl Pts',(-42.0114284012094,37.7593953581666,38.6371358690313));
#29879=CARTESIAN_POINT('Ctrl Pts',(-42.0240441715429,37.777610024664,38.6479155517638));
#29880=CARTESIAN_POINT('Ctrl Pts',(-42.0365667948123,37.7959459495368,38.658596276982));
#29881=CARTESIAN_POINT('Ctrl Pts',(-42.0490894180816,37.8142818744097,38.6692770022));
#29882=CARTESIAN_POINT('Ctrl Pts',(-42.0615188942673,37.8327390576306,38.6798587698879));
#29883=CARTESIAN_POINT('Ctrl Pts',(-42.0738538651359,37.8513154822757,38.6903404237066));
#29884=CARTESIAN_POINT('Ctrl Pts',(-42.0861888360046,37.8698919069209,38.7008220775252));
#29885=CARTESIAN_POINT('Ctrl Pts',(-42.0984293015361,37.8885875729586,38.7112036174569));
#29886=CARTESIAN_POINT('Ctrl Pts',(-42.1105739241704,37.9074004374591,38.7214839090885));
#29887=CARTESIAN_POINT('Ctrl Pts',(-42.1227185468047,37.9262133019595,38.7317642007201));
#29888=CARTESIAN_POINT('Ctrl Pts',(-42.1347673265229,37.9451433648946,38.7419432440364));
#29889=CARTESIAN_POINT('Ctrl Pts',(-42.1467189466908,37.964188557661,38.7520199267026));
#29890=CARTESIAN_POINT('Ctrl Pts',(-42.1586705668587,37.9832337504274,38.7620966093687));
#29891=CARTESIAN_POINT('Ctrl Pts',(-42.1705250274568,38.0023940729928,38.7720709313674));
#29892=CARTESIAN_POINT('Ctrl Pts',(-42.1822810331068,38.0216674316579,38.7819418027877));
#29893=CARTESIAN_POINT('Ctrl Pts',(-42.1940370387568,38.0409407903231,38.791812674208));
#29894=CARTESIAN_POINT('Ctrl Pts',(-42.2056945894344,38.0603271850404,38.8015800950206));
#29895=CARTESIAN_POINT('Ctrl Pts',(-42.2172524112672,38.0798244973725,38.811242997896));
#29896=CARTESIAN_POINT('Ctrl Pts',(-42.2288205050293,38.0993391377976,38.8209144886053));
#29897=CARTESIAN_POINT('Ctrl Pts',(-42.2402886926352,38.1189648932256,38.8304812756349));
#29898=CARTESIAN_POINT('Ctrl Pts',(-42.2516557185626,38.1386996149097,38.8399423114431));
#29899=CARTESIAN_POINT('Ctrl Pts',(-41.6248905220744,37.2849245869424,38.3195352797675));
#29900=CARTESIAN_POINT('Ctrl Pts',(-41.6397142976295,37.3013405039226,38.3326715088623));
#29901=CARTESIAN_POINT('Ctrl Pts',(-41.6544526590647,37.3179086508079,38.3457138880137));
#29902=CARTESIAN_POINT('Ctrl Pts',(-41.6691038594573,37.334627064395,38.3586608721299));
#29903=CARTESIAN_POINT('Ctrl Pts',(-41.6837550598498,37.3513454779822,38.3716078562462));
#29904=CARTESIAN_POINT('Ctrl Pts',(-41.6983190991723,37.36821415824,38.3844594453032));
#29905=CARTESIAN_POINT('Ctrl Pts',(-41.7127942510923,37.385231106464,38.397214116745));
#29906=CARTESIAN_POINT('Ctrl Pts',(-41.7272694030124,37.4022480546879,38.4099687881869));
#29907=CARTESIAN_POINT('Ctrl Pts',(-41.741655667503,37.4194132708462,38.4226265419898));
#29908=CARTESIAN_POINT('Ctrl Pts',(-41.755951339229,37.4367247212032,38.4351858784923));
#29909=CARTESIAN_POINT('Ctrl Pts',(-41.7702470109551,37.4540361715602,38.4477452149948));
#29910=CARTESIAN_POINT('Ctrl Pts',(-41.7844520898901,37.4714938560836,38.4602061341736));
#29911=CARTESIAN_POINT('Ctrl Pts',(-41.7985648920981,37.4890957064858,38.4725671596147));
#29912=CARTESIAN_POINT('Ctrl Pts',(-41.8126776943061,37.5066975568881,38.4849281850559));
#29913=CARTESIAN_POINT('Ctrl Pts',(-41.8266982197609,37.5244435731363,38.4971893167365));
#29914=CARTESIAN_POINT('Ctrl Pts',(-41.8406248063226,37.5423316528782,38.509349101838));
#29915=CARTESIAN_POINT('Ctrl Pts',(-41.8545513928842,37.5602197326201,38.5215088869395));
#29916=CARTESIAN_POINT('Ctrl Pts',(-41.8683840405269,37.5782498758223,38.5335673254393));
#29917=CARTESIAN_POINT('Ctrl Pts',(-41.8821211092983,37.5964199465627,38.5455229884566));
#29918=CARTESIAN_POINT('Ctrl Pts',(-41.8958581780698,37.6145900173031,38.5574786514739));
#29919=CARTESIAN_POINT('Ctrl Pts',(-41.9094996679445,37.6329000155479,38.5693315389865));
#29920=CARTESIAN_POINT('Ctrl Pts',(-41.9230439615446,37.6513477723083,38.5810802463877));
#29921=CARTESIAN_POINT('Ctrl Pts',(-41.9365882551445,37.6697955290687,38.5928289537889));
#29922=CARTESIAN_POINT('Ctrl Pts',(-41.9500353524446,37.6883810443104,38.6044734810568));
#29923=CARTESIAN_POINT('Ctrl Pts',(-41.9633836590221,37.7071021164888,38.61601244819));
#29924=CARTESIAN_POINT('Ctrl Pts',(-41.9767319655996,37.7258231886672,38.6275514153232));
#29925=CARTESIAN_POINT('Ctrl Pts',(-41.9899814813991,37.74467981767,38.6389848222313));
#29926=CARTESIAN_POINT('Ctrl Pts',(-42.0031306353897,37.7636697700671,38.6503113139786));
#29927=CARTESIAN_POINT('Ctrl Pts',(-42.0162797893803,37.7826597224643,38.6616378057259));
#29928=CARTESIAN_POINT('Ctrl Pts',(-42.0293285815038,37.8017829981353,38.6728573822152));
#29929=CARTESIAN_POINT('Ctrl Pts',(-42.0422754643776,37.8210373320075,38.683968713643));
#29930=CARTESIAN_POINT('Ctrl Pts',(-42.0552223472514,37.8402916658797,38.6950800450709));
#29931=CARTESIAN_POINT('Ctrl Pts',(-42.0680673208517,37.8596770579189,38.7060831314177));
#29932=CARTESIAN_POINT('Ctrl Pts',(-42.0808088618467,37.8791912120302,38.7169766684042));
#29933=CARTESIAN_POINT('Ctrl Pts',(-42.0935504028417,37.8987053661416,38.7278702053908));
#29934=CARTESIAN_POINT('Ctrl Pts',(-42.1061885112073,37.9183482822871,38.7386541929957));
#29935=CARTESIAN_POINT('Ctrl Pts',(-42.1187216880534,37.9381176339837,38.7493273528518));
#29936=CARTESIAN_POINT('Ctrl Pts',(-42.1312548648995,37.9578869856802,38.7600005127078));
#29937=CARTESIAN_POINT('Ctrl Pts',(-42.1436831102031,37.9777827728929,38.7705628447961));
#29938=CARTESIAN_POINT('Ctrl Pts',(-42.1560049498353,37.9978026391945,38.7810130968757));
#29939=CARTESIAN_POINT('Ctrl Pts',(-42.1683267894674,38.0178225054961,38.7914633489553));
#29940=CARTESIAN_POINT('Ctrl Pts',(-42.1805422234048,38.0379664508477,38.8018015210056));
#29941=CARTESIAN_POINT('Ctrl Pts',(-42.192649802663,38.0582320895472,38.8120263873004));
#29942=CARTESIAN_POINT('Ctrl Pts',(-42.2047573819213,38.0784977282466,38.8222512535952));
#29943=CARTESIAN_POINT('Ctrl Pts',(-42.2167571064732,38.0988850602409,38.832362814103));
#29944=CARTESIAN_POINT('Ctrl Pts',(-42.2286475527926,38.1193916710235,38.842359869828));
#29945=CARTESIAN_POINT('Ctrl Pts',(-42.2405485666589,38.1399165069059,38.8523658103628));
#29946=CARTESIAN_POINT('Ctrl Pts',(-42.2523401079879,38.1605608338099,38.8622570425963));
#29947=CARTESIAN_POINT('Ctrl Pts',(-42.264020775239,38.1813222021877,38.8720323912022));
#29948=CARTESIAN_POINT('Ctrl Pts',(-41.6153886967966,37.285633720554,38.3293332759128));
#29949=CARTESIAN_POINT('Ctrl Pts',(-41.6307648261287,37.3027135135746,38.3430436449347));
#29950=CARTESIAN_POINT('Ctrl Pts',(-41.6460484915149,37.3199581010959,38.3566524179197));
#29951=CARTESIAN_POINT('Ctrl Pts',(-41.6612377308598,37.3373652698898,38.3701578485853));
#29952=CARTESIAN_POINT('Ctrl Pts',(-41.6764269702048,37.3547724386838,38.3836632792508));
#29953=CARTESIAN_POINT('Ctrl Pts',(-41.6915217834752,37.3723421887124,38.3970653675675));
#29954=CARTESIAN_POINT('Ctrl Pts',(-41.7065202327379,37.3900722651408,38.4103623936964));
#29955=CARTESIAN_POINT('Ctrl Pts',(-41.7215186820006,37.4078023415691,38.4236594198254));
#29956=CARTESIAN_POINT('Ctrl Pts',(-41.7364207672228,37.4256927443586,38.4368513837376));
#29957=CARTESIAN_POINT('Ctrl Pts',(-41.7512245751282,37.4437411776422,38.4499365924771));
#29958=CARTESIAN_POINT('Ctrl Pts',(-41.7660283830335,37.4617896109258,38.4630218012165));
#29959=CARTESIAN_POINT('Ctrl Pts',(-41.7807339135895,37.4799960746643,38.4760002547544));
#29960=CARTESIAN_POINT('Ctrl Pts',(-41.7953392786647,37.4983582325443,38.488870287449));
#29961=CARTESIAN_POINT('Ctrl Pts',(-41.8099446437399,37.5167203904243,38.5017403201436));
#29962=CARTESIAN_POINT('Ctrl Pts',(-41.8244498433024,37.5352382424059,38.5145019319667));
#29963=CARTESIAN_POINT('Ctrl Pts',(-41.8388530148473,37.553909412325,38.5271534850154));
#29964=CARTESIAN_POINT('Ctrl Pts',(-41.8532561863922,37.5725805822442,38.539805038064));
#29965=CARTESIAN_POINT('Ctrl Pts',(-41.8675573298881,37.5914050700601,38.5523465323107));
#29966=CARTESIAN_POINT('Ctrl Pts',(-41.8817546089319,37.6103804603642,38.564776358009));
#29967=CARTESIAN_POINT('Ctrl Pts',(-41.8959518879759,37.6293558506681,38.5772061837074));
#29968=CARTESIAN_POINT('Ctrl Pts',(-41.9100453025368,37.6484821434189,38.5895243408303));
#29969=CARTESIAN_POINT('Ctrl Pts',(-41.9240330427824,37.6677568845784,38.601729248199));
#29970=CARTESIAN_POINT('Ctrl Pts',(-41.9380207830281,37.687031625738,38.6139341555677));
#29971=CARTESIAN_POINT('Ctrl Pts',(-41.9519028489279,37.7064548152644,38.6260258131555));
#29972=CARTESIAN_POINT('Ctrl Pts',(-41.9656774576819,37.7260239611165,38.6380026687541));
#29973=CARTESIAN_POINT('Ctrl Pts',(-41.979452066436,37.7455931069687,38.6499795243528));
#29974=CARTESIAN_POINT('Ctrl Pts',(-41.9931192180142,37.7653082091039,38.6618415779362));
#29975=CARTESIAN_POINT('Ctrl Pts',(-42.0066771571042,37.785166738113,38.6735873066626));
#29976=CARTESIAN_POINT('Ctrl Pts',(-42.0202350961943,37.8050252671221,38.6853330353891));
#29977=CARTESIAN_POINT('Ctrl Pts',(-42.0336838227664,37.8250272229619,38.696962439233));
#29978=CARTESIAN_POINT('Ctrl Pts',(-42.0470216094439,37.8451700394999,38.7084740251079));
#29979=CARTESIAN_POINT('Ctrl Pts',(-42.0603593961213,37.865312856038,38.7199856109827));
#29980=CARTESIAN_POINT('Ctrl Pts',(-42.0735862428749,37.8855965332304,38.7313793788634));
#29981=CARTESIAN_POINT('Ctrl Pts',(-42.0867004507042,37.9060184688758,38.7426538657995));
#29982=CARTESIAN_POINT('Ctrl Pts',(-42.0998146585335,37.9264404045212,38.7539283527356));
#29983=CARTESIAN_POINT('Ctrl Pts',(-42.1128162274098,37.9470005985752,38.7650835587024));
#29984=CARTESIAN_POINT('Ctrl Pts',(-42.1257034871429,37.9676964134305,38.7761180512591));
#29985=CARTESIAN_POINT('Ctrl Pts',(-42.138590746876,37.9883922282858,38.7871525438156));
#29986=CARTESIAN_POINT('Ctrl Pts',(-42.1513636974377,38.0092236638974,38.7980663229379));
#29987=CARTESIAN_POINT('Ctrl Pts',(-42.1640206978744,38.030188047925,38.8088579870595));
#29988=CARTESIAN_POINT('Ctrl Pts',(-42.176677698311,38.0511524319525,38.8196496511812));
#29989=CARTESIAN_POINT('Ctrl Pts',(-42.189218748595,38.0722497643502,38.8303192002788));
#29990=CARTESIAN_POINT('Ctrl Pts',(-42.2016422374281,38.0934773387253,38.8408652640187));
#29991=CARTESIAN_POINT('Ctrl Pts',(-42.2140657262613,38.1147049131006,38.8514113277587));
#29992=CARTESIAN_POINT('Ctrl Pts',(-42.2263716536165,38.136062729407,38.861833906118));
#29993=CARTESIAN_POINT('Ctrl Pts',(-42.2385584382627,38.1575480478897,38.8721316603454));
#29994=CARTESIAN_POINT('Ctrl Pts',(-42.2507560538243,38.1790524612914,38.8824385666263));
#29995=CARTESIAN_POINT('Ctrl Pts',(-42.2628343147816,38.2006846035563,38.8926204267812));
#29996=CARTESIAN_POINT('Ctrl Pts',(-42.2747916662362,38.2224416948671,38.9026759304956));
#29997=CARTESIAN_POINT('Ctrl Pts',(-41.6058635266892,37.286315601138,38.3391083125477));
#29998=CARTESIAN_POINT('Ctrl Pts',(-41.6217688958728,37.3040329697291,38.3533711969399));
#29999=CARTESIAN_POINT('Ctrl Pts',(-41.6375746651768,37.3219278508808,38.36752464459));
#30000=CARTESIAN_POINT('Ctrl Pts',(-41.6532786431145,37.3399977634488,38.3815666931073));
#30001=CARTESIAN_POINT('Ctrl Pts',(-41.6689826210522,37.3580676760168,38.3956087416246));
#30002=CARTESIAN_POINT('Ctrl Pts',(-41.6845848075833,37.3763126199546,38.4095393909731));
#30003=CARTESIAN_POINT('Ctrl Pts',(-41.7000830394478,37.3947300655812,38.4233567096532));
#30004=CARTESIAN_POINT('Ctrl Pts',(-41.7155812713123,37.4131475112078,38.4371740283333));
#30005=CARTESIAN_POINT('Ctrl Pts',(-41.7309755484705,37.4317374584759,38.4508780163097));
#30006=CARTESIAN_POINT('Ctrl Pts',(-41.7462637364893,37.4504973298695,38.4644667735097));
#30007=CARTESIAN_POINT('Ctrl Pts',(-41.7615519245081,37.4692572012631,38.4780555307096));
#30008=CARTESIAN_POINT('Ctrl Pts',(-41.7767340233484,37.4881869967341,38.4915290570984));
#30009=CARTESIAN_POINT('Ctrl Pts',(-41.7918079279958,37.5072840916458,38.5048854845569));
#30010=CARTESIAN_POINT('Ctrl Pts',(-41.8068818326432,37.5263811865576,38.5182419120155));
#30011=CARTESIAN_POINT('Ctrl Pts',(-41.8218475430591,37.5456455808612,38.5314812405097));
#30012=CARTESIAN_POINT('Ctrl Pts',(-41.8367029842316,37.5650746035277,38.5446016343923));
#30013=CARTESIAN_POINT('Ctrl Pts',(-41.8515584254041,37.5845036261943,38.5577220282749));
#30014=CARTESIAN_POINT('Ctrl Pts',(-41.8663035972952,37.6040972771739,38.5707234875124));
#30015=CARTESIAN_POINT('Ctrl Pts',(-41.8809364554709,37.6238528397859,38.5836042094385));
#30016=CARTESIAN_POINT('Ctrl Pts',(-41.8955693136467,37.6436084023978,38.5964849313646));
#30017=CARTESIAN_POINT('Ctrl Pts',(-41.9100898580695,37.6635258765915,38.6092449159461));
#30018=CARTESIAN_POINT('Ctrl Pts',(-41.9244960754504,37.6836025007876,38.6218823939976));
#30019=CARTESIAN_POINT('Ctrl Pts',(-41.9389022928313,37.7036791249839,38.6345198720492));
#30020=CARTESIAN_POINT('Ctrl Pts',(-41.9531941831333,37.723914899131,38.6470348435383));
#30021=CARTESIAN_POINT('Ctrl Pts',(-41.9673697647705,37.7443070175174,38.6594255732507));
#30022=CARTESIAN_POINT('Ctrl Pts',(-41.9815453464077,37.7646991359038,38.6718163029631));
#30023=CARTESIAN_POINT('Ctrl Pts',(-41.9956046193437,37.7852475984771,38.6840827908671));
#30024=CARTESIAN_POINT('Ctrl Pts',(-42.0095456342452,37.8059495561709,38.6962233362008));
#30025=CARTESIAN_POINT('Ctrl Pts',(-42.0234866491467,37.8266515138647,38.7083638815347));
#30026=CARTESIAN_POINT('Ctrl Pts',(-42.037309405978,37.847506966626,38.7203784842671));
#30027=CARTESIAN_POINT('Ctrl Pts',(-42.051011988199,37.8685130228238,38.7322654785607));
#30028=CARTESIAN_POINT('Ctrl Pts',(-42.0647145704201,37.8895190790215,38.7441524728544));
#30029=CARTESIAN_POINT('Ctrl Pts',(-42.0782969779956,37.9106757386019,38.7559118586786));
#30030=CARTESIAN_POINT('Ctrl Pts',(-42.0917573277104,37.9319800681713,38.7675420055821));
#30031=CARTESIAN_POINT('Ctrl Pts',(-42.1052176774251,37.9532843977408,38.7791721524855));
#30032=CARTESIAN_POINT('Ctrl Pts',(-42.1185559692445,37.9747363972447,38.7906730604383));
#30033=CARTESIAN_POINT('Ctrl Pts',(-42.1317703538001,37.9963330923403,38.8020431348271));
#30034=CARTESIAN_POINT('Ctrl Pts',(-42.1449847383556,38.0179297874359,38.813413209216));
#30035=CARTESIAN_POINT('Ctrl Pts',(-42.1580752156135,38.0396711780678,38.8246524500119));
#30036=CARTESIAN_POINT('Ctrl Pts',(-42.1710399705648,38.0615542497689,38.8357592988819));
#30037=CARTESIAN_POINT('Ctrl Pts',(-42.1840047255163,38.0834373214698,38.8468661477519));
#30038=CARTESIAN_POINT('Ctrl Pts',(-42.196843758128,38.1054620741839,38.8578406046676));
#30039=CARTESIAN_POINT('Ctrl Pts',(-42.2095552882544,38.1276254541553,38.8686811480087));
#30040=CARTESIAN_POINT('Ctrl Pts',(-42.2222668183807,38.1497888341268,38.8795216913498));
#30041=CARTESIAN_POINT('Ctrl Pts',(-42.2348508459891,38.1720908412988,38.8902283210885));
#30042=CARTESIAN_POINT('Ctrl Pts',(-42.2473056262907,38.1945283834742,38.9007995527392));
#30043=CARTESIAN_POINT('Ctrl Pts',(-42.2597714756867,38.2169858668503,38.9113801794943));
#30044=CARTESIAN_POINT('Ctrl Pts',(-42.2721078479066,38.2395791261907,38.9218251673591));
#30045=CARTESIAN_POINT('Ctrl Pts',(-42.2843130294414,38.2623050233617,38.9321330655328));
#30046=CARTESIAN_POINT('Ctrl Pts',(-41.5963383565818,37.286997481722,38.3488833491826));
#30047=CARTESIAN_POINT('Ctrl Pts',(-41.6127729656169,37.3053524258835,38.3636987489452));
#30048=CARTESIAN_POINT('Ctrl Pts',(-41.6291008388388,37.3238976006658,38.3783968712603));
#30049=CARTESIAN_POINT('Ctrl Pts',(-41.6453195553693,37.3426302570077,38.3929755376294));
#30050=CARTESIAN_POINT('Ctrl Pts',(-41.6615382718997,37.3613629133496,38.4075542039984));
#30051=CARTESIAN_POINT('Ctrl Pts',(-41.6776478316914,37.3802830511966,38.4220134143787));
#30052=CARTESIAN_POINT('Ctrl Pts',(-41.6936458461577,37.3993878660215,38.43635102561));
#30053=CARTESIAN_POINT('Ctrl Pts',(-41.7096438606239,37.4184926808463,38.4506886368413));
#30054=CARTESIAN_POINT('Ctrl Pts',(-41.725530329718,37.4377821725933,38.4649046488818));
#30055=CARTESIAN_POINT('Ctrl Pts',(-41.7413028978504,37.4572534820969,38.4789969545423));
#30056=CARTESIAN_POINT('Ctrl Pts',(-41.7570754659828,37.4767247916005,38.4930892602028));
#30057=CARTESIAN_POINT('Ctrl Pts',(-41.7727341331073,37.4963779188038,38.5070578594423));
#30058=CARTESIAN_POINT('Ctrl Pts',(-41.7882765773269,37.5162099507473,38.5209006816648));
#30059=CARTESIAN_POINT('Ctrl Pts',(-41.8038190215465,37.5360419826907,38.5347435038874));
#30060=CARTESIAN_POINT('Ctrl Pts',(-41.8192452428157,37.5560529193164,38.5484605490526));
#30061=CARTESIAN_POINT('Ctrl Pts',(-41.8345529536159,37.5762397947304,38.5620497837692));
#30062=CARTESIAN_POINT('Ctrl Pts',(-41.849860664416,37.5964266701443,38.5756390184859));
#30063=CARTESIAN_POINT('Ctrl Pts',(-41.8650498647023,37.6167894842876,38.5891004427142));
#30064=CARTESIAN_POINT('Ctrl Pts',(-41.8801183020099,37.6373252192075,38.602432060868));
#30065=CARTESIAN_POINT('Ctrl Pts',(-41.8951867393174,37.6578609541275,38.6157636790217));
#30066=CARTESIAN_POINT('Ctrl Pts',(-41.9101344136022,37.6785696097642,38.6289654910619));
#30067=CARTESIAN_POINT('Ctrl Pts',(-41.9249591081184,37.6994481169969,38.6420355397963));
#30068=CARTESIAN_POINT('Ctrl Pts',(-41.9397838026345,37.7203266242297,38.6551055885306));
#30069=CARTESIAN_POINT('Ctrl Pts',(-41.9544855173388,37.7413749829976,38.668043873921));
#30070=CARTESIAN_POINT('Ctrl Pts',(-41.9690620718591,37.7625900739183,38.6808484777472));
#30071=CARTESIAN_POINT('Ctrl Pts',(-41.9836386263794,37.7838051648389,38.6936530815734));
#30072=CARTESIAN_POINT('Ctrl Pts',(-41.9980900206732,37.8051869878503,38.706324003798));
#30073=CARTESIAN_POINT('Ctrl Pts',(-42.0124141113862,37.8267323742288,38.7188593657391));
#30074=CARTESIAN_POINT('Ctrl Pts',(-42.0267382020992,37.8482777606074,38.7313947276802));
#30075=CARTESIAN_POINT('Ctrl Pts',(-42.0409349891896,37.8699867102901,38.7437945293013));
#30076=CARTESIAN_POINT('Ctrl Pts',(-42.0550023669542,37.8918560061476,38.7560569320136));
#30077=CARTESIAN_POINT('Ctrl Pts',(-42.0690697447188,37.913725302005,38.768319334726));
#30078=CARTESIAN_POINT('Ctrl Pts',(-42.0830077131163,37.9357549439734,38.7804443384939));
#30079=CARTESIAN_POINT('Ctrl Pts',(-42.0968142047165,37.9579416674669,38.7924301453646));
#30080=CARTESIAN_POINT('Ctrl Pts',(-42.1106206963167,37.9801283909604,38.8044159522353));
#30081=CARTESIAN_POINT('Ctrl Pts',(-42.1242957110792,38.0024721959143,38.8162625621741));
#30082=CARTESIAN_POINT('Ctrl Pts',(-42.1378372204572,38.0249697712501,38.8279682183953));
#30083=CARTESIAN_POINT('Ctrl Pts',(-42.1513787298352,38.047467346586,38.8396738746164));
#30084=CARTESIAN_POINT('Ctrl Pts',(-42.1647867337893,38.0701186922381,38.851238577086));
#30085=CARTESIAN_POINT('Ctrl Pts',(-42.1780592432554,38.0929204516126,38.8626606107043));
#30086=CARTESIAN_POINT('Ctrl Pts',(-42.1913317527215,38.1157222109872,38.8740826443226));
#30087=CARTESIAN_POINT('Ctrl Pts',(-42.204468767661,38.1386743840176,38.8853620090564));
#30088=CARTESIAN_POINT('Ctrl Pts',(-42.2174683390806,38.1617735695853,38.8964970319986));
#30089=CARTESIAN_POINT('Ctrl Pts',(-42.2304679105001,38.1848727551531,38.9076320549408));
#30090=CARTESIAN_POINT('Ctrl Pts',(-42.2433300383618,38.2081189531906,38.9186227360591));
#30091=CARTESIAN_POINT('Ctrl Pts',(-42.2560528143186,38.2315087190587,38.9294674451329));
#30092=CARTESIAN_POINT('Ctrl Pts',(-42.2687868975491,38.2549192724092,38.9403217923623));
#30093=CARTESIAN_POINT('Ctrl Pts',(-42.2813813810315,38.278473648825,38.9510299079371));
#30094=CARTESIAN_POINT('Ctrl Pts',(-42.2938343926466,38.3021683518564,38.9615902005701));
#30095=CARTESIAN_POINT('Ctrl Pts',(-41.5867897802837,37.2876520376445,38.3586353659586));
#30096=CARTESIAN_POINT('Ctrl Pts',(-41.6037304885494,37.3066182518131,38.3739816725687));
#30097=CARTESIAN_POINT('Ctrl Pts',(-41.620557238131,37.3257875696053,38.3892027655024));
#30098=CARTESIAN_POINT('Ctrl Pts',(-41.6372673645311,37.3451569561447,38.4042962352317));
#30099=CARTESIAN_POINT('Ctrl Pts',(-41.6539774909312,37.3645263426841,38.4193897049609));
#30100=CARTESIAN_POINT('Ctrl Pts',(-41.6705709940942,37.3840957979064,38.4343555514354));
#30101=CARTESIAN_POINT('Ctrl Pts',(-41.6870452463718,37.4038622237152,38.4491914054513));
#30102=CARTESIAN_POINT('Ctrl Pts',(-41.7035194986494,37.4236286495241,38.4640272594672));
#30103=CARTESIAN_POINT('Ctrl Pts',(-41.7198744999866,37.4435920458539,38.4787331209752));
#30104=CARTESIAN_POINT('Ctrl Pts',(-41.7361076604127,37.4637492523649,38.493306661843));
#30105=CARTESIAN_POINT('Ctrl Pts',(-41.7523408208388,37.483906458876,38.5078802027108));
#30106=CARTESIAN_POINT('Ctrl Pts',(-41.7684521402996,37.5042574755014,38.5223214228898));
#30107=CARTESIAN_POINT('Ctrl Pts',(-41.7844390673187,37.5247990806544,38.5366280360533));
#30108=CARTESIAN_POINT('Ctrl Pts',(-41.8004259943379,37.5453406858074,38.5509346492168));
#30109=CARTESIAN_POINT('Ctrl Pts',(-41.8162885288619,37.5660728794197,38.5651066553171));
#30110=CARTESIAN_POINT('Ctrl Pts',(-41.8320241587134,37.5869923796731,38.5791418105536));
#30111=CARTESIAN_POINT('Ctrl Pts',(-41.8477597885648,37.6079118799265,38.59317696579));
#30112=CARTESIAN_POINT('Ctrl Pts',(-41.8633685136913,37.6290186867515,38.6070752701159));
#30113=CARTESIAN_POINT('Ctrl Pts',(-41.8788478620063,37.6503094591325,38.6208345229642));
#30114=CARTESIAN_POINT('Ctrl Pts',(-41.8943272103213,37.6716002315136,38.6345937758125));
#30115=CARTESIAN_POINT('Ctrl Pts',(-41.9096771817734,37.69307496938,38.6482139771374));
#30116=CARTESIAN_POINT('Ctrl Pts',(-41.924895345147,37.7147302735725,38.6616929702995));
#30117=CARTESIAN_POINT('Ctrl Pts',(-41.9401135085206,37.736385577765,38.6751719634615));
#30118=CARTESIAN_POINT('Ctrl Pts',(-41.9551998637651,37.7582214482115,38.6885097484157));
#30119=CARTESIAN_POINT('Ctrl Pts',(-41.9701520213029,37.7802344286799,38.7017042131301));
#30120=CARTESIAN_POINT('Ctrl Pts',(-41.9851041788406,37.8022474091484,38.7148986778445));
#30121=CARTESIAN_POINT('Ctrl Pts',(-41.9999221386806,37.8244374997358,38.7279498224257));
#30122=CARTESIAN_POINT('Ctrl Pts',(-42.0146035535198,37.8468011878927,38.7408555798182));
#30123=CARTESIAN_POINT('Ctrl Pts',(-42.029284968359,37.8691648760496,38.7537613372108));
#30124=CARTESIAN_POINT('Ctrl Pts',(-42.0438298382064,37.8917021618657,38.766521707518));
#30125=CARTESIAN_POINT('Ctrl Pts',(-42.058235859008,37.9144094782492,38.7791346699066));
#30126=CARTESIAN_POINT('Ctrl Pts',(-42.0726418798095,37.9371167946327,38.7917476322951));
#30127=CARTESIAN_POINT('Ctrl Pts',(-42.0869090515172,37.9599941415081,38.8042131867229));
#30128=CARTESIAN_POINT('Ctrl Pts',(-42.1010351139354,37.9830378980317,38.8165293589193));
#30129=CARTESIAN_POINT('Ctrl Pts',(-42.1151611763537,38.0060816545551,38.8288455311156));
#30130=CARTESIAN_POINT('Ctrl Pts',(-42.1291461294356,38.0292918206501,38.8410123210396));
#30131=CARTESIAN_POINT('Ctrl Pts',(-42.1429877575575,38.0526647228616,38.8530278016054));
#30132=CARTESIAN_POINT('Ctrl Pts',(-42.1568293856795,38.0760376250732,38.8650432821713));
#30133=CARTESIAN_POINT('Ctrl Pts',(-42.1705276887953,38.0995732633236,38.8769074533392));
#30134=CARTESIAN_POINT('Ctrl Pts',(-42.1840804965524,38.1232679127047,38.8886184358165));
#30135=CARTESIAN_POINT('Ctrl Pts',(-42.1976333043096,38.1469625620857,38.900329418294));
#30136=CARTESIAN_POINT('Ctrl Pts',(-42.2110406166629,38.1708162225187,38.9118872120419));
#30137=CARTESIAN_POINT('Ctrl Pts',(-42.2243003092155,38.1948251188158,38.9232899861538));
#30138=CARTESIAN_POINT('Ctrl Pts',(-42.2375600017681,38.218834015113,38.9346927602656));
#30139=CARTESIAN_POINT('Ctrl Pts',(-42.2506720744758,38.2429981471945,38.9459405147036));
#30140=CARTESIAN_POINT('Ctrl Pts',(-42.2636344495679,38.2673136907831,38.9570314675243));
#30141=CARTESIAN_POINT('Ctrl Pts',(-42.2766083448756,38.2916508446324,38.968132277348));
#30142=CARTESIAN_POINT('Ctrl Pts',(-42.2894322762548,38.3161396788477,38.9790760064518));
#30143=CARTESIAN_POINT('Ctrl Pts',(-42.3021042079305,38.3407763115497,38.9898609182514));
#30144=CARTESIAN_POINT('Ctrl Pts',(-41.5772224901889,37.2882847468617,38.3683689778196));
#30145=CARTESIAN_POINT('Ctrl Pts',(-41.5946507223381,37.3078407290261,38.3842282194709));
#30146=CARTESIAN_POINT('Ctrl Pts',(-41.6119577122494,37.327612795967,38.3999542445415));
#30147=CARTESIAN_POINT('Ctrl Pts',(-41.6291405389079,37.3475976106221,38.4155443988461));
#30148=CARTESIAN_POINT('Ctrl Pts',(-41.6463233655664,37.3675824252771,38.4311345531509));
#30149=CARTESIAN_POINT('Ctrl Pts',(-41.663382028907,37.3877799875703,38.4465888366305));
#30150=CARTESIAN_POINT('Ctrl Pts',(-41.6803136498262,37.4081868886259,38.4619046409637));
#30151=CARTESIAN_POINT('Ctrl Pts',(-41.6972452707455,37.4285937896815,38.4772204452969));
#30152=CARTESIAN_POINT('Ctrl Pts',(-41.7140498491792,37.4492100294219,38.4923977704254));
#30153=CARTESIAN_POINT('Ctrl Pts',(-41.7307245489078,37.4700321283081,38.5074340547719));
#30154=CARTESIAN_POINT('Ctrl Pts',(-41.7473992486363,37.4908542271945,38.5224703391184));
#30155=CARTESIAN_POINT('Ctrl Pts',(-41.7639440695964,37.5118821851476,38.5373655826258));
#30156=CARTESIAN_POINT('Ctrl Pts',(-41.7803562194093,37.5331124531404,38.5521172713255));
#30157=CARTESIAN_POINT('Ctrl Pts',(-41.7967683692221,37.5543427211332,38.5668689600252));
#30158=CARTESIAN_POINT('Ctrl Pts',(-41.8130478478255,37.5757752990849,38.5814770938612));
#30159=CARTESIAN_POINT('Ctrl Pts',(-41.8291919076243,37.5974065696779,38.5959392073223));
#30160=CARTESIAN_POINT('Ctrl Pts',(-41.8453359674232,37.6190378402709,38.6104013207834));
#30161=CARTESIAN_POINT('Ctrl Pts',(-41.8613446083561,37.6408678034231,38.6247174138146));
#30162=CARTESIAN_POINT('Ctrl Pts',(-41.8772151285393,37.6628927747474,38.6388850701946));
#30163=CARTESIAN_POINT('Ctrl Pts',(-41.8930856487224,37.6849177460716,38.6530527265745));
#30164=CARTESIAN_POINT('Ctrl Pts',(-41.9088180480953,37.7071377254845,38.6670719462493));
#30165=CARTESIAN_POINT('Ctrl Pts',(-41.9244096713972,37.7295489627732,38.6809403631027));
#30166=CARTESIAN_POINT('Ctrl Pts',(-41.9400012946991,37.7519602000619,38.694808779956));
#30167=CARTESIAN_POINT('Ctrl Pts',(-41.9554521418707,37.7745626951413,38.7085263939354));
#30168=CARTESIAN_POINT('Ctrl Pts',(-41.9707596051706,37.7973526332393,38.7220908898283));
#30169=CARTESIAN_POINT('Ctrl Pts',(-41.9860670684705,37.8201425713374,38.7356553857213));
#30170=CARTESIAN_POINT('Ctrl Pts',(-42.001231147894,37.8431199525268,38.7490667636172));
#30171=CARTESIAN_POINT('Ctrl Pts',(-42.016249283993,37.8662808984502,38.7623227597117));
#30172=CARTESIAN_POINT('Ctrl Pts',(-42.031267420092,37.8894418443737,38.7755787558061));
#30173=CARTESIAN_POINT('Ctrl Pts',(-42.0461396128623,37.9127863550969,38.7886793701855));
#30174=CARTESIAN_POINT('Ctrl Pts',(-42.0608633522257,37.9363104906126,38.8016223917728));
#30175=CARTESIAN_POINT('Ctrl Pts',(-42.075587091589,37.9598346261284,38.81456541336));
#30176=CARTESIAN_POINT('Ctrl Pts',(-42.0901623774896,37.9835383863474,38.8273508421058));
#30177=CARTESIAN_POINT('Ctrl Pts',(-42.1045867499601,38.0074177706295,38.8399765201292));
#30178=CARTESIAN_POINT('Ctrl Pts',(-42.1190111224306,38.0312971549117,38.8526021981525));
#30179=CARTESIAN_POINT('Ctrl Pts',(-42.1332845814163,38.0553521631663,38.8650681254053));
#30180=CARTESIAN_POINT('Ctrl Pts',(-42.1474047178913,38.0795787354709,38.8773721979308));
#30181=CARTESIAN_POINT('Ctrl Pts',(-42.1615248543663,38.1038053077755,38.8896762704562));
#30182=CARTESIAN_POINT('Ctrl Pts',(-42.175491668277,38.128203444038,38.9018184882076));
#30183=CARTESIAN_POINT('Ctrl Pts',(-42.1893028023519,38.1527690264238,38.9137968018627));
#30184=CARTESIAN_POINT('Ctrl Pts',(-42.2031139364269,38.1773346088097,38.9257751155178));
#30185=CARTESIAN_POINT('Ctrl Pts',(-42.2167693906136,38.2020676372257,38.9375895250311));
#30186=CARTESIAN_POINT('Ctrl Pts',(-42.2302668601911,38.2269639373153,38.9492380364066));
#30187=CARTESIAN_POINT('Ctrl Pts',(-42.2437643297685,38.2518602374049,38.9608865477822));
#30188=CARTESIAN_POINT('Ctrl Pts',(-42.2571038146854,38.2769198090737,38.9723691609758));
#30189=CARTESIAN_POINT('Ctrl Pts',(-42.2702830635487,38.302138422852,38.9836839379911));
#30190=CARTESIAN_POINT('Ctrl Pts',(-42.2834740253727,38.3273794494882,38.9950087709313));
#30191=CARTESIAN_POINT('Ctrl Pts',(-42.2965044660913,38.3527798006676,39.0061654689777));
#30192=CARTESIAN_POINT('Ctrl Pts',(-42.3093721826523,38.378335182382,39.0171521461915));
#30193=CARTESIAN_POINT('Ctrl Pts',(-41.5676552000942,37.2889174560789,38.3781025896805));
#30194=CARTESIAN_POINT('Ctrl Pts',(-41.5855709561268,37.3090632062391,38.3944747663732));
#30195=CARTESIAN_POINT('Ctrl Pts',(-41.6033581863678,37.3294380223288,38.4107057235805));
#30196=CARTESIAN_POINT('Ctrl Pts',(-41.6210137132847,37.3500382650995,38.4267925624606));
#30197=CARTESIAN_POINT('Ctrl Pts',(-41.6386692402017,37.3706385078701,38.4428794013408));
#30198=CARTESIAN_POINT('Ctrl Pts',(-41.6561930637196,37.3914641772344,38.4588221218257));
#30199=CARTESIAN_POINT('Ctrl Pts',(-41.6735820532807,37.4125115535366,38.4746178764762));
#30200=CARTESIAN_POINT('Ctrl Pts',(-41.6909710428417,37.4335589298388,38.4904136311266));
#30201=CARTESIAN_POINT('Ctrl Pts',(-41.7082251983718,37.4548280129899,38.5060624198756));
#30202=CARTESIAN_POINT('Ctrl Pts',(-41.7253414374028,37.4763150042514,38.5215614477008));
#30203=CARTESIAN_POINT('Ctrl Pts',(-41.7424576764339,37.4978019955129,38.5370604755261));
#30204=CARTESIAN_POINT('Ctrl Pts',(-41.759435998893,37.519506894794,38.5524097423618));
#30205=CARTESIAN_POINT('Ctrl Pts',(-41.7762733714997,37.5414258256264,38.5676065065977));
#30206=CARTESIAN_POINT('Ctrl Pts',(-41.7931107441064,37.563344756459,38.5828032708336));
#30207=CARTESIAN_POINT('Ctrl Pts',(-41.8098071667891,37.5854777187501,38.5978475324052));
#30208=CARTESIAN_POINT('Ctrl Pts',(-41.8263596565353,37.6078207596827,38.612736604091));
#30209=CARTESIAN_POINT('Ctrl Pts',(-41.8429121462815,37.6301638006153,38.6276256757767));
#30210=CARTESIAN_POINT('Ctrl Pts',(-41.859320703021,37.6527169200947,38.6423595575134));
#30211=CARTESIAN_POINT('Ctrl Pts',(-41.8755823950722,37.6754760903623,38.6569356174249));
#30212=CARTESIAN_POINT('Ctrl Pts',(-41.8918440871234,37.6982352606297,38.6715116773365));
#30213=CARTESIAN_POINT('Ctrl Pts',(-41.9079589144172,37.7212004815889,38.6859299153611));
#30214=CARTESIAN_POINT('Ctrl Pts',(-41.9239239976474,37.7443676519738,38.7001877559059));
#30215=CARTESIAN_POINT('Ctrl Pts',(-41.9398890808776,37.7675348223587,38.7144455964506));
#30216=CARTESIAN_POINT('Ctrl Pts',(-41.9557044199763,37.7909039420712,38.728543039455));
#30217=CARTESIAN_POINT('Ctrl Pts',(-41.9713671890384,37.8144708377988,38.7424775665265));
#30218=CARTESIAN_POINT('Ctrl Pts',(-41.9870299581004,37.8380377335264,38.756412093598));
#30219=CARTESIAN_POINT('Ctrl Pts',(-42.0025401571074,37.8618024053179,38.7701837048088));
#30220=CARTESIAN_POINT('Ctrl Pts',(-42.0178950144663,37.8857606090078,38.7837899396051));
#30221=CARTESIAN_POINT('Ctrl Pts',(-42.0332498718251,37.9097188126977,38.7973961744014));
#30222=CARTESIAN_POINT('Ctrl Pts',(-42.0484493875181,37.933870548328,38.810837032853));
#30223=CARTESIAN_POINT('Ctrl Pts',(-42.0634908454433,37.958211502976,38.824110113639));
#30224=CARTESIAN_POINT('Ctrl Pts',(-42.0785323033685,37.9825524576241,38.8373831944249));
#30225=CARTESIAN_POINT('Ctrl Pts',(-42.093415703462,38.0070826311866,38.8504884974888));
#30226=CARTESIAN_POINT('Ctrl Pts',(-42.1081383859847,38.0317976432275,38.8634236813391));
#30227=CARTESIAN_POINT('Ctrl Pts',(-42.1228610685075,38.0565126552683,38.8763588651893));
#30228=CARTESIAN_POINT('Ctrl Pts',(-42.1374230333971,38.0814125056826,38.8891239297711));
#30229=CARTESIAN_POINT('Ctrl Pts',(-42.1518216782251,38.1064927480802,38.9017165942561));
#30230=CARTESIAN_POINT('Ctrl Pts',(-42.1662203230532,38.1315729904777,38.9143092587412));
#30231=CARTESIAN_POINT('Ctrl Pts',(-42.1804556477587,38.1568336247523,38.9267295230761));
#30232=CARTESIAN_POINT('Ctrl Pts',(-42.1945251081514,38.182270140143,38.9389751679089));
#30233=CARTESIAN_POINT('Ctrl Pts',(-42.2085945685441,38.2077066555336,38.9512208127417));
#30234=CARTESIAN_POINT('Ctrl Pts',(-42.2224981645643,38.2333190519327,38.9632918380203));
#30235=CARTESIAN_POINT('Ctrl Pts',(-42.2362334111666,38.2591027558148,38.9751860866595));
#30236=CARTESIAN_POINT('Ctrl Pts',(-42.2499686577689,38.2848864596969,38.9870803352988));
#30237=CARTESIAN_POINT('Ctrl Pts',(-42.2635355548949,38.3108414709527,38.9987978072482));
#30238=CARTESIAN_POINT('Ctrl Pts',(-42.2769316775296,38.3369631549211,39.0103364084579));
#30239=CARTESIAN_POINT('Ctrl Pts',(-42.2903397058698,38.3631080543441,39.0218852645147));
#30240=CARTESIAN_POINT('Ctrl Pts',(-42.3035766559278,38.3894199224876,39.0332549315036));
#30241=CARTESIAN_POINT('Ctrl Pts',(-42.3166401573741,38.4158940532142,39.0444433741316));
#30242=CARTESIAN_POINT('Ctrl Pts',(-41.5580691595818,37.2895282758387,38.3878177606096));
#30243=CARTESIAN_POINT('Ctrl Pts',(-41.576453838129,37.3102422736121,38.4046848944203));
#30244=CARTESIAN_POINT('Ctrl Pts',(-41.5947026462334,37.3311984273574,38.4214027387092));
#30245=CARTESIAN_POINT('Ctrl Pts',(-41.6128121369395,37.3523927792619,38.4379681363462));
#30246=CARTESIAN_POINT('Ctrl Pts',(-41.6309216276457,37.3735871311664,38.4545335339833));
#30247=CARTESIAN_POINT('Ctrl Pts',(-41.6488918008674,37.39501968113,38.4709464848899));
#30248=CARTESIAN_POINT('Ctrl Pts',(-41.6667192621919,37.4166863814999,38.4872038894299));
#30249=CARTESIAN_POINT('Ctrl Pts',(-41.6845467235163,37.4383530818698,38.5034612939699));
#30250=CARTESIAN_POINT('Ctrl Pts',(-41.7022314728587,37.4602539325432,38.5195631520664));
#30251=CARTESIAN_POINT('Ctrl Pts',(-41.7197701696272,37.482384797551,38.5355064227447));
#30252=CARTESIAN_POINT('Ctrl Pts',(-41.7373088663957,37.5045156625588,38.551449693423));
#30253=CARTESIAN_POINT('Ctrl Pts',(-41.754701510507,37.5268765417961,38.5672343766076));
#30254=CARTESIAN_POINT('Ctrl Pts',(-41.7719448164483,37.5494632125342,38.5828574911305));
#30255=CARTESIAN_POINT('Ctrl Pts',(-41.7891881223896,37.5720498832724,38.5984806056533));
#30256=CARTESIAN_POINT('Ctrl Pts',(-41.8062820900792,37.5948623454045,38.6139421514404));
#30257=CARTESIAN_POINT('Ctrl Pts',(-41.8232234903209,37.6178962910326,38.6292392082528));
#30258=CARTESIAN_POINT('Ctrl Pts',(-41.8401648905627,37.6409302366608,38.6445362650652));
#30259=CARTESIAN_POINT('Ctrl Pts',(-41.8569537232762,37.6641856656757,38.6596688328305));
#30260=CARTESIAN_POINT('Ctrl Pts',(-41.8735868167985,37.6876581866323,38.6746340533385));
#30261=CARTESIAN_POINT('Ctrl Pts',(-41.8902199103208,37.7111307075889,38.6895992738465));
#30262=CARTESIAN_POINT('Ctrl Pts',(-41.9066972645729,37.7348203203759,38.7043971470262));
#30263=CARTESIAN_POINT('Ctrl Pts',(-41.9230157666195,37.7587225516539,38.7190248777729));
#30264=CARTESIAN_POINT('Ctrl Pts',(-41.939334268666,37.782624782932,38.7336526085196));
#30265=CARTESIAN_POINT('Ctrl Pts',(-41.9554939184296,37.8067396325878,38.7481101967638));
#30266=CARTESIAN_POINT('Ctrl Pts',(-41.971491662875,37.8310625470722,38.7623949115585));
#30267=CARTESIAN_POINT('Ctrl Pts',(-41.9874894073204,37.8553854615566,38.7766796263532));
#30268=CARTESIAN_POINT('Ctrl Pts',(-42.0033252463718,37.8799164407544,38.7907914676305));
#30269=CARTESIAN_POINT('Ctrl Pts',(-42.0189961880445,37.9046508526205,38.8047277696299));
#30270=CARTESIAN_POINT('Ctrl Pts',(-42.0346671297171,37.9293852644866,38.8186640716294));
#30271=CARTESIAN_POINT('Ctrl Pts',(-42.0501731739366,37.9543231089039,38.8324248342847));
#30272=CARTESIAN_POINT('Ctrl Pts',(-42.0655113908957,37.9794596770759,38.8460074580256));
#30273=CARTESIAN_POINT('Ctrl Pts',(-42.0808496078549,38.0045962452478,38.8595900817665));
#30274=CARTESIAN_POINT('Ctrl Pts',(-42.0960199974808,38.0299315370551,38.8729945665287));
#30275=CARTESIAN_POINT('Ctrl Pts',(-42.1110196932476,38.0554607687221,38.8862183799112));
#30276=CARTESIAN_POINT('Ctrl Pts',(-42.1260193890143,38.0809900003891,38.8994421932938));
#30277=CARTESIAN_POINT('Ctrl Pts',(-42.1408483908508,38.1067131717948,38.912485335234));
#30278=CARTESIAN_POINT('Ctrl Pts',(-42.1555038965921,38.1326254259851,38.9253453414547));
#30279=CARTESIAN_POINT('Ctrl Pts',(-42.1701594023335,38.1585376801753,38.9382053476754));
#30280=CARTESIAN_POINT('Ctrl Pts',(-42.1846414119102,38.1846390170274,38.9508822181156));
#30281=CARTESIAN_POINT('Ctrl Pts',(-42.1989471885747,38.2109245082375,38.9633735575496));
#30282=CARTESIAN_POINT('Ctrl Pts',(-42.2132529652392,38.2372099994476,38.9758648969837));
#30283=CARTESIAN_POINT('Ctrl Pts',(-42.2273825089236,38.263679644891,38.9881707053525));
#30284=CARTESIAN_POINT('Ctrl Pts',(-42.2413331493284,38.2903284467695,39.0002886573846));
#30285=CARTESIAN_POINT('Ctrl Pts',(-42.2552837897332,38.3169772486478,39.0124066094168));
#30286=CARTESIAN_POINT('Ctrl Pts',(-42.2690555267923,38.3438052068348,39.0243367050547));
#30287=CARTESIAN_POINT('Ctrl Pts',(-42.2826457576608,38.3708072559186,39.0360766898576));
#30288=CARTESIAN_POINT('Ctrl Pts',(-42.2962480667472,38.3978333028752,39.0478271084856));
#30289=CARTESIAN_POINT('Ctrl Pts',(-42.3096685468105,38.425033750182,39.0593870781533));
#30290=CARTESIAN_POINT('Ctrl Pts',(-42.3229046566779,38.452403453028,39.0707544102742));
#30291=CARTESIAN_POINT('Ctrl Pts',(-41.5484677647746,37.2901211708148,38.3975178306748));
#30292=CARTESIAN_POINT('Ctrl Pts',(-41.5673061531269,37.311385584891,38.4148648435003));
#30293=CARTESIAN_POINT('Ctrl Pts',(-41.5860012811259,37.3329053256431,38.4320544470383));
#30294=CARTESIAN_POINT('Ctrl Pts',(-41.6045494205091,37.3546761015114,38.4490832132649));
#30295=CARTESIAN_POINT('Ctrl Pts',(-41.6230975598923,37.3764468773797,38.4661119794914));
#30296=CARTESIAN_POINT('Ctrl Pts',(-41.6414987105613,37.3984686882489,38.4829799083159));
#30297=CARTESIAN_POINT('Ctrl Pts',(-41.6597492028795,37.420737142435,38.4996836358636));
#30298=CARTESIAN_POINT('Ctrl Pts',(-41.6779996951978,37.443005596621,38.5163873634113));
#30299=CARTESIAN_POINT('Ctrl Pts',(-41.6960995290685,37.4655206940058,38.5329268895937));
#30300=CARTESIAN_POINT('Ctrl Pts',(-41.7140450949451,37.488277944532,38.5492989160273));
#30301=CARTESIAN_POINT('Ctrl Pts',(-41.7319906608217,37.5110351950581,38.5656709424609));
#30302=CARTESIAN_POINT('Ctrl Pts',(-41.7497819586091,37.5340345986049,38.581875469059));
#30303=CARTESIAN_POINT('Ctrl Pts',(-41.7674154402901,37.5572715685325,38.5979092642452));
#30304=CARTESIAN_POINT('Ctrl Pts',(-41.7850489219711,37.5805085384601,38.6139430594314));
#30305=CARTESIAN_POINT('Ctrl Pts',(-41.8025245874523,37.6039830746453,38.6298061231207));
#30306=CARTESIAN_POINT('Ctrl Pts',(-41.8198389516615,37.6276904956952,38.6454952918329));
#30307=CARTESIAN_POINT('Ctrl Pts',(-41.8371533158706,37.6513979167452,38.6611844605451));
#30308=CARTESIAN_POINT('Ctrl Pts',(-41.8543063787158,37.6753382225342,38.6766997341969));
#30309=CARTESIAN_POINT('Ctrl Pts',(-41.8712947194597,37.6995066387835,38.6920380186659));
#30310=CARTESIAN_POINT('Ctrl Pts',(-41.8882830602036,37.723675055033,38.7073763031348));
#30311=CARTESIAN_POINT('Ctrl Pts',(-41.9051066787561,37.7480715816146,38.7225375983396));
#30312=CARTESIAN_POINT('Ctrl Pts',(-41.9217622200788,37.7726913532685,38.7375188807495));
#30313=CARTESIAN_POINT('Ctrl Pts',(-41.9384177614015,37.7973111249223,38.7525001631594));
#30314=CARTESIAN_POINT('Ctrl Pts',(-41.9549052254061,37.8221541415177,38.7673014326951));
#30315=CARTESIAN_POINT('Ctrl Pts',(-41.9712213240919,37.8472154487537,38.7819197376237));
#30316=CARTESIAN_POINT('Ctrl Pts',(-41.9875374227776,37.8722767559897,38.7965380425524));
#30317=CARTESIAN_POINT('Ctrl Pts',(-42.003682156058,37.8975563537332,38.8109733827966));
#30318=CARTESIAN_POINT('Ctrl Pts',(-42.0196523042808,37.9230492006185,38.8252228795986));
#30319=CARTESIAN_POINT('Ctrl Pts',(-42.0356224525036,37.9485420475038,38.8394723764007));
#30320=CARTESIAN_POINT('Ctrl Pts',(-42.0514180155842,37.9742481433955,38.8535360296852));
#30321=CARTESIAN_POINT('Ctrl Pts',(-42.0670358435035,38.0001623618738,38.8674110348178));
#30322=CARTESIAN_POINT('Ctrl Pts',(-42.0826536714229,38.0260765803519,38.8812860399505));
#30323=CARTESIAN_POINT('Ctrl Pts',(-42.0980937640983,38.0521989212791,38.8949723968578));
#30324=CARTESIAN_POINT('Ctrl Pts',(-42.1133530424,38.0785241752259,38.9084673761477));
#30325=CARTESIAN_POINT('Ctrl Pts',(-42.1286123207017,38.1048494291727,38.9219623554375));
#30326=CARTESIAN_POINT('Ctrl Pts',(-42.1436907845489,38.1313775959995,38.9352659570384));
#30327=CARTESIAN_POINT('Ctrl Pts',(-42.1585854269294,38.1581033853453,38.9483755278889));
#30328=CARTESIAN_POINT('Ctrl Pts',(-42.17348006931,38.1848291746911,38.9614850987395));
#30329=CARTESIAN_POINT('Ctrl Pts',(-42.188190890145,38.2117525864143,38.9744006387701));
#30330=CARTESIAN_POINT('Ctrl Pts',(-42.2027149557394,38.2388682513324,38.9871195723083));
#30331=CARTESIAN_POINT('Ctrl Pts',(-42.2172390213338,38.2659839162503,38.9998385058467));
#30332=CARTESIAN_POINT('Ctrl Pts',(-42.2315763316105,38.2932918342195,39.0123608328251));
#30333=CARTESIAN_POINT('Ctrl Pts',(-42.2457240273616,38.3207865593774,39.0246840559876));
#30334=CARTESIAN_POINT('Ctrl Pts',(-42.2598717231127,38.3482812845353,39.0370072791501));
#30335=CARTESIAN_POINT('Ctrl Pts',(-42.2738298042631,38.3759628167363,39.0491313984311));
#30336=CARTESIAN_POINT('Ctrl Pts',(-42.2875954872323,38.4038256356102,39.0610539959869));
#30337=CARTESIAN_POINT('Ctrl Pts',(-42.3013734043511,38.4317132173598,39.0729871896636));
#30338=CARTESIAN_POINT('Ctrl Pts',(-42.3149585810787,38.4597824080118,39.0847185031907));
#30339=CARTESIAN_POINT('Ctrl Pts',(-42.3283483033489,38.4880275999658,39.0962455928629));
#30340=CARTESIAN_POINT('Ctrl Pts',(-41.5388663699673,37.2907140657908,38.4072179007401));
#30341=CARTESIAN_POINT('Ctrl Pts',(-41.5581584681248,37.3125288961699,38.4250447925802));
#30342=CARTESIAN_POINT('Ctrl Pts',(-41.5772999160183,37.3346122239288,38.4427061553675));
#30343=CARTESIAN_POINT('Ctrl Pts',(-41.5962867040786,37.3569594237608,38.4601982901835));
#30344=CARTESIAN_POINT('Ctrl Pts',(-41.615273492139,37.3793066235928,38.4776904249995));
#30345=CARTESIAN_POINT('Ctrl Pts',(-41.6341056202551,37.4019176953677,38.495013331742));
#30346=CARTESIAN_POINT('Ctrl Pts',(-41.6527791435672,37.42478790337,38.5121633822974));
#30347=CARTESIAN_POINT('Ctrl Pts',(-41.6714526668793,37.4476581113723,38.5293134328528));
#30348=CARTESIAN_POINT('Ctrl Pts',(-41.6899675852783,37.4707874554685,38.546290627121));
#30349=CARTESIAN_POINT('Ctrl Pts',(-41.708320020263,37.4941710915129,38.5630914093099));
#30350=CARTESIAN_POINT('Ctrl Pts',(-41.7266724552478,37.5175547275574,38.5798921914988));
#30351=CARTESIAN_POINT('Ctrl Pts',(-41.7448624067111,37.5411926554138,38.5965165615103));
#30352=CARTESIAN_POINT('Ctrl Pts',(-41.7628860641319,37.5650799245308,38.6129610373599));
#30353=CARTESIAN_POINT('Ctrl Pts',(-41.7809097215526,37.5889671936478,38.6294055132095));
#30354=CARTESIAN_POINT('Ctrl Pts',(-41.7987670848255,37.6131038038861,38.6456700948011));
#30355=CARTESIAN_POINT('Ctrl Pts',(-41.816454413002,37.6374847003579,38.661751375413));
#30356=CARTESIAN_POINT('Ctrl Pts',(-41.8341417411785,37.6618655968296,38.6778326560249));
#30357=CARTESIAN_POINT('Ctrl Pts',(-41.8516590341555,37.6864907793926,38.6937306355633));
#30358=CARTESIAN_POINT('Ctrl Pts',(-41.8690026221209,37.7113550909348,38.7094419839932));
#30359=CARTESIAN_POINT('Ctrl Pts',(-41.8863462100864,37.736219402477,38.7251533324231));
#30360=CARTESIAN_POINT('Ctrl Pts',(-41.9035160929392,37.7613228428534,38.7406780496528));
#30361=CARTESIAN_POINT('Ctrl Pts',(-41.920508673538,37.786660154883,38.756012883726));
#30362=CARTESIAN_POINT('Ctrl Pts',(-41.9375012541369,37.8119974669126,38.7713477177992));
#30363=CARTESIAN_POINT('Ctrl Pts',(-41.9543165323828,37.8375686504476,38.7864926686264));
#30364=CARTESIAN_POINT('Ctrl Pts',(-41.9709509853088,37.8633683504351,38.801444563689));
#30365=CARTESIAN_POINT('Ctrl Pts',(-41.9875854382349,37.8891680504226,38.8163964587517));
#30366=CARTESIAN_POINT('Ctrl Pts',(-42.0040390657441,37.9151962667122,38.8311552979626));
#30367=CARTESIAN_POINT('Ctrl Pts',(-42.020308420517,37.9414475486165,38.8457179895674));
#30368=CARTESIAN_POINT('Ctrl Pts',(-42.03657777529,37.967698830521,38.8602806811721));
#30369=CARTESIAN_POINT('Ctrl Pts',(-42.0526628572317,37.9941731778871,38.8746472250857));
#30370=CARTESIAN_POINT('Ctrl Pts',(-42.0685602961113,38.0208650466716,38.88881461161));
#30371=CARTESIAN_POINT('Ctrl Pts',(-42.084457734991,38.0475569154561,38.9029819981344));
#30372=CARTESIAN_POINT('Ctrl Pts',(-42.1001675307158,38.0744663055032,38.9169502271869));
#30373=CARTESIAN_POINT('Ctrl Pts',(-42.1156863915524,38.1015875817298,38.9307163723841));
#30374=CARTESIAN_POINT('Ctrl Pts',(-42.1312052523891,38.1287088579564,38.9444825175813));
#30375=CARTESIAN_POINT('Ctrl Pts',(-42.146533178247,38.1560420202043,38.9580465788428));
#30376=CARTESIAN_POINT('Ctrl Pts',(-42.1616669572668,38.1835813447057,38.9714057143231));
#30377=CARTESIAN_POINT('Ctrl Pts',(-42.1768007362866,38.211120669207,38.9847648498035));
#30378=CARTESIAN_POINT('Ctrl Pts',(-42.1917403683798,38.2388661558012,38.9979190594246));
#30379=CARTESIAN_POINT('Ctrl Pts',(-42.2064827229041,38.2668119944271,39.0108655870671));
#30380=CARTESIAN_POINT('Ctrl Pts',(-42.2212250774283,38.2947578330531,39.0238121147095));
#30381=CARTESIAN_POINT('Ctrl Pts',(-42.2357701542975,38.3229040235479,39.0365509602978));
#30382=CARTESIAN_POINT('Ctrl Pts',(-42.2501149053948,38.3512446719854,39.0490794545905));
#30383=CARTESIAN_POINT('Ctrl Pts',(-42.2644596564921,38.3795853204229,39.0616079488833));
#30384=CARTESIAN_POINT('Ctrl Pts',(-42.2786040817338,38.4081204266379,39.0739260918075));
#30385=CARTESIAN_POINT('Ctrl Pts',(-42.2925452168037,38.4368440153019,39.0860313021162));
#30386=CARTESIAN_POINT('Ctrl Pts',(-42.306498741955,38.4655931318444,39.0981472708417));
#30387=CARTESIAN_POINT('Ctrl Pts',(-42.320248615347,38.4945310658416,39.1100499282281));
#30388=CARTESIAN_POINT('Ctrl Pts',(-42.3337919500199,38.5236517469037,39.1217367754516));
#30389=CARTESIAN_POINT('Ctrl Pts',(-41.5292495984737,37.2912890098431,38.4169028479196));
#30390=CARTESIAN_POINT('Ctrl Pts',(-41.5489801744942,37.3136364084946,38.4351945310541));
#30391=CARTESIAN_POINT('Ctrl Pts',(-41.5685526648667,37.3362655562732,38.4533125154055));
#30392=CARTESIAN_POINT('Ctrl Pts',(-41.5879627668261,37.3591714789373,38.4712528185517));
#30393=CARTESIAN_POINT('Ctrl Pts',(-41.6073728687856,37.3820774016012,38.4891931216979));
#30394=CARTESIAN_POINT('Ctrl Pts',(-41.6266205822024,37.405260098996,38.5069557435165));
#30395=CARTESIAN_POINT('Ctrl Pts',(-41.6457016756296,37.4287144753495,38.5245367796226));
#30396=CARTESIAN_POINT('Ctrl Pts',(-41.6647827690567,37.452168851703,38.5421178157288));
#30397=CARTESIAN_POINT('Ctrl Pts',(-41.6836972423668,37.4758949068577,38.5595172660032));
#30398=CARTESIAN_POINT('Ctrl Pts',(-41.7024409372682,37.4998874257178,38.5767313057839));
#30399=CARTESIAN_POINT('Ctrl Pts',(-41.7211846321696,37.5238799445779,38.5939453455648));
#30400=CARTESIAN_POINT('Ctrl Pts',(-41.7397575485418,37.5481389269893,38.6109739747415));
#30401=CARTESIAN_POINT('Ctrl Pts',(-41.758155603082,37.5726590408337,38.6278134500664));
#30402=CARTESIAN_POINT('Ctrl Pts',(-41.7765536576222,37.5971791546782,38.6446529253913));
#30403=CARTESIAN_POINT('Ctrl Pts',(-41.7947768502118,37.621960399797,38.6613032467549));
#30404=CARTESIAN_POINT('Ctrl Pts',(-41.8128211743291,37.6469973293907,38.6777607539682));
#30405=CARTESIAN_POINT('Ctrl Pts',(-41.8308654984464,37.6720342589844,38.6942182611814));
#30406=CARTESIAN_POINT('Ctrl Pts',(-41.8487309539755,37.6973268728927,38.7104829541389));
#30407=CARTESIAN_POINT('Ctrl Pts',(-41.8664136129311,37.7228696120156,38.7265512573074));
#30408=CARTESIAN_POINT('Ctrl Pts',(-41.8840962718867,37.7484123511386,38.742619560476));
#30409=CARTESIAN_POINT('Ctrl Pts',(-41.9015961341555,37.7742052153137,38.7584914737537));
#30410=CARTESIAN_POINT('Ctrl Pts',(-41.9189093520144,37.8002425355872,38.7741635078405));
#30411=CARTESIAN_POINT('Ctrl Pts',(-41.9362225698734,37.8262798558608,38.7898355419273));
#30412=CARTESIAN_POINT('Ctrl Pts',(-41.953349143217,37.8525616320841,38.8053076967389));
#30413=CARTESIAN_POINT('Ctrl Pts',(-41.9702853062599,37.8790820878963,38.8205765707031));
#30414=CARTESIAN_POINT('Ctrl Pts',(-41.9872214693027,37.9056025437085,38.8358454446673));
#30415=CARTESIAN_POINT('Ctrl Pts',(-42.0039672219417,37.9323616789571,38.850911037702));
#30416=CARTESIAN_POINT('Ctrl Pts',(-42.0205188820049,37.9593536124801,38.8657700375203));
#30417=CARTESIAN_POINT('Ctrl Pts',(-42.0370705420681,37.9863455460031,38.8806290373385));
#30418=CARTESIAN_POINT('Ctrl Pts',(-42.053428109449,38.013570277627,38.8952814438449));
#30419=CARTESIAN_POINT('Ctrl Pts',(-42.069587987193,38.0410218239313,38.9097240354583));
#30420=CARTESIAN_POINT('Ctrl Pts',(-42.0857478649369,38.0684733702357,38.9241666270717));
#30421=CARTESIAN_POINT('Ctrl Pts',(-42.1017100529399,38.0961517310441,38.9383994036993));
#30422=CARTESIAN_POINT('Ctrl Pts',(-42.1174710410429,38.1240508233014,38.9524192358795));
#30423=CARTESIAN_POINT('Ctrl Pts',(-42.1332320291459,38.1519499155588,38.9664390680596));
#30424=CARTESIAN_POINT('Ctrl Pts',(-42.1487918172394,38.1800697390476,38.9802459556711));
#30425=CARTESIAN_POINT('Ctrl Pts',(-42.1641469835165,38.2084041138213,38.993836862806));
#30426=CARTESIAN_POINT('Ctrl Pts',(-42.1795021497936,38.2367384885949,39.0074277699409));
#30427=CARTESIAN_POINT('Ctrl Pts',(-42.1946526941551,38.2652874144759,39.0208026965141));
#30428=CARTESIAN_POINT('Ctrl Pts',(-42.2095952845997,38.294044617103,39.0339587013158));
#30429=CARTESIAN_POINT('Ctrl Pts',(-42.2245378750442,38.3228018197301,39.0471147061175));
#30430=CARTESIAN_POINT('Ctrl Pts',(-42.2392725114835,38.351767298959,39.0600517890953));
#30431=CARTESIAN_POINT('Ctrl Pts',(-42.2537959532316,38.3809346890054,39.0727671052191));
#30432=CARTESIAN_POINT('Ctrl Pts',(-42.2683193949798,38.4101020790518,39.085482421343));
#30433=CARTESIAN_POINT('Ctrl Pts',(-42.2826316419432,38.4394713797283,39.097975970531));
#30434=CARTESIAN_POINT('Ctrl Pts',(-42.2967295461582,38.4690361365363,39.110245005117));
#30435=CARTESIAN_POINT('Ctrl Pts',(-42.310839979782,38.4986271688047,39.1225249437173));
#30436=CARTESIAN_POINT('Ctrl Pts',(-42.3247356894058,38.5284140045892,39.1345799683876));
#30437=CARTESIAN_POINT('Ctrl Pts',(-42.3384136130202,38.558390086054,39.1464074229614));
#30438=CARTESIAN_POINT('Ctrl Pts',(-41.5196199854034,37.2918489624882,38.4265751654796));
#30439=CARTESIAN_POINT('Ctrl Pts',(-41.5397763593754,37.3147139246234,38.4453188414494));
#30440=CARTESIAN_POINT('Ctrl Pts',(-41.5597671768411,37.3378739508545,38.4638806099285));
#30441=CARTESIAN_POINT('Ctrl Pts',(-41.5795878307549,37.3613237037659,38.482256193207));
#30442=CARTESIAN_POINT('Ctrl Pts',(-41.5994084846687,37.3847734566774,38.5006317764855));
#30443=CARTESIAN_POINT('Ctrl Pts',(-41.6190589748855,37.4085129360958,38.5188211744265));
#30444=CARTESIAN_POINT('Ctrl Pts',(-41.6385347728,37.4325366710798,38.536820195149));
#30445=CARTESIAN_POINT('Ctrl Pts',(-41.6580105707144,37.4565604060638,38.5548192158715));
#30446=CARTESIAN_POINT('Ctrl Pts',(-41.677311676184,37.4808683964366,38.5726278592417));
#30447=CARTESIAN_POINT('Ctrl Pts',(-41.6964336411126,37.505455040225,38.5902420211136));
#30448=CARTESIAN_POINT('Ctrl Pts',(-41.7155556060412,37.5300416840132,38.6078561829855));
#30449=CARTESIAN_POINT('Ctrl Pts',(-41.7344984302935,37.554906981043,38.6252758632343));
#30450=CARTESIAN_POINT('Ctrl Pts',(-41.7532577483422,37.580045200905,38.6424970473537));
#30451=CARTESIAN_POINT('Ctrl Pts',(-41.7720170663908,37.6051834207671,38.659718231473));
#30452=CARTESIAN_POINT('Ctrl Pts',(-41.7905928781026,37.6305945632822,38.6767409193396));
#30453=CARTESIAN_POINT('Ctrl Pts',(-41.808980902532,37.6562727722492,38.6935611879397));
#30454=CARTESIAN_POINT('Ctrl Pts',(-41.8273689269614,37.6819509812161,38.7103814565398));
#30455=CARTESIAN_POINT('Ctrl Pts',(-41.8455691639783,37.7078962564534,38.7269993057545));
#30456=CARTESIAN_POINT('Ctrl Pts',(-41.8635774191899,37.7341026186593,38.743410905863));
#30457=CARTESIAN_POINT('Ctrl Pts',(-41.8815856744014,37.7603089808652,38.7598225059716));
#30458=CARTESIAN_POINT('Ctrl Pts',(-41.8994019476804,37.7867764298557,38.7760278568591));
#30459=CARTESIAN_POINT('Ctrl Pts',(-41.9170221331224,37.8134988659925,38.7920232238713));
#30460=CARTESIAN_POINT('Ctrl Pts',(-41.9346423185645,37.8402213021293,38.8080185908835));
#30461=CARTESIAN_POINT('Ctrl Pts',(-41.9520664160503,37.8671987252411,38.8238039739227));
#30462=CARTESIAN_POINT('Ctrl Pts',(-41.9692904100445,37.8944249181274,38.8393757350887));
#30463=CARTESIAN_POINT('Ctrl Pts',(-41.9865144040386,37.9216511110137,38.8549474962546));
#30464=CARTESIAN_POINT('Ctrl Pts',(-42.0035382944246,37.9491260734988,38.8703056354524));
#30465=CARTESIAN_POINT('Ctrl Pts',(-42.0203581579091,37.976843473755,38.8854466132742));
#30466=CARTESIAN_POINT('Ctrl Pts',(-42.0371780213936,38.0045608740113,38.900587591096));
#30467=CARTESIAN_POINT('Ctrl Pts',(-42.0537938578574,38.0325207118424,38.9155114074348));
#30468=CARTESIAN_POINT('Ctrl Pts',(-42.0702018380465,38.0607165436773,38.9302146229761));
#30469=CARTESIAN_POINT('Ctrl Pts',(-42.0866098182356,38.0889123755123,38.9449178385174));
#30470=CARTESIAN_POINT('Ctrl Pts',(-42.1028099420337,38.1173442011513,38.9594004531572));
#30471=CARTESIAN_POINT('Ctrl Pts',(-42.1187984759912,38.1460054682499,38.9736591292596));
#30472=CARTESIAN_POINT('Ctrl Pts',(-42.1347870099487,38.1746667353486,38.987917805362));
#30473=CARTESIAN_POINT('Ctrl Pts',(-42.150563953945,38.2035574436675,39.0019525427967));
#30474=CARTESIAN_POINT('Ctrl Pts',(-42.1661256720702,38.2326709351807,39.015760107203));
#30475=CARTESIAN_POINT('Ctrl Pts',(-42.1816873901954,38.2617844266939,39.0295676716092));
#30476=CARTESIAN_POINT('Ctrl Pts',(-42.197033882339,38.2911207011994,39.0431480628913));
#30477=CARTESIAN_POINT('Ctrl Pts',(-42.2121616117635,38.3206729978371,39.0564981512768));
#30478=CARTESIAN_POINT('Ctrl Pts',(-42.227289341188,38.3502252944748,39.0698482396623));
#30479=CARTESIAN_POINT('Ctrl Pts',(-42.2421983077933,38.379993613074,39.082968025087));
#30480=CARTESIAN_POINT('Ctrl Pts',(-42.2568850756873,38.4099710932844,39.0958544839902));
#30481=CARTESIAN_POINT('Ctrl Pts',(-42.2715718435813,38.4399485734949,39.1087409428933));
#30482=CARTESIAN_POINT('Ctrl Pts',(-42.2860364126601,38.4701352151043,39.1213940751837));
#30483=CARTESIAN_POINT('Ctrl Pts',(-42.3002754494465,38.5005240613567,39.1338109648444));
#30484=CARTESIAN_POINT('Ctrl Pts',(-42.3145271410722,38.5309399154729,39.1462388899246));
#30485=CARTESIAN_POINT('Ctrl Pts',(-42.3285528992461,38.561558333592,39.1584301521826));
#30486=CARTESIAN_POINT('Ctrl Pts',(-42.3423494858242,38.5923722469452,39.1703819369987));
#30487=CARTESIAN_POINT('Ctrl Pts',(-41.5003607592628,37.2929688677784,38.4459198005997));
#30488=CARTESIAN_POINT('Ctrl Pts',(-41.5213687291377,37.3168689568809,38.4655674622402));
#30489=CARTESIAN_POINT('Ctrl Pts',(-41.5421962007899,37.3410907400172,38.4850167989745));
#30490=CARTESIAN_POINT('Ctrl Pts',(-41.5628379586124,37.3656281534234,38.5042629425176));
#30491=CARTESIAN_POINT('Ctrl Pts',(-41.5834797164349,37.3901655668296,38.5235090860608));
#30492=CARTESIAN_POINT('Ctrl Pts',(-41.6039357602518,37.4150186102955,38.5425520362467));
#30493=CARTESIAN_POINT('Ctrl Pts',(-41.6242009671407,37.4401810625406,38.5613870262018));
#30494=CARTESIAN_POINT('Ctrl Pts',(-41.6444661740297,37.4653435147855,38.5802220161569));
#30495=CARTESIAN_POINT('Ctrl Pts',(-41.6645405438182,37.4908153755945,38.5988490457189));
#30496=CARTESIAN_POINT('Ctrl Pts',(-41.6844190488013,37.5165902692392,38.6172634517729));
#30497=CARTESIAN_POINT('Ctrl Pts',(-41.7042975537844,37.542365162884,38.6356778578269));
#30498=CARTESIAN_POINT('Ctrl Pts',(-41.7239801937969,37.5684430891506,38.65387964022));
#30499=CARTESIAN_POINT('Ctrl Pts',(-41.7434620388624,37.5948175210478,38.6718642419281));
#30500=CARTESIAN_POINT('Ctrl Pts',(-41.7629438839279,37.6211919529449,38.6898488436363));
#30501=CARTESIAN_POINT('Ctrl Pts',(-41.7822249338842,37.6478628902529,38.707616264509));
#30502=CARTESIAN_POINT('Ctrl Pts',(-41.8013003589378,37.6748236579662,38.7251620558827));
#30503=CARTESIAN_POINT('Ctrl Pts',(-41.8203757839915,37.7017844256796,38.7427078472564));
#30504=CARTESIAN_POINT('Ctrl Pts',(-41.839245583984,37.7290350235749,38.7600320089856));
#30505=CARTESIAN_POINT('Ctrl Pts',(-41.8579050317074,37.7565686319467,38.7771302029742));
#30506=CARTESIAN_POINT('Ctrl Pts',(-41.8765644794308,37.7841022403185,38.7942283969628));
#30507=CARTESIAN_POINT('Ctrl Pts',(-41.8950135747302,37.8119188589395,38.8111006230699));
#30508=CARTESIAN_POINT('Ctrl Pts',(-41.9132476953384,37.8400115268029,38.8277426559328));
#30509=CARTESIAN_POINT('Ctrl Pts',(-41.9314818159467,37.8681041946664,38.8443846887957));
#30510=CARTESIAN_POINT('Ctrl Pts',(-41.9495009617168,37.896472911555,38.8607965282903));
#30511=CARTESIAN_POINT('Ctrl Pts',(-41.9673006176136,37.9251105785895,38.8769740638598));
#30512=CARTESIAN_POINT('Ctrl Pts',(-41.9851002735103,37.953748245624,38.8931515994293));
#30513=CARTESIAN_POINT('Ctrl Pts',(-42.0026804393904,37.9826548625821,38.909094830953));
#30514=CARTESIAN_POINT('Ctrl Pts',(-42.0200367097175,38.0118231963049,38.924799764782));
#30515=CARTESIAN_POINT('Ctrl Pts',(-42.0373929800445,38.0409915300278,38.9405046986109));
#30516=CARTESIAN_POINT('Ctrl Pts',(-42.0545253546742,38.0704215802733,38.9559713346146));
#30517=CARTESIAN_POINT('Ctrl Pts',(-42.0714295397536,38.1001059831694,38.9711957980117));
#30518=CARTESIAN_POINT('Ctrl Pts',(-42.0883337248329,38.1297903860654,38.9864202614089));
#30519=CARTESIAN_POINT('Ctrl Pts',(-42.1050097202214,38.1597291413657,39.0014025520731));
#30520=CARTESIAN_POINT('Ctrl Pts',(-42.1214533458878,38.1899147581469,39.01613891602));
#30521=CARTESIAN_POINT('Ctrl Pts',(-42.1378969715542,38.2201003749281,39.0308752799669));
#30522=CARTESIAN_POINT('Ctrl Pts',(-42.1541082273559,38.2505328529074,39.0453657170479));
#30523=CARTESIAN_POINT('Ctrl Pts',(-42.1700830491774,38.2812045778996,39.0596065959968));
#30524=CARTESIAN_POINT('Ctrl Pts',(-42.1860578709989,38.3118763028919,39.0738474749456));
#30525=CARTESIAN_POINT('Ctrl Pts',(-42.2017962587068,38.3427872746465,39.0878387956457));
#30526=CARTESIAN_POINT('Ctrl Pts',(-42.2172942660912,38.3739297593054,39.1015770511987));
#30527=CARTESIAN_POINT('Ctrl Pts',(-42.2327922734756,38.4050722439644,39.1153153067518));
#30528=CARTESIAN_POINT('Ctrl Pts',(-42.2480499004129,38.4364462413039,39.1288004970705));
#30529=CARTESIAN_POINT('Ctrl Pts',(-42.2630633205988,38.4680439018423,39.1420292415324));
#30530=CARTESIAN_POINT('Ctrl Pts',(-42.2780767407846,38.4996415623808,39.1552579859942));
#30531=CARTESIAN_POINT('Ctrl Pts',(-42.2928459540939,38.5314628858563,39.168230284489));
#30532=CARTESIAN_POINT('Ctrl Pts',(-42.3073672560232,38.5634999109975,39.1809428842993));
#30533=CARTESIAN_POINT('Ctrl Pts',(-42.3219014636528,38.5955654088094,39.1936667823392));
#30534=CARTESIAN_POINT('Ctrl Pts',(-42.3361873189266,38.6278469915978,39.2061305197727));
#30535=CARTESIAN_POINT('Ctrl Pts',(-42.3502212314322,38.6603365687275,39.2183309650732));
#30536=CARTESIAN_POINT('Ctrl Pts',(-41.4810505382599,37.2940292410687,38.4652142825554));
#30537=CARTESIAN_POINT('Ctrl Pts',(-41.5028597677074,37.318904858524,38.4857150693105));
#30538=CARTESIAN_POINT('Ctrl Pts',(-41.5244734170253,37.3441290497964,38.506000959708));
#30539=CARTESIAN_POINT('Ctrl Pts',(-41.5458856178102,37.3696949679436,38.5260664478572));
#30540=CARTESIAN_POINT('Ctrl Pts',(-41.567297818595,37.395260886091,38.5461319360062));
#30541=CARTESIAN_POINT('Ctrl Pts',(-41.5885085706376,37.4211685308637,38.565977021711));
#30542=CARTESIAN_POINT('Ctrl Pts',(-41.6095121145511,37.4474108703597,38.5855963183546));
#30543=CARTESIAN_POINT('Ctrl Pts',(-41.6305156584647,37.4736532098558,38.6052156149982));
#30544=CARTESIAN_POINT('Ctrl Pts',(-41.651311994044,37.5002302438191,38.6246091223891));
#30545=CARTESIAN_POINT('Ctrl Pts',(-41.6718954740267,37.5271347591798,38.64377157609));
#30546=CARTESIAN_POINT('Ctrl Pts',(-41.6924789540094,37.5540392745403,38.6629340297909));
#30547=CARTESIAN_POINT('Ctrl Pts',(-41.7128495781944,37.5812712710359,38.6818654296146));
#30548=CARTESIAN_POINT('Ctrl Pts',(-41.7330018144911,37.6088233583184,38.7005606361427));
#30549=CARTESIAN_POINT('Ctrl Pts',(-41.7531540507878,37.6363754456009,38.7192558426709));
#30550=CARTESIAN_POINT('Ctrl Pts',(-41.7730878989981,37.6642476233992,38.7377148557188));
#30551=CARTESIAN_POINT('Ctrl Pts',(-41.7927979451909,37.6924323280774,38.7559326636636));
#30552=CARTESIAN_POINT('Ctrl Pts',(-41.8125079913837,37.7206170327555,38.7741504716083));
#30553=CARTESIAN_POINT('Ctrl Pts',(-41.8319942353652,37.7491142640362,38.7921270742699));
#30554=CARTESIAN_POINT('Ctrl Pts',(-41.8512513842813,37.7779162890641,38.8098575905164));
#30555=CARTESIAN_POINT('Ctrl Pts',(-41.8705085331973,37.8067183140921,38.8275881067629));
#30556=CARTESIAN_POINT('Ctrl Pts',(-41.8895365868606,37.8358251325889,38.8450725364234));
#30557=CARTESIAN_POINT('Ctrl Pts',(-41.9083303763512,37.8652288466486,38.8623061314902));
#30558=CARTESIAN_POINT('Ctrl Pts',(-41.9271241658417,37.8946325607082,38.879539726557));
#30559=CARTESIAN_POINT('Ctrl Pts',(-41.9456836909767,37.9243331700466,38.8965224868639));
#30560=CARTESIAN_POINT('Ctrl Pts',(-41.9640039095648,37.9543226159753,38.9132498000987));
#30561=CARTESIAN_POINT('Ctrl Pts',(-41.9823241281528,37.984312061904,38.9299771133336));
#30562=CARTESIAN_POINT('Ctrl Pts',(-42.0004050400183,38.0145903441468,38.9464489793472));
#30563=CARTESIAN_POINT('Ctrl Pts',(-42.0182417324114,38.0451492475406,38.9626609239792));
#30564=CARTESIAN_POINT('Ctrl Pts',(-42.0360784248044,38.0757081509344,38.9788728686112));
#30565=CARTESIAN_POINT('Ctrl Pts',(-42.0536708975543,38.1065476751967,38.9948248917171));
#30566=CARTESIAN_POINT('Ctrl Pts',(-42.0710143700199,38.1376594531819,39.01051265976));
#30567=CARTESIAN_POINT('Ctrl Pts',(-42.0883578424855,38.168771231167,39.026200427803));
#30568=CARTESIAN_POINT('Ctrl Pts',(-42.1054523144972,38.2001552625715,39.0416239406297));
#30569=CARTESIAN_POINT('Ctrl Pts',(-42.1222931400975,38.2318030327456,39.0567790076379));
#30570=CARTESIAN_POINT('Ctrl Pts',(-42.1391339656979,38.2634508029195,39.0719340746463));
#30571=CARTESIAN_POINT('Ctrl Pts',(-42.1557211447188,38.2953623115353,39.0868206956727));
#30572=CARTESIAN_POINT('Ctrl Pts',(-42.1720501684025,38.3275289010664,39.1014348253432));
#30573=CARTESIAN_POINT('Ctrl Pts',(-42.1883791920861,38.3596954905976,39.1160489550136));
#30574=CARTESIAN_POINT('Ctrl Pts',(-42.2044500602723,38.3921171607325,39.1303905931859));
#30575=CARTESIAN_POINT('Ctrl Pts',(-42.2202584038194,38.4247851156183,39.1444558418065));
#30576=CARTESIAN_POINT('Ctrl Pts',(-42.2360667473665,38.4574530705043,39.158521090427));
#30577=CARTESIAN_POINT('Ctrl Pts',(-42.2516125661229,38.4903673098427,39.1723099493739));
#30578=CARTESIAN_POINT('Ctrl Pts',(-42.2668916329426,38.5235189043152,39.185818670113));
#30579=CARTESIAN_POINT('Ctrl Pts',(-42.2821706997623,38.5566704987877,39.1993273908521));
#30580=CARTESIAN_POINT('Ctrl Pts',(-42.2971830144957,38.5900594480711,39.2125559732512));
#30581=CARTESIAN_POINT('Ctrl Pts',(-42.3119244942714,38.623676694153,39.2255008202899));
#30582=CARTESIAN_POINT('Ctrl Pts',(-42.326679075429,38.6573238173155,39.2384571719662));
#30583=CARTESIAN_POINT('Ctrl Pts',(-42.3411623398628,38.6911996428923,39.2511292835741));
#30584=CARTESIAN_POINT('Ctrl Pts',(-42.3553703406829,38.7252949646174,39.2635137024035));
#30585=CARTESIAN_POINT('Ctrl Pts',(-41.4617031412175,37.2950462146149,38.4844722020825));
#30586=CARTESIAN_POINT('Ctrl Pts',(-41.4842771920991,37.3208536029999,38.505788299774));
#30587=CARTESIAN_POINT('Ctrl Pts',(-41.5066404845182,37.3470366168299,38.5268728237077));
#30588=CARTESIAN_POINT('Ctrl Pts',(-41.5287864577224,37.3735875747549,38.5477195882852));
#30589=CARTESIAN_POINT('Ctrl Pts',(-41.5509324309266,37.4001385326801,38.5685663528626));
#30590=CARTESIAN_POINT('Ctrl Pts',(-41.5728610846616,37.4270574343957,38.5891753578446));
#30591=CARTESIAN_POINT('Ctrl Pts',(-41.5945659856856,37.4543363826632,38.6095405571367));
#30592=CARTESIAN_POINT('Ctrl Pts',(-41.6162708867097,37.4816153309308,38.6299057564287));
#30593=CARTESIAN_POINT('Ctrl Pts',(-41.6377520347735,37.5092543254373,38.650027149797));
#30594=CARTESIAN_POINT('Ctrl Pts',(-41.6590031279208,37.5372452576896,38.6698988341983));
#30595=CARTESIAN_POINT('Ctrl Pts',(-41.680254221068,37.5652361899419,38.6897705185996));
#30596=CARTESIAN_POINT('Ctrl Pts',(-41.7012752590547,37.5935790596188,38.7093924938059));
#30597=CARTESIAN_POINT('Ctrl Pts',(-41.7220600749075,37.6222655517302,38.7287590032889));
#30598=CARTESIAN_POINT('Ctrl Pts',(-41.7428448907603,37.6509520438417,38.7481255127719));
#30599=CARTESIAN_POINT('Ctrl Pts',(-41.7633934842396,37.6799821580562,38.7672365563075));
#30600=CARTESIAN_POINT('Ctrl Pts',(-41.783699826976,37.7093473777702,38.7860865272641));
#30601=CARTESIAN_POINT('Ctrl Pts',(-41.8040061697124,37.7387125974843,38.8049364982207));
#30602=CARTESIAN_POINT('Ctrl Pts',(-41.8240702614719,37.7684129223586,38.8235253963801));
#30603=CARTESIAN_POINT('Ctrl Pts',(-41.8438862160216,37.7984396391645,38.8418477682894));
#30604=CARTESIAN_POINT('Ctrl Pts',(-41.8637021705714,37.8284663559705,38.8601701401986));
#30605=CARTESIAN_POINT('Ctrl Pts',(-41.8832699876851,37.8588194643661,38.8782259856497));
#30606=CARTESIAN_POINT('Ctrl Pts',(-41.9025839267211,37.8894900596093,38.896010007568));
#30607=CARTESIAN_POINT('Ctrl Pts',(-41.921897865757,37.9201606548526,38.9137940294863));
#30608=CARTESIAN_POINT('Ctrl Pts',(-41.9409579264945,37.9511487365941,38.9313062276698));
#30609=CARTESIAN_POINT('Ctrl Pts',(-41.959758517255,37.9824452138141,38.9485414645386));
#30610=CARTESIAN_POINT('Ctrl Pts',(-41.9785591080156,38.013741691034,38.9657767014075));
#30611=CARTESIAN_POINT('Ctrl Pts',(-41.9971002285865,38.045346563388,38.9827349767773));
#30612=CARTESIAN_POINT('Ctrl Pts',(-42.0153764395253,38.0772505588784,38.9994113155473));
#30613=CARTESIAN_POINT('Ctrl Pts',(-42.0336526504642,38.1091545543687,39.0160876543173));
#30614=CARTESIAN_POINT('Ctrl Pts',(-42.0516639515643,38.1413576726435,39.0324820563089));
#30615=CARTESIAN_POINT('Ctrl Pts',(-42.0694050588234,38.1738504662258,39.048589711872));
#30616=CARTESIAN_POINT('Ctrl Pts',(-42.0871461660825,38.2063432598082,39.064697367435));
#30617=CARTESIAN_POINT('Ctrl Pts',(-42.104617079297,38.239125728325,39.0805182763847));
#30618=CARTESIAN_POINT('Ctrl Pts',(-42.1218126729988,38.2721882543348,39.0960477973172));
#30619=CARTESIAN_POINT('Ctrl Pts',(-42.1390082667007,38.3052507803445,39.1115773182498));
#30620=CARTESIAN_POINT('Ctrl Pts',(-42.1559285406899,38.33859336345,39.1268154509731));
#30621=CARTESIAN_POINT('Ctrl Pts',(-42.1725685310459,38.3722062219227,39.141757725081));
#30622=CARTESIAN_POINT('Ctrl Pts',(-42.189208521402,38.4058190803953,39.1566999991889));
#30623=CARTESIAN_POINT('Ctrl Pts',(-42.2055682279336,38.4397022138511,39.1713464145106));
#30624=CARTESIAN_POINT('Ctrl Pts',(-42.2216428511641,38.4738456819071,39.1856926741767));
#30625=CARTESIAN_POINT('Ctrl Pts',(-42.2377174743946,38.5079891499631,39.2000389338428));
#30626=CARTESIAN_POINT('Ctrl Pts',(-42.2535070141421,38.5423929522459,39.2140850377029));
#30627=CARTESIAN_POINT('Ctrl Pts',(-42.2690068382058,38.5770469956607,39.2278268650306));
#30628=CARTESIAN_POINT('Ctrl Pts',(-42.2845066622695,38.6117010390754,39.2415686923582));
#30629=CARTESIAN_POINT('Ctrl Pts',(-42.2997167704714,38.6466053232244,39.2550062429957));
#30630=CARTESIAN_POINT('Ctrl Pts',(-42.3146327005994,38.6817496081857,39.2681355747486));
#30631=CARTESIAN_POINT('Ctrl Pts',(-42.3295618871507,38.7169251273719,39.2812765750988));
#30632=CARTESIAN_POINT('Ctrl Pts',(-42.3441963723255,38.7523410737258,39.2941088082959));
#30633=CARTESIAN_POINT('Ctrl Pts',(-42.3585318550746,38.7879870388601,39.3066285029924));
#30634=CARTESIAN_POINT('Ctrl Pts',(-41.4423557441752,37.2960631881612,38.5037301216096));
#30635=CARTESIAN_POINT('Ctrl Pts',(-41.4656946164909,37.3228023474757,38.5258615302376));
#30636=CARTESIAN_POINT('Ctrl Pts',(-41.4888075520112,37.3499441838633,38.5477446877073));
#30637=CARTESIAN_POINT('Ctrl Pts',(-41.5116872976347,37.3774801815662,38.5693727287131));
#30638=CARTESIAN_POINT('Ctrl Pts',(-41.5345670432582,37.4050161792692,38.591000769719));
#30639=CARTESIAN_POINT('Ctrl Pts',(-41.5572135986857,37.4329463379276,38.6123736939783));
#30640=CARTESIAN_POINT('Ctrl Pts',(-41.5796198568202,37.4612618949667,38.6334847959188));
#30641=CARTESIAN_POINT('Ctrl Pts',(-41.6020261149547,37.4895774520057,38.6545958978593));
#30642=CARTESIAN_POINT('Ctrl Pts',(-41.6241920755031,37.5182784070554,38.6754451772049));
#30643=CARTESIAN_POINT('Ctrl Pts',(-41.6461107818148,37.5473557561995,38.6960260923066));
#30644=CARTESIAN_POINT('Ctrl Pts',(-41.6680294881265,37.5764331053434,38.7166070074083));
#30645=CARTESIAN_POINT('Ctrl Pts',(-41.6897009399149,37.6058868482017,38.7369195579971));
#30646=CARTESIAN_POINT('Ctrl Pts',(-41.7111183353238,37.6357077451421,38.756957370435));
#30647=CARTESIAN_POINT('Ctrl Pts',(-41.7325357307328,37.6655286420825,38.776995182873));
#30648=CARTESIAN_POINT('Ctrl Pts',(-41.7536990694811,37.6957166927132,38.7967582568962));
#30649=CARTESIAN_POINT('Ctrl Pts',(-41.7746017087611,37.7262624274631,38.8162403908647));
#30650=CARTESIAN_POINT('Ctrl Pts',(-41.7955043480412,37.756808162213,38.8357225248331));
#30651=CARTESIAN_POINT('Ctrl Pts',(-41.8161462875785,37.7877115806809,38.8549237184903));
#30652=CARTESIAN_POINT('Ctrl Pts',(-41.836521047762,37.818962989265,38.8738379460623));
#30653=CARTESIAN_POINT('Ctrl Pts',(-41.8568958079455,37.850214397849,38.8927521736344));
#30654=CARTESIAN_POINT('Ctrl Pts',(-41.8770033885096,37.8818137961431,38.9113794348761));
#30655=CARTESIAN_POINT('Ctrl Pts',(-41.896837477091,37.91375127257,38.9297138836458));
#30656=CARTESIAN_POINT('Ctrl Pts',(-41.9166715656723,37.9456887489969,38.9480483324156));
#30657=CARTESIAN_POINT('Ctrl Pts',(-41.9362321620123,37.9779643031416,38.9660899684756));
#30658=CARTESIAN_POINT('Ctrl Pts',(-41.9555131249453,38.0105678116528,38.9838331289786));
#30659=CARTESIAN_POINT('Ctrl Pts',(-41.9747940878784,38.0431713201639,39.0015762894816));
#30660=CARTESIAN_POINT('Ctrl Pts',(-41.9937954171547,38.0761027826293,39.0190209742075));
#30661=CARTESIAN_POINT('Ctrl Pts',(-42.0125111466393,38.1093518702162,39.0361617071154));
#30662=CARTESIAN_POINT('Ctrl Pts',(-42.0312268761239,38.1426009578031,39.0533024400233));
#30663=CARTESIAN_POINT('Ctrl Pts',(-42.0496570055743,38.1761676700903,39.0701392209007));
#30664=CARTESIAN_POINT('Ctrl Pts',(-42.0677957476269,38.2100414792698,39.0866667639839));
#30665=CARTESIAN_POINT('Ctrl Pts',(-42.0859344896795,38.2439152884493,39.103194307067));
#30666=CARTESIAN_POINT('Ctrl Pts',(-42.1037818440966,38.2780961940786,39.1194126121397));
#30667=CARTESIAN_POINT('Ctrl Pts',(-42.1213322059,38.3125734759241,39.1353165869965));
#30668=CARTESIAN_POINT('Ctrl Pts',(-42.1388825677034,38.3470507577696,39.1512205618533));
#30669=CARTESIAN_POINT('Ctrl Pts',(-42.156135936661,38.3818244153648,39.1668102062735));
#30670=CARTESIAN_POINT('Ctrl Pts',(-42.1730868936895,38.4168835427789,39.1820806248188));
#30671=CARTESIAN_POINT('Ctrl Pts',(-42.1900378507179,38.451942670193,39.1973510433641));
#30672=CARTESIAN_POINT('Ctrl Pts',(-42.2066863955949,38.4872872669698,39.2123022358353));
#30673=CARTESIAN_POINT('Ctrl Pts',(-42.2230272985088,38.5229062481958,39.226929506547));
#30674=CARTESIAN_POINT('Ctrl Pts',(-42.2393682014227,38.5585252294219,39.2415567772586));
#30675=CARTESIAN_POINT('Ctrl Pts',(-42.2554014621614,38.594418594649,39.255860126032));
#30676=CARTESIAN_POINT('Ctrl Pts',(-42.2711220434691,38.6305750870061,39.2698350599482));
#30677=CARTESIAN_POINT('Ctrl Pts',(-42.2868426247767,38.6667315793631,39.2838099938643));
#30678=CARTESIAN_POINT('Ctrl Pts',(-42.3022505264471,38.7031511983778,39.2974565127401));
#30679=CARTESIAN_POINT('Ctrl Pts',(-42.3173409069274,38.7398225222183,39.3107703292074));
#30680=CARTESIAN_POINT('Ctrl Pts',(-42.3324446988724,38.7765264374284,39.3240959782312));
#30681=CARTESIAN_POINT('Ctrl Pts',(-42.3472304047882,38.8134825045594,39.3370883330176));
#30682=CARTESIAN_POINT('Ctrl Pts',(-42.3616933694662,38.8506791131029,39.3497433035812));
#30683=CARTESIAN_POINT('Ctrl Pts',(-41.4229709680434,37.2970365249204,38.5229512790095));
#30684=CARTESIAN_POINT('Ctrl Pts',(-41.4470380178747,37.3246634845394,38.5458600258535));
#30685=CARTESIAN_POINT('Ctrl Pts',(-41.4708638548674,37.3527203469931,38.5685037367787));
#30686=CARTESIAN_POINT('Ctrl Pts',(-41.4944404939676,37.3811977108283,38.5908748246234));
#30687=CARTESIAN_POINT('Ctrl Pts',(-41.5180171330677,37.4096750746636,38.6132459124681));
#30688=CARTESIAN_POINT('Ctrl Pts',(-41.5413445739236,37.438572939456,38.6353443768986));
#30689=CARTESIAN_POINT('Ctrl Pts',(-41.564414998132,37.4678816225096,38.6571628130699));
#30690=CARTESIAN_POINT('Ctrl Pts',(-41.5874854223405,37.4971903055632,38.6789812492413));
#30691=CARTESIAN_POINT('Ctrl Pts',(-41.6102988295575,37.5269098064413,38.7005196568283));
#30692=CARTESIAN_POINT('Ctrl Pts',(-41.6328475732494,37.5570301676657,38.7217708182439));
#30693=CARTESIAN_POINT('Ctrl Pts',(-41.6553963169414,37.5871505288901,38.7430219796596));
#30694=CARTESIAN_POINT('Ctrl Pts',(-41.677680396772,37.617671750012,38.7639858945871));
#30695=CARTESIAN_POINT('Ctrl Pts',(-41.6996923431815,37.648583605415,38.7846555375145));
#30696=CARTESIAN_POINT('Ctrl Pts',(-41.7217042895911,37.6794954608179,38.8053251804419));
#30697=CARTESIAN_POINT('Ctrl Pts',(-41.743444102251,37.7107979500415,38.8257005510608));
#30698=CARTESIAN_POINT('Ctrl Pts',(-41.7649044935619,37.7424805861532,38.8457748206228));
#30699=CARTESIAN_POINT('Ctrl Pts',(-41.7863648848728,37.7741632222648,38.8658490901848));
#30700=CARTESIAN_POINT('Ctrl Pts',(-41.8075458545143,37.8062260047926,38.8856222583904));
#30701=CARTESIAN_POINT('Ctrl Pts',(-41.828440301712,37.8386581924846,38.9050876978125));
#30702=CARTESIAN_POINT('Ctrl Pts',(-41.8493347489098,37.8710903801766,38.9245531372346));
#30703=CARTESIAN_POINT('Ctrl Pts',(-41.869942673352,37.9038919725495,38.9437108475828));
#30704=CARTESIAN_POINT('Ctrl Pts',(-41.8902571658307,37.9370519811976,38.962554407175));
#30705=CARTESIAN_POINT('Ctrl Pts',(-41.9105716583094,37.9702119898458,38.9813979667672));
#30706=CARTESIAN_POINT('Ctrl Pts',(-41.9305927185212,38.0037304142752,38.9999273753223));
#30707=CARTESIAN_POINT('Ctrl Pts',(-41.9503136334377,38.0375960262564,39.0181364211902));
#30708=CARTESIAN_POINT('Ctrl Pts',(-41.9700345483543,38.0714616382376,39.0363454670581));
#30709=CARTESIAN_POINT('Ctrl Pts',(-41.9894553176812,38.1056744372663,39.0542341499672));
#30710=CARTESIAN_POINT('Ctrl Pts',(-42.0085694290524,38.1402229627798,39.0717964724463));
#30711=CARTESIAN_POINT('Ctrl Pts',(-42.0276835404236,38.1747714882931,39.0893587949255));
#30712=CARTESIAN_POINT('Ctrl Pts',(-42.0464909935538,38.2096557397765,39.1065947567127));
#30713=CARTESIAN_POINT('Ctrl Pts',(-42.0649854810888,38.2448640319788,39.1234985785208));
#30714=CARTESIAN_POINT('Ctrl Pts',(-42.0834799686239,38.2800723241811,39.1404024003288));
#30715=CARTESIAN_POINT('Ctrl Pts',(-42.1016614902876,38.3156046565778,39.1569740819053));
#30716=CARTESIAN_POINT('Ctrl Pts',(-42.1195239479505,38.3514491270237,39.1732080660062));
#30717=CARTESIAN_POINT('Ctrl Pts',(-42.1373864056134,38.3872935974697,39.189442050107));
#30718=CARTESIAN_POINT('Ctrl Pts',(-42.1549297990088,38.4234502054309,39.2053383364899));
#30719=CARTESIAN_POINT('Ctrl Pts',(-42.1721482433057,38.4599068398074,39.2208915936653));
#30720=CARTESIAN_POINT('Ctrl Pts',(-42.1893666876025,38.496363474184,39.2364448508407));
#30721=CARTESIAN_POINT('Ctrl Pts',(-42.2062601825436,38.5331201344327,39.2516550785763));
#30722=CARTESIAN_POINT('Ctrl Pts',(-42.222823060528,38.5701645085773,39.266517174699));
#30723=CARTESIAN_POINT('Ctrl Pts',(-42.2393859385125,38.6072088827218,39.2813792708218));
#30724=CARTESIAN_POINT('Ctrl Pts',(-42.2556181992928,38.6445409702104,39.2958932351096));
#30725=CARTESIAN_POINT('Ctrl Pts',(-42.2715143962856,38.6821482664024,39.3100541981141));
#30726=CARTESIAN_POINT('Ctrl Pts',(-42.2874105932784,38.7197555625943,39.3242151611187));
#30727=CARTESIAN_POINT('Ctrl Pts',(-42.3029707262459,38.7576380669294,39.3380231226285));
#30728=CARTESIAN_POINT('Ctrl Pts',(-42.3181895732623,38.7957830904435,39.3514734491742));
#30729=CARTESIAN_POINT('Ctrl Pts',(-42.3334219459173,38.833962015067,39.3649357295989));
#30730=CARTESIAN_POINT('Ctrl Pts',(-42.3483124254927,38.8724039251315,39.3780397388846));
#30731=CARTESIAN_POINT('Ctrl Pts',(-42.3628560048845,38.9110959214823,39.3907810709114));
#30732=CARTESIAN_POINT('Ctrl Pts',(-41.4035576403252,37.2979765302231,38.5421443560826));
#30733=CARTESIAN_POINT('Ctrl Pts',(-41.428325003475,37.3264575328628,38.565801044497));
#30734=CARTESIAN_POINT('Ctrl Pts',(-41.4528358013829,37.3553958001794,38.5891758283308));
#30735=CARTESIAN_POINT('Ctrl Pts',(-41.4770812806816,37.3847809976551,38.6122603599134));
#30736=CARTESIAN_POINT('Ctrl Pts',(-41.5013267599803,37.4141661951307,38.6353448914959));
#30737=CARTESIAN_POINT('Ctrl Pts',(-41.5253069202575,37.4439983222656,38.6581391704346));
#30738=CARTESIAN_POINT('Ctrl Pts',(-41.5490131976487,37.4742667253239,38.6806350563704));
#30739=CARTESIAN_POINT('Ctrl Pts',(-41.5727194750401,37.5045351283822,38.7031309423063));
#30740=CARTESIAN_POINT('Ctrl Pts',(-41.5961518691422,37.5352398068492,38.7253284348567));
#30741=CARTESIAN_POINT('Ctrl Pts',(-41.6193020117108,37.566369795381,38.7472196067887));
#30742=CARTESIAN_POINT('Ctrl Pts',(-41.6424521542793,37.5974997839129,38.7691107787207));
#30743=CARTESIAN_POINT('Ctrl Pts',(-41.6653200449205,37.6290550819801,38.790695629662));
#30744=CARTESIAN_POINT('Ctrl Pts',(-41.6878975169869,37.6610244204632,38.811966451168));
#30745=CARTESIAN_POINT('Ctrl Pts',(-41.7104749890533,37.6929937589462,38.833237272674));
#30746=CARTESIAN_POINT('Ctrl Pts',(-41.7327620421608,37.7253771373014,38.854194064383));
#30747=CARTESIAN_POINT('Ctrl Pts',(-41.7547507170926,37.7581629906826,38.8748293421447));
#30748=CARTESIAN_POINT('Ctrl Pts',(-41.7767393920243,37.7909488440638,38.8954646199064));
#30749=CARTESIAN_POINT('Ctrl Pts',(-41.7984296884063,37.8241371719135,38.9157783833699));
#30750=CARTESIAN_POINT('Ctrl Pts',(-41.8198138601368,37.8577161219199,38.9357633780249));
#30751=CARTESIAN_POINT('Ctrl Pts',(-41.8411980318674,37.8912950719261,38.95574837268));
#30752=CARTESIAN_POINT('Ctrl Pts',(-41.8622760785829,37.925264643518,38.9754045981869));
#30753=CARTESIAN_POINT('Ctrl Pts',(-41.8830404728302,37.9596127053833,38.9947250348572));
#30754=CARTESIAN_POINT('Ctrl Pts',(-41.9038048670775,37.9939607672486,39.0140454715275));
#30755=CARTESIAN_POINT('Ctrl Pts',(-41.9242556085034,38.0286873188033,39.0330301190327));
#30756=CARTESIAN_POINT('Ctrl Pts',(-41.9443853936797,38.0637799584006,39.0516721975204));
#30757=CARTESIAN_POINT('Ctrl Pts',(-41.9645151788561,38.0988725979979,39.0703142760081));
#30758=CARTESIAN_POINT('Ctrl Pts',(-41.9843240074406,38.1343313250409,39.0886137851613));
#30759=CARTESIAN_POINT('Ctrl Pts',(-42.003804805247,38.1701434764062,39.1065641898061));
#30760=CARTESIAN_POINT('Ctrl Pts',(-42.0232856030534,38.2059556277714,39.1245145944509));
#30761=CARTESIAN_POINT('Ctrl Pts',(-42.0424383697503,38.2421212028499,39.142115894282));
#30762=CARTESIAN_POINT('Ctrl Pts',(-42.0612562654461,38.2786272860865,39.1593618034723));
#30763=CARTESIAN_POINT('Ctrl Pts',(-42.0800741611419,38.315133369323,39.1766077126626));
#30764=CARTESIAN_POINT('Ctrl Pts',(-42.0985571855166,38.3519799600968,39.1934982309186));
#30765=CARTESIAN_POINT('Ctrl Pts',(-42.1166987378588,38.3891538996466,39.2100273262496));
#30766=CARTESIAN_POINT('Ctrl Pts',(-42.1348402902011,38.4263278391962,39.2265564215806));
#30767=CARTESIAN_POINT('Ctrl Pts',(-42.1526403702024,38.4638291268896,39.2427240937055));
#30768=CARTESIAN_POINT('Ctrl Pts',(-42.1700926210466,38.5016443701579,39.2585245687782));
#30769=CARTESIAN_POINT('Ctrl Pts',(-42.1875448718908,38.5394596134262,39.2743250438509));
#30770=CARTESIAN_POINT('Ctrl Pts',(-42.204649293281,38.5775888116264,39.2897583216026));
#30771=CARTESIAN_POINT('Ctrl Pts',(-42.2213997768367,38.6160183479486,39.3048188904566));
#30772=CARTESIAN_POINT('Ctrl Pts',(-42.2381502603923,38.6544478842708,39.3198794593106));
#30773=CARTESIAN_POINT('Ctrl Pts',(-42.2545468058286,38.6931777580614,39.3345673190107));
#30774=CARTESIAN_POINT('Ctrl Pts',(-42.2705835575636,38.7321941379955,39.3488772241858));
#30775=CARTESIAN_POINT('Ctrl Pts',(-42.2866203092985,38.7712105179296,39.3631871293609));
#30776=CARTESIAN_POINT('Ctrl Pts',(-42.3022972670594,38.8105134033437,39.3771190797676));
#30777=CARTESIAN_POINT('Ctrl Pts',(-42.3176088322457,38.8500887582774,39.3906680999874));
#30778=CARTESIAN_POINT('Ctrl Pts',(-42.332934005473,38.8896992855169,39.4042291617993));
#30779=CARTESIAN_POINT('Ctrl Pts',(-42.3478931360962,38.9295827661274,39.4174066122383));
#30780=CARTESIAN_POINT('Ctrl Pts',(-42.3624808722509,38.9697249315629,39.4301957368445));
#30781=CARTESIAN_POINT('Ctrl Pts',(-41.3841443126071,37.2989165355258,38.5613374331557));
#30782=CARTESIAN_POINT('Ctrl Pts',(-41.4096119890754,37.3282515811861,38.5857420631406));
#30783=CARTESIAN_POINT('Ctrl Pts',(-41.4348077478983,37.3580712533658,38.6098479198828));
#30784=CARTESIAN_POINT('Ctrl Pts',(-41.4597220673956,37.3883642844818,38.6336458952033));
#30785=CARTESIAN_POINT('Ctrl Pts',(-41.4846363868929,37.4186573155978,38.6574438705238));
#30786=CARTESIAN_POINT('Ctrl Pts',(-41.5092692665914,37.4494237050751,38.6809339639707));
#30787=CARTESIAN_POINT('Ctrl Pts',(-41.5336113971655,37.4806518281381,38.704107299671));
#30788=CARTESIAN_POINT('Ctrl Pts',(-41.5579535277396,37.5118799512011,38.7272806353713));
#30789=CARTESIAN_POINT('Ctrl Pts',(-41.582004908727,37.5435698072571,38.7501372128852));
#30790=CARTESIAN_POINT('Ctrl Pts',(-41.6057564501721,37.5757094230964,38.7726683953334));
#30791=CARTESIAN_POINT('Ctrl Pts',(-41.6295079916173,37.6078490389357,38.7951995777818));
#30792=CARTESIAN_POINT('Ctrl Pts',(-41.652959693069,37.6404384139483,38.8174053647368));
#30793=CARTESIAN_POINT('Ctrl Pts',(-41.6761026907923,37.6734652355113,38.8392773648215));
#30794=CARTESIAN_POINT('Ctrl Pts',(-41.6992456885155,37.7064920570744,38.8611493649062));
#30795=CARTESIAN_POINT('Ctrl Pts',(-41.7220799820707,37.7399563245612,38.8826875777052));
#30796=CARTESIAN_POINT('Ctrl Pts',(-41.7445969406233,37.7738453952121,38.9038838636666));
#30797=CARTESIAN_POINT('Ctrl Pts',(-41.7671138991759,37.8077344658628,38.925080149628));
#30798=CARTESIAN_POINT('Ctrl Pts',(-41.7893135222983,37.8420483390345,38.9459345083493));
#30799=CARTESIAN_POINT('Ctrl Pts',(-41.8111874185617,37.8767740513551,38.9664390582374));
#30800=CARTESIAN_POINT('Ctrl Pts',(-41.833061314825,37.9114997636757,38.9869436081255));
#30801=CARTESIAN_POINT('Ctrl Pts',(-41.8546094838138,37.9466373144864,39.0070983487909));
#30802=CARTESIAN_POINT('Ctrl Pts',(-41.8758237798296,37.9821734295689,39.0268956625394));
#30803=CARTESIAN_POINT('Ctrl Pts',(-41.8970380758455,38.0177095446515,39.0466929762878));
#30804=CARTESIAN_POINT('Ctrl Pts',(-41.9179184984855,38.0536442233315,39.0661328627431));
#30805=CARTESIAN_POINT('Ctrl Pts',(-41.9384571539217,38.0899638905448,39.0852079738506));
#30806=CARTESIAN_POINT('Ctrl Pts',(-41.9589958093579,38.1262835577581,39.1042830849581));
#30807=CARTESIAN_POINT('Ctrl Pts',(-41.9791926972001,38.1629882128155,39.1229934203554));
#30808=CARTESIAN_POINT('Ctrl Pts',(-41.9990401814417,38.2000639900327,39.1413319071658));
#30809=CARTESIAN_POINT('Ctrl Pts',(-42.0188876656832,38.2371397672498,39.1596703939762));
#30810=CARTESIAN_POINT('Ctrl Pts',(-42.0383857459468,38.2745866659233,39.1776370318513));
#30811=CARTESIAN_POINT('Ctrl Pts',(-42.0575270498033,38.3123905401941,39.1952250284238));
#30812=CARTESIAN_POINT('Ctrl Pts',(-42.0766683536599,38.350194414465,39.2128130249963));
#30813=CARTESIAN_POINT('Ctrl Pts',(-42.0954528807456,38.3883552636159,39.2300223799319));
#30814=CARTESIAN_POINT('Ctrl Pts',(-42.1138735277671,38.4268586722694,39.2468465864931));
#30815=CARTESIAN_POINT('Ctrl Pts',(-42.1322941747887,38.4653620809229,39.2636707930542));
#30816=CARTESIAN_POINT('Ctrl Pts',(-42.150350941396,38.5042080483483,39.2801098509211));
#30817=CARTESIAN_POINT('Ctrl Pts',(-42.1680369987875,38.5433819005085,39.296157543891));
#30818=CARTESIAN_POINT('Ctrl Pts',(-42.1857230561791,38.5825557526686,39.312205236861));
#30819=CARTESIAN_POINT('Ctrl Pts',(-42.2030384040184,38.6220574888201,39.3278615646289));
#30820=CARTESIAN_POINT('Ctrl Pts',(-42.2199764931453,38.6618721873199,39.3431206062142));
#30821=CARTESIAN_POINT('Ctrl Pts',(-42.2369145822722,38.7016868858197,39.3583796477995));
#30822=CARTESIAN_POINT('Ctrl Pts',(-42.2534754123644,38.7418145459123,39.3732414029119));
#30823=CARTESIAN_POINT('Ctrl Pts',(-42.2696527188415,38.7822400095886,39.3877002502575));
#30824=CARTESIAN_POINT('Ctrl Pts',(-42.2858300253186,38.8226654732649,39.402159097603));
#30825=CARTESIAN_POINT('Ctrl Pts',(-42.3016238078729,38.863388739758,39.4162150369067));
#30826=CARTESIAN_POINT('Ctrl Pts',(-42.317028091229,38.9043944261112,39.4298627508005));
#30827=CARTESIAN_POINT('Ctrl Pts',(-42.3324460650287,38.9454365559668,39.4435225939999));
#30828=CARTESIAN_POINT('Ctrl Pts',(-42.3474738466997,38.9867616071232,39.4567734855919));
#30829=CARTESIAN_POINT('Ctrl Pts',(-42.3621057396173,39.0283539416435,39.4696104027777));
#30830=CARTESIAN_POINT('Ctrl Pts',(-41.3647023344627,37.2998230939851,38.5805023326933));
#30831=CARTESIAN_POINT('Ctrl Pts',(-41.3908423574775,37.3299783140399,38.6056254203547));
#30832=CARTESIAN_POINT('Ctrl Pts',(-41.4166950335924,37.3606456594132,38.6304327816703));
#30833=CARTESIAN_POINT('Ctrl Pts',(-41.4422500364264,37.3918128820555,38.6549145092738));
#30834=CARTESIAN_POINT('Ctrl Pts',(-41.4678050392604,37.4229801046978,38.6793962368773));
#30835=CARTESIAN_POINT('Ctrl Pts',(-41.4930623682715,37.4546472039489,38.7035523302504));
#30836=CARTESIAN_POINT('Ctrl Pts',(-41.5180119344913,37.4868015330437,38.7273731417376));
#30837=CARTESIAN_POINT('Ctrl Pts',(-41.5429615007111,37.5189558621386,38.7511939532247));
#30838=CARTESIAN_POINT('Ctrl Pts',(-41.5676033036101,37.5515974203945,38.77467948232));
#30839=CARTESIAN_POINT('Ctrl Pts',(-41.5919274996662,37.5847131724031,38.797820348766));
#30840=CARTESIAN_POINT('Ctrl Pts',(-41.6162516957224,37.6178289244116,38.8209612152119));
#30841=CARTESIAN_POINT('Ctrl Pts',(-41.6402582844198,37.6514188694715,38.8437574185185));
#30842=CARTESIAN_POINT('Ctrl Pts',(-41.6639376755246,37.6854695939044,38.8661998532878));
#30843=CARTESIAN_POINT('Ctrl Pts',(-41.6876170666294,37.7195203183375,38.888642288057));
#30844=CARTESIAN_POINT('Ctrl Pts',(-41.7109692596392,37.7540318214229,38.9107309538146));
#30845=CARTESIAN_POINT('Ctrl Pts',(-41.7339849252473,37.7889903219007,38.9324570272832));
#30846=CARTESIAN_POINT('Ctrl Pts',(-41.7570005908553,37.8239488223784,38.9541831007517));
#30847=CARTESIAN_POINT('Ctrl Pts',(-41.7796797285733,37.8593543195073,38.9755465814704));
#30848=CARTESIAN_POINT('Ctrl Pts',(-41.8020132774537,37.8951926754153,38.9965389353068));
#30849=CARTESIAN_POINT('Ctrl Pts',(-41.8243468263341,37.9310310313234,39.0175312891431));
#30850=CARTESIAN_POINT('Ctrl Pts',(-41.846334785903,37.9673022452508,39.0381525156518));
#30851=CARTESIAN_POINT('Ctrl Pts',(-41.8679683707908,38.0039918339702,39.0583943766432));
#30852=CARTESIAN_POINT('Ctrl Pts',(-41.8896019556786,38.0406814226895,39.0786362376347));
#30853=CARTESIAN_POINT('Ctrl Pts',(-41.910881165426,38.0777893854232,39.0984987326795));
#30854=CARTESIAN_POINT('Ctrl Pts',(-41.931797497241,38.1153009051195,39.1179739260933));
#30855=CARTESIAN_POINT('Ctrl Pts',(-41.9527138290561,38.1528124248159,39.1374491195071));
#30856=CARTESIAN_POINT('Ctrl Pts',(-41.973267282494,38.190727500674,39.1565370108716));
#30857=CARTESIAN_POINT('Ctrl Pts',(-41.9934496441163,38.2290309936264,39.1752299733406));
#30858=CARTESIAN_POINT('Ctrl Pts',(-42.0136320057387,38.2673344865787,39.1939229358096));
#30859=CARTESIAN_POINT('Ctrl Pts',(-42.0334432751162,38.3060263958077,39.2122209689812));
#30860=CARTESIAN_POINT('Ctrl Pts',(-42.0528755347069,38.34509127226,39.2301167609037));
#30861=CARTESIAN_POINT('Ctrl Pts',(-42.0723077942975,38.3841561487124,39.2480125528261));
#30862=CARTESIAN_POINT('Ctrl Pts',(-42.0913610436888,38.4235939915674,39.2655061031254));
#30863=CARTESIAN_POINT('Ctrl Pts',(-42.1100276675451,38.4633890540822,39.2825904205687));
#30864=CARTESIAN_POINT('Ctrl Pts',(-42.1286942914013,38.503184116597,39.2996747380119));
#30865=CARTESIAN_POINT('Ctrl Pts',(-42.146974289326,38.543336397925,39.316349822234));
#30866=CARTESIAN_POINT('Ctrl Pts',(-42.164860354262,38.583829866219,39.3326090083328));
#30867=CARTESIAN_POINT('Ctrl Pts',(-42.182746419198,38.6243233345131,39.3488681944315));
#30868=CARTESIAN_POINT('Ctrl Pts',(-42.200238550765,38.6651579889162,39.3647114820621));
#30869=CARTESIAN_POINT('Ctrl Pts',(-42.2173297560061,38.7063175251639,39.3801325379038));
#30870=CARTESIAN_POINT('Ctrl Pts',(-42.2344209612472,38.7474770614115,39.3955535937456));
#30871=CARTESIAN_POINT('Ctrl Pts',(-42.2511112397995,38.7889614786422,39.4105524174792));
#30872=CARTESIAN_POINT('Ctrl Pts',(-42.267393918383,38.8307542132177,39.4251230124646));
#30873=CARTESIAN_POINT('Ctrl Pts',(-42.2836765969667,38.8725469477931,39.43969360745));
#30874=CARTESIAN_POINT('Ctrl Pts',(-42.2995516752353,38.9146479988278,39.4538359733773));
#30875=CARTESIAN_POINT('Ctrl Pts',(-42.3150128049069,38.9570405564743,39.467544455051));
#30876=CARTESIAN_POINT('Ctrl Pts',(-42.3304876755439,38.9994707901951,39.481265120037));
#30877=CARTESIAN_POINT('Ctrl Pts',(-42.3455478611398,39.0421930480067,39.4945511289116));
#30878=CARTESIAN_POINT('Ctrl Pts',(-42.3601873274122,39.0851902417554,39.5073971582654));
#30879=CARTESIAN_POINT('Ctrl Pts',(-41.3452377207148,37.3007032273757,38.5996449702406));
#30880=CARTESIAN_POINT('Ctrl Pts',(-41.3720280192526,37.3316517033458,38.6254629394162));
#30881=CARTESIAN_POINT('Ctrl Pts',(-41.3985154762073,37.3631399200295,38.6509481572531));
#30882=CARTESIAN_POINT('Ctrl Pts',(-41.424688926481,37.3951546043889,38.6760898811217));
#30883=CARTESIAN_POINT('Ctrl Pts',(-41.4508623767548,37.4271692887483,38.7012316049902));
#30884=CARTESIAN_POINT('Ctrl Pts',(-41.4767218197276,37.4597104400256,38.7260298342954));
#30885=CARTESIAN_POINT('Ctrl Pts',(-41.502256355026,37.4927643413466,38.7504741159893));
#30886=CARTESIAN_POINT('Ctrl Pts',(-41.5277908903244,37.5258182426675,38.7749183976833));
#30887=CARTESIAN_POINT('Ctrl Pts',(-41.5530005173431,37.5593848932482,38.7990087311859));
#30888=CARTESIAN_POINT('Ctrl Pts',(-41.5778746096208,37.5934501439432,38.8227349618473));
#30889=CARTESIAN_POINT('Ctrl Pts',(-41.6027487018984,37.6275153946382,38.8464611925086));
#30890=CARTESIAN_POINT('Ctrl Pts',(-41.6272872588458,37.6620792446412,38.8698233197672));
#30891=CARTESIAN_POINT('Ctrl Pts',(-41.6514799368739,37.6971271244599,38.892811495924));
#30892=CARTESIAN_POINT('Ctrl Pts',(-41.675672614902,37.7321750042785,38.9157996720809));
#30893=CARTESIAN_POINT('Ctrl Pts',(-41.6995194134375,37.7677069130834,38.9384138965928));
#30894=CARTESIAN_POINT('Ctrl Pts',(-41.7230102804842,37.8037078733246,38.960644637023));
#30895=CARTESIAN_POINT('Ctrl Pts',(-41.7465011475309,37.8397088335659,38.9828753774532));
#30896=CARTESIAN_POINT('Ctrl Pts',(-41.7696360825321,37.8761788443904,39.0047226332749));
#30897=CARTESIAN_POINT('Ctrl Pts',(-41.792405333559,37.913102532816,39.0261771953468));
#30898=CARTESIAN_POINT('Ctrl Pts',(-41.815174584586,37.9500262212414,39.0476317574188));
#30899=CARTESIAN_POINT('Ctrl Pts',(-41.8375781510992,37.9874035863929,39.0686936252327));
#30900=CARTESIAN_POINT('Ctrl Pts',(-41.8596065894592,38.0252188728165,39.0893539207072));
#30901=CARTESIAN_POINT('Ctrl Pts',(-41.8816350278192,38.0630341592401,39.1100142161817));
#30902=CARTESIAN_POINT('Ctrl Pts',(-41.903288337504,38.1012873660397,39.1302729388273));
#30903=CARTESIAN_POINT('Ctrl Pts',(-41.9245573911254,38.1399623685732,39.1501215491074));
#30904=CARTESIAN_POINT('Ctrl Pts',(-41.9458264447468,38.1786373711068,39.1699701593876));
#30905=CARTESIAN_POINT('Ctrl Pts',(-41.9667112418003,38.2177341684525,39.1894086568271));
#30906=CARTESIAN_POINT('Ctrl Pts',(-41.9872029788452,38.257236280385,39.2084288476439));
#30907=CARTESIAN_POINT('Ctrl Pts',(-42.00769471589,38.2967383923175,39.2274490384606));
#30908=CARTESIAN_POINT('Ctrl Pts',(-42.0277933924401,38.3366458178957,39.2460509221991));
#30909=CARTESIAN_POINT('Ctrl Pts',(-42.0474905364223,38.3769417351846,39.2642266577201));
#30910=CARTESIAN_POINT('Ctrl Pts',(-42.0671876804046,38.4172376524736,39.2824023932411));
#30911=CARTESIAN_POINT('Ctrl Pts',(-42.0864832913524,38.4579220605255,39.3001519801198));
#30912=CARTESIAN_POINT('Ctrl Pts',(-42.1053692357035,38.498977809875,39.3174679364691));
#30913=CARTESIAN_POINT('Ctrl Pts',(-42.1242551800547,38.5400335592245,39.3347838928183));
#30914=CARTESIAN_POINT('Ctrl Pts',(-42.1427314573616,38.5814606488959,39.3516662182258));
#30915=CARTESIAN_POINT('Ctrl Pts',(-42.1607902794319,38.6232416163983,39.3681077964026));
#30916=CARTESIAN_POINT('Ctrl Pts',(-42.1788491015022,38.6650225839007,39.3845493745794));
#30917=CARTESIAN_POINT('Ctrl Pts',(-42.1964904679075,38.7071574282453,39.4005502051364));
#30918=CARTESIAN_POINT('Ctrl Pts',(-42.2137069423898,38.7496283885661,39.4161035433246));
#30919=CARTESIAN_POINT('Ctrl Pts',(-42.2309234168721,38.7920993488871,39.4316568815127));
#30920=CARTESIAN_POINT('Ctrl Pts',(-42.2477149990234,38.834906424188,39.4467627269715));
#30921=CARTESIAN_POINT('Ctrl Pts',(-42.2640746107899,38.8780315702624,39.4614147122255));
#30922=CARTESIAN_POINT('Ctrl Pts',(-42.2804342225564,38.9211567163368,39.4760666974795));
#30923=CARTESIAN_POINT('Ctrl Pts',(-42.2963618635506,38.9645999321627,39.4902648221815));
#30924=CARTESIAN_POINT('Ctrl Pts',(-42.3118508198906,39.008342905385,39.5040031014822));
#30925=CARTESIAN_POINT('Ctrl Pts',(-42.3273535419267,39.0521247548533,39.5177535905777));
#30926=CARTESIAN_POINT('Ctrl Pts',(-42.3424167988389,39.0962068937307,39.531043416214));
#30927=CARTESIAN_POINT('Ctrl Pts',(-42.3570342296479,39.1405707074102,39.5438669662772));
#30928=CARTESIAN_POINT('Ctrl Pts',(-41.325773106967,37.3015833607663,38.6187876077879));
#30929=CARTESIAN_POINT('Ctrl Pts',(-41.3532136810277,37.3333250926518,38.6453004584778));
#30930=CARTESIAN_POINT('Ctrl Pts',(-41.3803359188222,37.3656341806458,38.6714635328359));
#30931=CARTESIAN_POINT('Ctrl Pts',(-41.4071278165357,37.3984963267223,38.6972652529695));
#30932=CARTESIAN_POINT('Ctrl Pts',(-41.4339197142492,37.4313584727989,38.723066973103));
#30933=CARTESIAN_POINT('Ctrl Pts',(-41.4603812711837,37.4647736761024,38.7485073383404));
#30934=CARTESIAN_POINT('Ctrl Pts',(-41.4865007755607,37.4987271496494,38.7735750902411));
#30935=CARTESIAN_POINT('Ctrl Pts',(-41.5126202799377,37.5326806231965,38.7986428421418));
#30936=CARTESIAN_POINT('Ctrl Pts',(-41.5383977310762,37.5671723661017,38.8233379800519));
#30937=CARTESIAN_POINT('Ctrl Pts',(-41.5638217195754,37.6021871154832,38.8476495749286));
#30938=CARTESIAN_POINT('Ctrl Pts',(-41.5892457080746,37.6372018648648,38.8719611698053));
#30939=CARTESIAN_POINT('Ctrl Pts',(-41.6143162332718,37.6727396198109,38.8958892210159));
#30940=CARTESIAN_POINT('Ctrl Pts',(-41.6390221982231,37.7087846550152,38.9194231385604));
#30941=CARTESIAN_POINT('Ctrl Pts',(-41.6637281631745,37.7448296902195,38.9429570561048));
#30942=CARTESIAN_POINT('Ctrl Pts',(-41.6880695672358,37.7813820047439,38.966096839371));
#30943=CARTESIAN_POINT('Ctrl Pts',(-41.7120356357211,37.8184254247486,38.9888322467629));
#30944=CARTESIAN_POINT('Ctrl Pts',(-41.7360017042064,37.8554688447534,39.0115676541547));
#30945=CARTESIAN_POINT('Ctrl Pts',(-41.7595924364909,37.8930033692735,39.0338986850794));
#30946=CARTESIAN_POINT('Ctrl Pts',(-41.7827973896644,37.9310123902165,39.0558154553869));
#30947=CARTESIAN_POINT('Ctrl Pts',(-41.8060023428379,37.9690214111595,39.0777322256945));
#30948=CARTESIAN_POINT('Ctrl Pts',(-41.8288215162954,38.007504927535,39.0992347348136));
#30949=CARTESIAN_POINT('Ctrl Pts',(-41.8512448081276,38.0464459116628,39.1203134647711));
#30950=CARTESIAN_POINT('Ctrl Pts',(-41.8736680999599,38.0853868957906,39.1413921947287));
#30951=CARTESIAN_POINT('Ctrl Pts',(-41.895695509582,38.1247853466562,39.1620471449751));
#30952=CARTESIAN_POINT('Ctrl Pts',(-41.9173172850097,38.164623832027,39.1822691721216));
#30953=CARTESIAN_POINT('Ctrl Pts',(-41.9389390604375,38.2044623173978,39.202491199268));
#30954=CARTESIAN_POINT('Ctrl Pts',(-41.9601552011066,38.2447408362309,39.2222803027826));
#30955=CARTESIAN_POINT('Ctrl Pts',(-41.980956313574,38.2854415671435,39.2416277219471));
#30956=CARTESIAN_POINT('Ctrl Pts',(-42.0017574260413,38.3261422980563,39.2609751411116));
#30957=CARTESIAN_POINT('Ctrl Pts',(-42.0221435097639,38.3672652399837,39.2798808754169));
#30958=CARTESIAN_POINT('Ctrl Pts',(-42.0421055381378,38.4087921981093,39.2983365545365));
#30959=CARTESIAN_POINT('Ctrl Pts',(-42.0620675665116,38.450319156235,39.3167922336561));
#30960=CARTESIAN_POINT('Ctrl Pts',(-42.081605539016,38.4922501294836,39.3347978571142));
#30961=CARTESIAN_POINT('Ctrl Pts',(-42.100710803862,38.5345665656678,39.3523454523695));
#30962=CARTESIAN_POINT('Ctrl Pts',(-42.119816068708,38.5768830018521,39.3698930476248));
#30963=CARTESIAN_POINT('Ctrl Pts',(-42.1384886253973,38.6195848998668,39.3869826142177));
#30964=CARTESIAN_POINT('Ctrl Pts',(-42.1567202046019,38.6626533665775,39.4036065844725));
#30965=CARTESIAN_POINT('Ctrl Pts',(-42.1749517838064,38.7057218332882,39.4202305547273));
#30966=CARTESIAN_POINT('Ctrl Pts',(-42.1927423850501,38.7491568675743,39.4363889282107));
#30967=CARTESIAN_POINT('Ctrl Pts',(-42.2100841287736,38.7929392519684,39.4520745487453));
#30968=CARTESIAN_POINT('Ctrl Pts',(-42.2274258724969,38.8367216363625,39.4677601692799));
#30969=CARTESIAN_POINT('Ctrl Pts',(-42.2443187582472,38.8808513697338,39.4829730364638));
#30970=CARTESIAN_POINT('Ctrl Pts',(-42.2607553031968,38.925308927307,39.4977064119864));
#30971=CARTESIAN_POINT('Ctrl Pts',(-42.2771918481463,38.9697664848803,39.512439787509));
#30972=CARTESIAN_POINT('Ctrl Pts',(-42.2931720518659,39.0145518654976,39.5266936709857));
#30973=CARTESIAN_POINT('Ctrl Pts',(-42.3086888348743,39.0596452542956,39.5404617479134));
#30974=CARTESIAN_POINT('Ctrl Pts',(-42.3242194083095,39.1047787195115,39.5542420611184));
#30975=CARTESIAN_POINT('Ctrl Pts',(-42.339285736538,39.1502207394548,39.5675357035164));
#30976=CARTESIAN_POINT('Ctrl Pts',(-42.3538811318835,39.1959511730649,39.5803367742889));
#30977=CARTESIAN_POINT('Ctrl Pts',(-41.3062858049163,37.3024370075663,38.6379079315151));
#30978=CARTESIAN_POINT('Ctrl Pts',(-41.3343545286771,37.3349450157083,38.665092038194));
#30979=CARTESIAN_POINT('Ctrl Pts',(-41.3620893558469,37.3680481123285,38.6919092714245));
#30980=CARTESIAN_POINT('Ctrl Pts',(-41.389477409864,37.4017309298736,38.7183471819599));
#30981=CARTESIAN_POINT('Ctrl Pts',(-41.416865463881,37.4354137474188,38.7447850924952));
#30982=CARTESIAN_POINT('Ctrl Pts',(-41.4439067439596,37.469676284923,38.7708436795772));
#30983=CARTESIAN_POINT('Ctrl Pts',(-41.4705886951389,37.5045026371562,38.7965108457472));
#30984=CARTESIAN_POINT('Ctrl Pts',(-41.4972706463182,37.5393289893894,38.8221780119171));
#30985=CARTESIAN_POINT('Ctrl Pts',(-41.5235932678327,37.574719155353,38.8474537564389));
#30986=CARTESIAN_POINT('Ctrl Pts',(-41.5495443379544,37.6106567068741,38.8723263448488));
#30987=CARTESIAN_POINT('Ctrl Pts',(-41.5754954080762,37.6465942583951,38.8971989332587));
#30988=CARTESIAN_POINT('Ctrl Pts',(-41.6010749260608,37.6830791944433,38.9216683648434));
#30989=CARTESIAN_POINT('Ctrl Pts',(-41.6262710147375,37.7200945791203,38.9457232790054));
#30990=CARTESIAN_POINT('Ctrl Pts',(-41.6514671034143,37.7571099637973,38.9697781931674));
#30991=CARTESIAN_POINT('Ctrl Pts',(-41.6762797620602,37.794655796042,38.9934185892169));
#30992=CARTESIAN_POINT('Ctrl Pts',(-41.7006974690671,37.8327146479188,39.0166334909482));
#30993=CARTESIAN_POINT('Ctrl Pts',(-41.725115176074,37.8707734997956,39.0398483926795));
#30994=CARTESIAN_POINT('Ctrl Pts',(-41.7491379307412,37.9093453702133,39.0626377994268));
#30995=CARTESIAN_POINT('Ctrl Pts',(-41.7727545776992,37.9484123553418,39.0849911295462));
#30996=CARTESIAN_POINT('Ctrl Pts',(-41.7963712246572,37.9874793404703,39.1073444596656));
#30997=CARTESIAN_POINT('Ctrl Pts',(-41.8195817632284,38.0270414391895,39.1292617125159));
#30998=CARTESIAN_POINT('Ctrl Pts',(-41.8423754146195,38.0670802883583,39.1507327108198));
#30999=CARTESIAN_POINT('Ctrl Pts',(-41.8651690660106,38.107119137527,39.1722037091237));
#31000=CARTESIAN_POINT('Ctrl Pts',(-41.8875458295674,38.1476347359975,39.193228452265));
#31001=CARTESIAN_POINT('Ctrl Pts',(-41.9094953130622,38.1886082783258,39.213797176764));
#31002=CARTESIAN_POINT('Ctrl Pts',(-41.931444796557,38.2295818206541,39.2343659012629));
#31003=CARTESIAN_POINT('Ctrl Pts',(-41.9529669993598,38.2710133056656,39.2544786065292));
#31004=CARTESIAN_POINT('Ctrl Pts',(-41.9740519254398,38.3128835030316,39.274125951928));
#31005=CARTESIAN_POINT('Ctrl Pts',(-41.9951368515198,38.3547537003978,39.2937732973269));
#31006=CARTESIAN_POINT('Ctrl Pts',(-42.0157845002718,38.3970626089183,39.3129552822944));
#31007=CARTESIAN_POINT('Ctrl Pts',(-42.035985281127,38.439790591191,39.3316629976981));
#31008=CARTESIAN_POINT('Ctrl Pts',(-42.0561860619822,38.4825185734638,39.3503707131017));
#31009=CARTESIAN_POINT('Ctrl Pts',(-42.0759399743606,38.5256656282641,39.3686041584044));
#31010=CARTESIAN_POINT('Ctrl Pts',(-42.0952378420455,38.5692117293042,39.3863548642333));
#31011=CARTESIAN_POINT('Ctrl Pts',(-42.1145357097305,38.6127578303443,39.4041055700621));
#31012=CARTESIAN_POINT('Ctrl Pts',(-42.1333775321678,38.6567029763761,39.4213735359074));
#31013=CARTESIAN_POINT('Ctrl Pts',(-42.1517545559995,38.7010267707748,39.438150740007));
#31014=CARTESIAN_POINT('Ctrl Pts',(-42.1701315798312,38.7453505651734,39.4549279441066));
#31015=CARTESIAN_POINT('Ctrl Pts',(-42.1880438045295,38.7900530066685,39.4712143859786));
#31016=CARTESIAN_POINT('Ctrl Pts',(-42.2054829077106,38.8351133471886,39.487002498908));
#31017=CARTESIAN_POINT('Ctrl Pts',(-42.2229220108917,38.8801736877088,39.5027906118375));
#31018=CARTESIAN_POINT('Ctrl Pts',(-42.2398879920545,38.9255919259625,39.5180803953709));
#31019=CARTESIAN_POINT('Ctrl Pts',(-42.2563729675066,38.9713469816487,39.5328647448567));
#31020=CARTESIAN_POINT('Ctrl Pts',(-42.2728579429587,39.0171020373349,39.5476490943425));
#31021=CARTESIAN_POINT('Ctrl Pts',(-42.2888619122262,39.0631939091422,39.5619280093558));
#31022=CARTESIAN_POINT('Ctrl Pts',(-42.3043774376187,39.1096012040638,39.5756948538967));
#31023=CARTESIAN_POINT('Ctrl Pts',(-42.3199067523203,39.1560497431279,39.5894739336195));
#31024=CARTESIAN_POINT('Ctrl Pts',(-42.3349467541126,39.2028142648828,39.6027400318712));
#31025=CARTESIAN_POINT('Ctrl Pts',(-42.3494904395659,39.2498730255593,39.6154869710169));
#31026=CARTESIAN_POINT('Ctrl Pts',(-41.2867801198513,37.3032691938199,38.6570101756496));
#31027=CARTESIAN_POINT('Ctrl Pts',(-41.3154590259865,37.3365214462081,38.6848461534539));
#31028=CARTESIAN_POINT('Ctrl Pts',(-41.3437884160841,37.3703966248004,38.7122980957319));
#31029=CARTESIAN_POINT('Ctrl Pts',(-41.3717545086029,37.4048782501681,38.739352647799));
#31030=CARTESIAN_POINT('Ctrl Pts',(-41.3997206011217,37.4393598755357,38.7664071998661));
#31031=CARTESIAN_POINT('Ctrl Pts',(-41.4273233951791,37.4744479465903,38.7930643608684));
#31032=CARTESIAN_POINT('Ctrl Pts',(-41.4545494627047,37.510125393861,38.8193111627622));
#31033=CARTESIAN_POINT('Ctrl Pts',(-41.4817755302303,37.5458028411317,38.8455579646562));
#31034=CARTESIAN_POINT('Ctrl Pts',(-41.5086248703647,37.5820696634925,38.8713944066132));
#31035=CARTESIAN_POINT('Ctrl Pts',(-41.5350844215741,37.6189082180394,38.8968079198494));
#31036=CARTESIAN_POINT('Ctrl Pts',(-41.5615439727835,37.6557467725863,38.9222214330856));
#31037=CARTESIAN_POINT('Ctrl Pts',(-41.5876137342328,37.6931570581567,38.9472120167988));
#31038=CARTESIAN_POINT('Ctrl Pts',(-41.6132810236338,37.7311208755803,38.9717675136936));
#31039=CARTESIAN_POINT('Ctrl Pts',(-41.6389483130347,37.7690846930039,38.9963230105884));
#31040=CARTESIAN_POINT('Ctrl Pts',(-41.6642131295771,37.8076020410825,39.02044341989));
#31041=CARTESIAN_POINT('Ctrl Pts',(-41.6890631825583,37.8466541820877,39.0441170076211));
#31042=CARTESIAN_POINT('Ctrl Pts',(-41.7139132355395,37.8857063230928,39.0677905953522));
#31043=CARTESIAN_POINT('Ctrl Pts',(-41.7383485241752,37.9252932557919,39.0910173607657));
#31044=CARTESIAN_POINT('Ctrl Pts',(-41.7623571613074,37.9653957221302,39.1137860046199));
#31045=CARTESIAN_POINT('Ctrl Pts',(-41.7863657984395,38.0054981884685,39.1365546484741));
#31046=CARTESIAN_POINT('Ctrl Pts',(-41.8099477833104,38.0461161871802,39.1588651700504));
#31047=CARTESIAN_POINT('Ctrl Pts',(-41.8330916438728,38.0872299586229,39.1807067158369));
#31048=CARTESIAN_POINT('Ctrl Pts',(-41.8562355044352,38.1283437300656,39.2025482616234));
#31049=CARTESIAN_POINT('Ctrl Pts',(-41.8789412399588,38.1699532729415,39.2239208309306));
#31050=CARTESIAN_POINT('Ctrl Pts',(-41.9011978046699,38.2120383452466,39.2448140265372));
#31051=CARTESIAN_POINT('Ctrl Pts',(-41.923454369381,38.2541234175516,39.2657072221438));
#31052=CARTESIAN_POINT('Ctrl Pts',(-41.9452617625771,38.2966840179575,39.2861210433902));
#31053=CARTESIAN_POINT('Ctrl Pts',(-41.9666093755058,38.3396994417945,39.3060455594619));
#31054=CARTESIAN_POINT('Ctrl Pts',(-41.9879569884345,38.3827148656314,39.3259700755336));
#31055=CARTESIAN_POINT('Ctrl Pts',(-42.0088448204219,38.4261851115417,39.3454052858018));
#31056=CARTESIAN_POINT('Ctrl Pts',(-42.0292627100592,38.4700890323357,39.3643417355216));
#31057=CARTESIAN_POINT('Ctrl Pts',(-42.0496805996965,38.5139929531297,39.3832781852415));
#31058=CARTESIAN_POINT('Ctrl Pts',(-42.0696285463391,38.5583305474217,39.4017158738155));
#31059=CARTESIAN_POINT('Ctrl Pts',(-42.089096845809,38.6030802460786,39.4196458317682));
#31060=CARTESIAN_POINT('Ctrl Pts',(-42.1085651452789,38.6478299447355,39.4375757897208));
#31061=CARTESIAN_POINT('Ctrl Pts',(-42.1275537969615,38.6929917463449,39.4549980164863));
#31062=CARTESIAN_POINT('Ctrl Pts',(-42.1460535633518,38.7385436808176,39.4719040365861));
#31063=CARTESIAN_POINT('Ctrl Pts',(-42.1645533297421,38.7840956152903,39.4888100566859));
#31064=CARTESIAN_POINT('Ctrl Pts',(-42.1825642102562,38.8300376811886,39.5051998695865));
#31065=CARTESIAN_POINT('Ctrl Pts',(-42.2000774430502,38.8763475288439,39.521065502053));
#31066=CARTESIAN_POINT('Ctrl Pts',(-42.2175906758442,38.9226573764992,39.5369311345194));
#31067=CARTESIAN_POINT('Ctrl Pts',(-42.2346062603653,38.9693350044501,39.5522725860509));
#31068=CARTESIAN_POINT('Ctrl Pts',(-42.2511159189565,39.0163577051954,39.5670823934142));
#31069=CARTESIAN_POINT('Ctrl Pts',(-42.2676255775476,39.0633804059407,39.5818922007775));
#31070=CARTESIAN_POINT('Ctrl Pts',(-42.2836293096875,39.1107481779964,39.5961703635052));
#31071=CARTESIAN_POINT('Ctrl Pts',(-42.2991193299602,39.1584379781235,39.6099099356275));
#31072=CARTESIAN_POINT('Ctrl Pts',(-42.3146231168746,39.2061701622101,39.6236617186936));
#31073=CARTESIAN_POINT('Ctrl Pts',(-42.3296122779107,39.2542249455147,39.6368739529574));
#31074=CARTESIAN_POINT('Ctrl Pts',(-42.3440795080264,39.302578909153,39.6495401993338));
#31075=CARTESIAN_POINT('Ctrl Pts',(-41.2672744347863,37.3041013800735,38.6761124197842));
#31076=CARTESIAN_POINT('Ctrl Pts',(-41.2965635232959,37.3380978767079,38.7046002687137));
#31077=CARTESIAN_POINT('Ctrl Pts',(-41.3254874763212,37.3727451372724,38.7326869200393));
#31078=CARTESIAN_POINT('Ctrl Pts',(-41.3540316073419,37.4080255704625,38.7603581136382));
#31079=CARTESIAN_POINT('Ctrl Pts',(-41.3825757383625,37.4433060036527,38.7880293072371));
#31080=CARTESIAN_POINT('Ctrl Pts',(-41.4107400463986,37.4792196082576,38.8152850421596));
#31081=CARTESIAN_POINT('Ctrl Pts',(-41.4385102302705,37.5157481505658,38.8421114797774));
#31082=CARTESIAN_POINT('Ctrl Pts',(-41.4662804141424,37.552276692874,38.8689379173952));
#31083=CARTESIAN_POINT('Ctrl Pts',(-41.4936564728967,37.5894201716319,38.8953350567876));
#31084=CARTESIAN_POINT('Ctrl Pts',(-41.5206245051938,37.6271597292047,38.92128949485));
#31085=CARTESIAN_POINT('Ctrl Pts',(-41.5475925374909,37.6648992867775,38.9472439329125));
#31086=CARTESIAN_POINT('Ctrl Pts',(-41.5741525424049,37.7032349218701,38.9727556687541));
#31087=CARTESIAN_POINT('Ctrl Pts',(-41.60029103253,37.7421471720403,38.9978117483818));
#31088=CARTESIAN_POINT('Ctrl Pts',(-41.6264295226551,37.7810594222105,39.0228678280095));
#31089=CARTESIAN_POINT('Ctrl Pts',(-41.6521464970939,37.820548286123,39.0474682505631));
#31090=CARTESIAN_POINT('Ctrl Pts',(-41.6774288960495,37.8605937162565,39.071600524294));
#31091=CARTESIAN_POINT('Ctrl Pts',(-41.702711295005,37.90063914639,39.0957327980249));
#31092=CARTESIAN_POINT('Ctrl Pts',(-41.7275591176092,37.9412411413704,39.1193969221046));
#31093=CARTESIAN_POINT('Ctrl Pts',(-41.7519597449155,37.9823790889186,39.1425808796936));
#31094=CARTESIAN_POINT('Ctrl Pts',(-41.7763603722218,38.0235170364667,39.1657648372826));
#31095=CARTESIAN_POINT('Ctrl Pts',(-41.8003138033923,38.0651909351709,39.1884686275849));
#31096=CARTESIAN_POINT('Ctrl Pts',(-41.8238078731261,38.1073796288875,39.210680720854));
#31097=CARTESIAN_POINT('Ctrl Pts',(-41.8473019428599,38.1495683226041,39.2328928141231));
#31098=CARTESIAN_POINT('Ctrl Pts',(-41.8703366503502,38.1922718098854,39.2546132095963));
#31099=CARTESIAN_POINT('Ctrl Pts',(-41.8929002962776,38.2354684121674,39.2758308763104));
#31100=CARTESIAN_POINT('Ctrl Pts',(-41.9154639422049,38.2786650144493,39.2970485430246));
#31101=CARTESIAN_POINT('Ctrl Pts',(-41.9375565257944,38.3223547302496,39.3177634802512));
#31102=CARTESIAN_POINT('Ctrl Pts',(-41.9591668255718,38.3665153805573,39.3379651669958));
#31103=CARTESIAN_POINT('Ctrl Pts',(-41.9807771253491,38.4106760308652,39.3581668537404));
#31104=CARTESIAN_POINT('Ctrl Pts',(-42.001905140572,38.4553076141653,39.3778552893091));
#31105=CARTESIAN_POINT('Ctrl Pts',(-42.0225401389914,38.5003874734805,39.3970204733452));
#31106=CARTESIAN_POINT('Ctrl Pts',(-42.0431751374107,38.5454673327957,39.4161856573814));
#31107=CARTESIAN_POINT('Ctrl Pts',(-42.0633171183177,38.5909954665794,39.4348275892266));
#31108=CARTESIAN_POINT('Ctrl Pts',(-42.0829558495725,38.636948762853,39.4529367993031));
#31109=CARTESIAN_POINT('Ctrl Pts',(-42.1025945808273,38.6829020591267,39.4710460093795));
#31110=CARTESIAN_POINT('Ctrl Pts',(-42.1217300617553,38.7292805163137,39.4886224970651));
#31111=CARTESIAN_POINT('Ctrl Pts',(-42.1403525707042,38.7760605908604,39.5056573331652));
#31112=CARTESIAN_POINT('Ctrl Pts',(-42.1589750796531,38.8228406654072,39.5226921692653));
#31113=CARTESIAN_POINT('Ctrl Pts',(-42.1770846159829,38.8700223557087,39.5391853531945));
#31114=CARTESIAN_POINT('Ctrl Pts',(-42.1946719783898,38.9175817104993,39.5551285051979));
#31115=CARTESIAN_POINT('Ctrl Pts',(-42.2122593407967,38.9651410652898,39.5710716572012));
#31116=CARTESIAN_POINT('Ctrl Pts',(-42.2293245286761,39.0130780829377,39.5864647767308));
#31117=CARTESIAN_POINT('Ctrl Pts',(-42.2458588704062,39.0613684287422,39.6013000419716));
#31118=CARTESIAN_POINT('Ctrl Pts',(-42.2623932121364,39.1096587745465,39.6161353072125));
#31119=CARTESIAN_POINT('Ctrl Pts',(-42.2783967071489,39.1583024468505,39.6304127176547));
#31120=CARTESIAN_POINT('Ctrl Pts',(-42.2938612223017,39.2072747521832,39.6441250173583));
#31121=CARTESIAN_POINT('Ctrl Pts',(-42.3093394814288,39.2562905812924,39.6578495037676));
#31122=CARTESIAN_POINT('Ctrl Pts',(-42.3242778017089,39.3056356261468,39.6710078740436));
#31123=CARTESIAN_POINT('Ctrl Pts',(-42.3386685764868,39.3552847927467,39.6835934276506));
#31124=CARTESIAN_POINT('Ctrl Pts',(-41.2477503364942,37.30491207051,38.695196554612));
#31125=CARTESIAN_POINT('Ctrl Pts',(-41.2776316088372,37.3396307438627,38.7243168606012));
#31126=CARTESIAN_POINT('Ctrl Pts',(-41.3071320670255,37.3750281244084,38.7530187418362));
#31127=CARTESIAN_POINT('Ctrl Pts',(-41.3362360873192,37.4110854666086,38.7812869986631));
#31128=CARTESIAN_POINT('Ctrl Pts',(-41.3653401076128,37.4471428088089,38.8095552554899));
#31129=CARTESIAN_POINT('Ctrl Pts',(-41.3940476889249,37.4838601113176,38.8373898868531));
#31130=CARTESIAN_POINT('Ctrl Pts',(-41.4223436270301,37.5212179301777,38.8647761519648));
#31131=CARTESIAN_POINT('Ctrl Pts',(-41.4506395651352,37.5585757490378,38.8921624170764));
#31132=CARTESIAN_POINT('Ctrl Pts',(-41.4785238589767,37.5965740828547,38.919100314914));
#31133=CARTESIAN_POINT('Ctrl Pts',(-41.5059817399214,37.6351928098112,38.9455755791419));
#31134=CARTESIAN_POINT('Ctrl Pts',(-41.5334396208661,37.6738115367676,38.9720508433698));
#31135=CARTESIAN_POINT('Ctrl Pts',(-41.5604710878885,37.7130506554219,38.9980634729996));
#31136=CARTESIAN_POINT('Ctrl Pts',(-41.5870618235653,37.7528893873707,39.0235996912331));
#31137=CARTESIAN_POINT('Ctrl Pts',(-41.6136525592421,37.7927281193195,39.0491359094667));
#31138=CARTESIAN_POINT('Ctrl Pts',(-41.6398025625802,37.8331664630757,39.0741957153506));
#31139=CARTESIAN_POINT('Ctrl Pts',(-41.665497982507,37.8741830056177,39.0987658361924));
#31140=CARTESIAN_POINT('Ctrl Pts',(-41.6911934024338,37.9151995481598,39.1233359570343));
#31141=CARTESIAN_POINT('Ctrl Pts',(-41.7164342379895,37.9567942879567,39.1474163919165));
#31142=CARTESIAN_POINT('Ctrl Pts',(-41.7412071191007,37.9989452000071,39.1709943862882));
#31143=CARTESIAN_POINT('Ctrl Pts',(-41.7659800002119,38.0410961120575,39.1945723806599));
#31144=CARTESIAN_POINT('Ctrl Pts',(-41.790284925953,38.083803194786,39.2176479336384));
#31145=CARTESIAN_POINT('Ctrl Pts',(-41.8141090213905,38.1270438345005,39.2402088223063));
#31146=CARTESIAN_POINT('Ctrl Pts',(-41.8379331168278,38.1702844742152,39.2627697109742));
#31147=CARTESIAN_POINT('Ctrl Pts',(-41.8612763810714,38.2140586693022,39.284815934489));
#31148=CARTESIAN_POINT('Ctrl Pts',(-41.8841264479437,38.2583432412732,39.3063358144816));
#31149=CARTESIAN_POINT('Ctrl Pts',(-41.9069765148161,38.3026278132442,39.3278556944743));
#31150=CARTESIAN_POINT('Ctrl Pts',(-41.9293333834634,38.3474227604456,39.3488492301403));
#31151=CARTESIAN_POINT('Ctrl Pts',(-41.9511852095457,38.3927043641151,39.3693053000282));
#31152=CARTESIAN_POINT('Ctrl Pts',(-41.9730370356281,38.4379859677846,39.3897613699161));
#31153=CARTESIAN_POINT('Ctrl Pts',(-41.9943838183286,38.4837542262293,39.409679973259));
#31154=CARTESIAN_POINT('Ctrl Pts',(-42.015214247673,38.5299849054721,39.4290505572722));
#31155=CARTESIAN_POINT('Ctrl Pts',(-42.0360446770173,38.5762155847148,39.4484211412853));
#31156=CARTESIAN_POINT('Ctrl Pts',(-42.0563587522268,38.6229086830301,39.4672437052448));
#31157=CARTESIAN_POINT('Ctrl Pts',(-42.0761457096572,38.6700394768505,39.4855082762004));
#31158=CARTESIAN_POINT('Ctrl Pts',(-42.0959326670877,38.7171702706709,39.503772847156));
#31159=CARTESIAN_POINT('Ctrl Pts',(-42.1151925059993,38.7647387582413,39.521479424428));
#31160=CARTESIAN_POINT('Ctrl Pts',(-42.1339150204658,38.8127197525332,39.5386186254455));
#31161=CARTESIAN_POINT('Ctrl Pts',(-42.1526375349323,38.8607007468251,39.555757826463));
#31162=CARTESIAN_POINT('Ctrl Pts',(-42.1708227242539,38.9090942460473,39.572329650585));
#31163=CARTESIAN_POINT('Ctrl Pts',(-42.1884609510199,38.9578746263604,39.5883253155651));
#31164=CARTESIAN_POINT('Ctrl Pts',(-42.2060991777859,39.0066550066736,39.6043209805452));
#31165=CARTESIAN_POINT('Ctrl Pts',(-42.2231904413368,39.0558222662528,39.6197404857819));
#31166=CARTESIAN_POINT('Ctrl Pts',(-42.2397256829768,39.1053503715122,39.6345756586278));
#31167=CARTESIAN_POINT('Ctrl Pts',(-42.2562609246168,39.1548784767715,39.6494108314737));
#31168=CARTESIAN_POINT('Ctrl Pts',(-42.2722401437274,39.2047674258621,39.6636616713738));
#31169=CARTESIAN_POINT('Ctrl Pts',(-42.2876548699138,39.254990802981,39.6773206239347));
#31170=CARTESIAN_POINT('Ctrl Pts',(-42.3030832958249,39.3052588157572,39.6909917157894));
#31171=CARTESIAN_POINT('Ctrl Pts',(-42.3179462244095,39.3558618493942,39.7040698672579));
#31172=CARTESIAN_POINT('Ctrl Pts',(-42.3322357615307,39.4067730623479,39.716548131702));
#31173=CARTESIAN_POINT('Ctrl Pts',(-41.2282110280907,37.3057050044843,38.7142657303796));
#31174=CARTESIAN_POINT('Ctrl Pts',(-41.2586695369814,37.3411274416385,38.7440022303608));
#31175=CARTESIAN_POINT('Ctrl Pts',(-41.2887314977015,37.3772566278719,38.7733030176263));
#31176=CARTESIAN_POINT('Ctrl Pts',(-41.3183803184579,37.4140726227688,38.8021519204898));
#31177=CARTESIAN_POINT('Ctrl Pts',(-41.3480291392142,37.4508886176657,38.8310008233533));
#31178=CARTESIAN_POINT('Ctrl Pts',(-41.3772648188021,37.4883914197305,38.8593978406427));
#31179=CARTESIAN_POINT('Ctrl Pts',(-41.4060712214694,37.5265603304216,38.88732729948));
#31180=CARTESIAN_POINT('Ctrl Pts',(-41.4348776241367,37.5647292411127,38.9152567583173));
#31181=CARTESIAN_POINT('Ctrl Pts',(-41.463254748713,37.6035642588794,38.9427186575678));
#31182=CARTESIAN_POINT('Ctrl Pts',(-41.4911869332995,37.6430439499042,38.9696978404639));
#31183=CARTESIAN_POINT('Ctrl Pts',(-41.519119117886,37.6825236409288,38.9966770233599));
#31184=CARTESIAN_POINT('Ctrl Pts',(-41.5466063613479,37.7226480036075,39.0231734888054));
#31185=CARTESIAN_POINT('Ctrl Pts',(-41.5736334929296,37.7633948925073,39.0491726128747));
#31186=CARTESIAN_POINT('Ctrl Pts',(-41.6006606245112,37.8041417814072,39.075171736944));
#31187=CARTESIAN_POINT('Ctrl Pts',(-41.6272276431146,37.8455111948727,39.1006735185808));
#31188=CARTESIAN_POINT('Ctrl Pts',(-41.6533198858744,37.8874803003029,39.1256638828453));
#31189=CARTESIAN_POINT('Ctrl Pts',(-41.6794121286342,37.9294494057331,39.1506542471098));
#31190=CARTESIAN_POINT('Ctrl Pts',(-41.7050295944903,37.9720182014228,39.1751331929866));
#31191=CARTESIAN_POINT('Ctrl Pts',(-41.7301581446544,38.0151631928082,39.1990872100594));
#31192=CARTESIAN_POINT('Ctrl Pts',(-41.7552866948186,38.0583081841935,39.2230412271322));
#31193=CARTESIAN_POINT('Ctrl Pts',(-41.7799263282698,38.1020293695198,39.2464703144257));
#31194=CARTESIAN_POINT('Ctrl Pts',(-41.8040634459051,38.1463026181998,39.269361540965));
#31195=CARTESIAN_POINT('Ctrl Pts',(-41.8282005635404,38.1905758668799,39.2922527675044));
#31196=CARTESIAN_POINT('Ctrl Pts',(-41.8518351643792,38.2354011771156,39.31460613236));
#31197=CARTESIAN_POINT('Ctrl Pts',(-41.8749542040155,38.2807538089233,39.3364092982614));
#31198=CARTESIAN_POINT('Ctrl Pts',(-41.8980732436519,38.326106440731,39.3582124641628));
#31199=CARTESIAN_POINT('Ctrl Pts',(-41.9206767211466,38.3719863922678,39.3794654302238));
#31200=CARTESIAN_POINT('Ctrl Pts',(-41.9427521611915,38.4183683414821,39.4001564665152));
#31201=CARTESIAN_POINT('Ctrl Pts',(-41.9648276012364,38.4647502906964,39.4208475028065));
#31202=CARTESIAN_POINT('Ctrl Pts',(-41.9863750029347,38.5116342357014,39.4409766084852));
#31203=CARTESIAN_POINT('Ctrl Pts',(-42.0073824738472,38.5589943003163,39.460532673898));
#31204=CARTESIAN_POINT('Ctrl Pts',(-42.0283899447598,38.6063543649314,39.4800887393107));
#31205=CARTESIAN_POINT('Ctrl Pts',(-42.0488574840331,38.6541905472324,39.499071763663));
#31206=CARTESIAN_POINT('Ctrl Pts',(-42.0687737952257,38.70247644548,39.5174712698466));
#31207=CARTESIAN_POINT('Ctrl Pts',(-42.0886901064184,38.7507623437277,39.5358707760302));
#31208=CARTESIAN_POINT('Ctrl Pts',(-42.108055188721,38.799497955964,39.5536867633005));
#31209=CARTESIAN_POINT('Ctrl Pts',(-42.1268583541603,38.8486563840293,39.5709093986544));
#31210=CARTESIAN_POINT('Ctrl Pts',(-42.1456615195996,38.8978148120945,39.5881320340084));
#31211=CARTESIAN_POINT('Ctrl Pts',(-42.1639027674119,38.947396053991,39.6047613167461));
#31212=CARTESIAN_POINT('Ctrl Pts',(-42.1815720298895,38.9973727448544,39.6207880688421));
#31213=CARTESIAN_POINT('Ctrl Pts',(-42.199241292367,39.0473494357178,39.6368148209381));
#31214=CARTESIAN_POINT('Ctrl Pts',(-42.2163385687924,39.0977215735138,39.6522390417384));
#31215=CARTESIAN_POINT('Ctrl Pts',(-42.232854422839,39.1484613568588,39.667052218309));
#31216=CARTESIAN_POINT('Ctrl Pts',(-42.2493702768857,39.1992011402039,39.6818653948796));
#31217=CARTESIAN_POINT('Ctrl Pts',(-42.2653047078826,39.2503085670367,39.6960675266187));
#31218=CARTESIAN_POINT('Ctrl Pts',(-42.2806489213008,39.301755430153,39.7096507750877));
#31219=CARTESIAN_POINT('Ctrl Pts',(-42.2960067717759,39.3532480162909,39.723246095569));
#31220=CARTESIAN_POINT('Ctrl Pts',(-42.3107733544778,39.4050806402349,39.7362214316859));
#31221=CARTESIAN_POINT('Ctrl Pts',(-42.3249405046544,39.4572246438149,39.7485696090469));
#31222=CARTESIAN_POINT('Ctrl Pts',(-41.2086717196872,37.3064979384586,38.7333349061473));
#31223=CARTESIAN_POINT('Ctrl Pts',(-41.2397074651256,37.3426241394144,38.7636876001203));
#31224=CARTESIAN_POINT('Ctrl Pts',(-41.2703309283775,37.3794851313355,38.7935872934165));
#31225=CARTESIAN_POINT('Ctrl Pts',(-41.3005245495965,37.417059778929,38.8230168423166));
#31226=CARTESIAN_POINT('Ctrl Pts',(-41.3307181708155,37.4546344265226,38.8524463912167));
#31227=CARTESIAN_POINT('Ctrl Pts',(-41.3604819486794,37.4929227281434,38.8814057944323));
#31228=CARTESIAN_POINT('Ctrl Pts',(-41.3897988159087,37.5319027306655,38.9098784469952));
#31229=CARTESIAN_POINT('Ctrl Pts',(-41.4191156831381,37.5708827331875,38.9383510995581));
#31230=CARTESIAN_POINT('Ctrl Pts',(-41.4479856384492,37.6105544349041,38.9663370002217));
#31231=CARTESIAN_POINT('Ctrl Pts',(-41.4763921266775,37.6508950899971,38.9938201017858));
#31232=CARTESIAN_POINT('Ctrl Pts',(-41.5047986149058,37.69123574509,39.02130320335));
#31233=CARTESIAN_POINT('Ctrl Pts',(-41.5327416348073,37.7322453517931,39.0482835046113));
#31234=CARTESIAN_POINT('Ctrl Pts',(-41.5602051622938,37.7739003976439,39.0747455345162));
#31235=CARTESIAN_POINT('Ctrl Pts',(-41.5876686897804,37.8155554434947,39.1012075644212));
#31236=CARTESIAN_POINT('Ctrl Pts',(-41.614652723649,37.8578559266697,39.127151321811));
#31237=CARTESIAN_POINT('Ctrl Pts',(-41.6411417892418,37.900777594988,39.1525619294982));
#31238=CARTESIAN_POINT('Ctrl Pts',(-41.6676308548345,37.9436992633064,39.1779725371852));
#31239=CARTESIAN_POINT('Ctrl Pts',(-41.6936249509911,37.987242114889,39.2028499940568));
#31240=CARTESIAN_POINT('Ctrl Pts',(-41.7191091702082,38.0313811856093,39.2271800338306));
#31241=CARTESIAN_POINT('Ctrl Pts',(-41.7445933894253,38.0755202563297,39.2515100736044));
#31242=CARTESIAN_POINT('Ctrl Pts',(-41.7695677305865,38.1202555442535,39.2752926952129));
#31243=CARTESIAN_POINT('Ctrl Pts',(-41.7940178704198,38.165561401899,39.2985142596238));
#31244=CARTESIAN_POINT('Ctrl Pts',(-41.818468010253,38.2108672595447,39.3217358240347));
#31245=CARTESIAN_POINT('Ctrl Pts',(-41.842393947687,38.256743684929,39.344396330231));
#31246=CARTESIAN_POINT('Ctrl Pts',(-41.8657819600873,38.3031643765735,39.3664827820411));
#31247=CARTESIAN_POINT('Ctrl Pts',(-41.8891699724877,38.349585068218,39.3885692338512));
#31248=CARTESIAN_POINT('Ctrl Pts',(-41.9120200588297,38.39655002409,39.4100816303073));
#31249=CARTESIAN_POINT('Ctrl Pts',(-41.9343191128372,38.4440323188491,39.4310076330021));
#31250=CARTESIAN_POINT('Ctrl Pts',(-41.9566181668448,38.4915146136082,39.4519336356969));
#31251=CARTESIAN_POINT('Ctrl Pts',(-41.9783661875408,38.5395142451733,39.4722732437114));
#31252=CARTESIAN_POINT('Ctrl Pts',(-41.9995507000215,38.5880036951607,39.4920147905237));
#31253=CARTESIAN_POINT('Ctrl Pts',(-42.0207352125022,38.6364931451479,39.511756337336));
#31254=CARTESIAN_POINT('Ctrl Pts',(-42.0413562158394,38.6854724114346,39.5308998220812));
#31255=CARTESIAN_POINT('Ctrl Pts',(-42.0614018807942,38.7349134141096,39.5494342634928));
#31256=CARTESIAN_POINT('Ctrl Pts',(-42.081447545749,38.7843544167844,39.5679687049045));
#31257=CARTESIAN_POINT('Ctrl Pts',(-42.1009178714426,38.8342571536868,39.585894102173));
#31258=CARTESIAN_POINT('Ctrl Pts',(-42.1198016878547,38.8845930155253,39.6032001718634));
#31259=CARTESIAN_POINT('Ctrl Pts',(-42.1386855042668,38.9349288773639,39.6205062415537));
#31260=CARTESIAN_POINT('Ctrl Pts',(-42.1569828105698,38.9856978619347,39.6371929829072));
#31261=CARTESIAN_POINT('Ctrl Pts',(-42.174683108759,39.0368708633483,39.6532508221192));
#31262=CARTESIAN_POINT('Ctrl Pts',(-42.1923834069483,39.088043864762,39.6693086613312));
#31263=CARTESIAN_POINT('Ctrl Pts',(-42.2094866962481,39.1396208807746,39.6847375976949));
#31264=CARTESIAN_POINT('Ctrl Pts',(-42.2259831627013,39.1915723422055,39.6995287779901));
#31265=CARTESIAN_POINT('Ctrl Pts',(-42.2424796291546,39.2435238036363,39.7143199582854));
#31266=CARTESIAN_POINT('Ctrl Pts',(-42.2583692720378,39.2958497082112,39.7284733818636));
#31267=CARTESIAN_POINT('Ctrl Pts',(-42.2736429726878,39.348520057325,39.7419809262407));
#31268=CARTESIAN_POINT('Ctrl Pts',(-42.2889302477269,39.4012372168246,39.7555004753485));
#31269=CARTESIAN_POINT('Ctrl Pts',(-42.3036004845462,39.4542994310756,39.768372996114));
#31270=CARTESIAN_POINT('Ctrl Pts',(-42.3176452477781,39.5076762252817,39.7805910863918));
#31271=CARTESIAN_POINT('Ctrl Pts',(-41.1891171828089,37.3072730945328,38.7523891047943));
#31272=CARTESIAN_POINT('Ctrl Pts',(-41.2207151987186,37.3440846246979,38.7833417116339));
#31273=CARTESIAN_POINT('Ctrl Pts',(-41.2518851430282,37.3816590864308,38.8138239689665));
#31274=CARTESIAN_POINT('Ctrl Pts',(-41.2826084569984,37.4199741089117,38.8438177285332));
#31275=CARTESIAN_POINT('Ctrl Pts',(-41.3133317709687,37.4582891313924,38.8738114880999));
#31276=CARTESIAN_POINT('Ctrl Pts',(-41.343608453149,37.4973447128122,38.9033167484847));
#31277=CARTESIAN_POINT('Ctrl Pts',(-41.3734204762462,37.5371176011145,38.9323159426931));
#31278=CARTESIAN_POINT('Ctrl Pts',(-41.4032324993435,37.5768904894166,38.9613151369015));
#31279=CARTESIAN_POINT('Ctrl Pts',(-41.43257986195,37.6173806827237,38.9898082635645));
#31280=CARTESIAN_POINT('Ctrl Pts',(-41.4614450896576,37.658564075392,39.0177783578423));
#31281=CARTESIAN_POINT('Ctrl Pts',(-41.4903103173653,37.6997474680603,39.0457484521201));
#31282=CARTESIAN_POINT('Ctrl Pts',(-41.5186934088111,37.7416240581456,39.0731955126921));
#31283=CARTESIAN_POINT('Ctrl Pts',(-41.5465774632538,37.7841689150809,39.1001031970481));
#31284=CARTESIAN_POINT('Ctrl Pts',(-41.5744615176964,37.8267137720161,39.1270108814041));
#31285=CARTESIAN_POINT('Ctrl Pts',(-41.6018465338191,37.869926893793,39.1533791882735));
#31286=CARTESIAN_POINT('Ctrl Pts',(-41.6287162046479,37.9137825545649,39.179192416911));
#31287=CARTESIAN_POINT('Ctrl Pts',(-41.6555858754767,37.9576382153368,39.2050056455483));
#31288=CARTESIAN_POINT('Ctrl Pts',(-41.6819401997425,38.0021364130336,39.2302637947347));
#31289=CARTESIAN_POINT('Ctrl Pts',(-41.7077634836333,38.0472506571184,39.2549518241621));
#31290=CARTESIAN_POINT('Ctrl Pts',(-41.7335867675241,38.0923649012032,39.2796398535895));
#31291=CARTESIAN_POINT('Ctrl Pts',(-41.7588790098202,38.1380951895466,39.3037577620919));
#31292=CARTESIAN_POINT('Ctrl Pts',(-41.783625148538,38.1844142984193,39.3272911876869));
#31293=CARTESIAN_POINT('Ctrl Pts',(-41.8083712872557,38.2307334072919,39.3508246132818));
#31294=CARTESIAN_POINT('Ctrl Pts',(-41.8325713212261,38.2776413345075,39.373773554858));
#31295=CARTESIAN_POINT('Ctrl Pts',(-41.8562108382094,38.325110155514,39.3961243458403));
#31296=CARTESIAN_POINT('Ctrl Pts',(-41.8798503551926,38.3725789765204,39.4184751368226));
#31297=CARTESIAN_POINT('Ctrl Pts',(-41.902929354072,38.4206086890771,39.4402277761556));
#31298=CARTESIAN_POINT('Ctrl Pts',(-41.9254340894953,38.469170701011,39.4613693089278));
#31299=CARTESIAN_POINT('Ctrl Pts',(-41.9479388249185,38.5177327129449,39.4825108417001));
#31300=CARTESIAN_POINT('Ctrl Pts',(-41.9698692958223,38.5668270219641,39.5030412669129));
#31301=CARTESIAN_POINT('Ctrl Pts',(-41.9912124400932,38.6164244022708,39.5229483567292));
#31302=CARTESIAN_POINT('Ctrl Pts',(-42.0125555843642,38.6660217825775,39.5428554465454));
#31303=CARTESIAN_POINT('Ctrl Pts',(-42.0333114009938,38.7161222318307,39.5621392000245));
#31304=CARTESIAN_POINT('Ctrl Pts',(-42.0534675266471,38.7666959253572,39.5807881309497));
#31305=CARTESIAN_POINT('Ctrl Pts',(-42.0736236523004,38.8172696188837,39.599437061875));
#31306=CARTESIAN_POINT('Ctrl Pts',(-42.0931800860248,38.8683165542964,39.6174511693651));
#31307=CARTESIAN_POINT('Ctrl Pts',(-42.1121251779732,38.9198063435073,39.6348197224895));
#31308=CARTESIAN_POINT('Ctrl Pts',(-42.1310702699216,38.9712961327183,39.6521882756139));
#31309=CARTESIAN_POINT('Ctrl Pts',(-42.1494040191985,39.0232287732974,39.6689112735516));
#31310=CARTESIAN_POINT('Ctrl Pts',(-42.1671155033061,39.0755733498729,39.6849787534261));
#31311=CARTESIAN_POINT('Ctrl Pts',(-42.1848269874139,39.1279179264482,39.7010462333006));
#31312=CARTESIAN_POINT('Ctrl Pts',(-42.201916205515,39.1806744365496,39.7164581943523));
#31313=CARTESIAN_POINT('Ctrl Pts',(-42.2183729754589,39.2338114742793,39.7312054536145));
#31314=CARTESIAN_POINT('Ctrl Pts',(-42.2348297454029,39.286948512009,39.7459527128766));
#31315=CARTESIAN_POINT('Ctrl Pts',(-42.2506540664114,39.3404660748592,39.7600352696516));
#31316=CARTESIAN_POINT('Ctrl Pts',(-42.2658365087988,39.3943323037477,39.7734447318117));
#31317=CARTESIAN_POINT('Ctrl Pts',(-42.2810324444704,39.4482464058514,39.7868661115327));
#31318=CARTESIAN_POINT('Ctrl Pts',(-42.2955853593645,39.5025097914708,39.7996131990557));
#31319=CARTESIAN_POINT('Ctrl Pts',(-42.3094865643585,39.557090100092,39.8116783828227));
#31320=CARTESIAN_POINT('Ctrl Pts',(-41.1695498758672,37.3080333426854,38.7714307441548));
#31321=CARTESIAN_POINT('Ctrl Pts',(-41.2016975079946,37.3455145501839,38.8029693924383));
#31322=CARTESIAN_POINT('Ctrl Pts',(-41.2334012260665,37.3837869243692,38.8340202841051));
#31323=CARTESIAN_POINT('Ctrl Pts',(-41.2646414427327,37.422826819611,38.8645642351373));
#31324=CARTESIAN_POINT('Ctrl Pts',(-41.2958816593989,37.4618667148527,38.8951081861696));
#31325=CARTESIAN_POINT('Ctrl Pts',(-41.3266583730689,37.5016741291636,38.9251451950123));
#31326=CARTESIAN_POINT('Ctrl Pts',(-41.3569525691191,37.542224468527,38.95465670405));
#31327=CARTESIAN_POINT('Ctrl Pts',(-41.3872467651694,37.5827748078904,38.9841682130878));
#31328=CARTESIAN_POINT('Ctrl Pts',(-41.4170584420575,37.6240680702419,39.0131542208182));
#31329=CARTESIAN_POINT('Ctrl Pts',(-41.4463691813837,37.6660787435711,39.0415968189604));
#31330=CARTESIAN_POINT('Ctrl Pts',(-41.4756799207099,37.7080894169003,39.0700394171026));
#31331=CARTESIAN_POINT('Ctrl Pts',(-41.504489720982,37.7508174990684,39.0979386042086));
#31332=CARTESIAN_POINT('Ctrl Pts',(-41.5327807827847,37.7942365915972,39.1252771434628));
#31333=CARTESIAN_POINT('Ctrl Pts',(-41.5610718445874,37.837655684126,39.1526156827169));
#31334=CARTESIAN_POINT('Ctrl Pts',(-41.5888441664803,37.8817657848052,39.1793935727274));
#31335=CARTESIAN_POINT('Ctrl Pts',(-41.6160805900283,37.9265396413109,39.2055942694438));
#31336=CARTESIAN_POINT('Ctrl Pts',(-41.6433170135763,37.9713134978166,39.2317949661601));
#31337=CARTESIAN_POINT('Ctrl Pts',(-41.6700175373926,38.0167511078695,39.2574184682485));
#31338=CARTESIAN_POINT('Ctrl Pts',(-41.6961656652258,38.0628243989772,39.2824489448684));
#31339=CARTESIAN_POINT('Ctrl Pts',(-41.7223137930589,38.1088976900851,39.3074794214883));
#31340=CARTESIAN_POINT('Ctrl Pts',(-41.7479095235777,38.1556066599023,39.3319168713652));
#31341=CARTESIAN_POINT('Ctrl Pts',(-41.7729370430994,38.2029224504587,39.3557461964314));
#31342=CARTESIAN_POINT('Ctrl Pts',(-41.7979645626212,38.2502382410151,39.3795755214976));
#31343=CARTESIAN_POINT('Ctrl Pts',(-41.8224238698717,38.2981608499019,39.40279672054));
#31344=CARTESIAN_POINT('Ctrl Pts',(-41.8462998532791,38.3466606693325,39.4253954469206));
#31345=CARTESIAN_POINT('Ctrl Pts',(-41.8701758366865,38.3951604887631,39.4479941733013));
#31346=CARTESIAN_POINT('Ctrl Pts',(-41.8934684950353,38.4442375162683,39.4699704258699));
#31347=CARTESIAN_POINT('Ctrl Pts',(-41.9161634375384,38.4938614308328,39.4913106271477));
#31348=CARTESIAN_POINT('Ctrl Pts',(-41.9388583800415,38.5434853453973,39.5126508284255));
#31349=CARTESIAN_POINT('Ctrl Pts',(-41.9609556055435,38.5936561444947,39.5333549773262));
#31350=CARTESIAN_POINT('Ctrl Pts',(-41.9824414618257,38.6443428313502,39.5534102823086));
#31351=CARTESIAN_POINT('Ctrl Pts',(-42.003927318108,38.6950295182057,39.5734655872909));
#31352=CARTESIAN_POINT('Ctrl Pts',(-42.0248018040765,38.7462320902388,39.592872047334));
#31353=CARTESIAN_POINT('Ctrl Pts',(-42.0450520229517,38.7979189132196,39.6116176726411));
#31354=CARTESIAN_POINT('Ctrl Pts',(-42.065302241827,38.8496057362004,39.6303632979483));
#31355=CARTESIAN_POINT('Ctrl Pts',(-42.0849281925779,38.9017768074975,39.6484480875653));
#31356=CARTESIAN_POINT('Ctrl Pts',(-42.1039177498013,38.9543998945179,39.6658608682567));
#31357=CARTESIAN_POINT('Ctrl Pts',(-42.1229073070247,39.0070229815383,39.683273648948));
#31358=CARTESIAN_POINT('Ctrl Pts',(-42.1412604697537,39.0600980816029,39.7000144198273));
#31359=CARTESIAN_POINT('Ctrl Pts',(-42.1589658989453,39.1135924035872,39.7160728380273));
#31360=CARTESIAN_POINT('Ctrl Pts',(-42.1766713281368,39.1670867255715,39.7321312562274));
#31361=CARTESIAN_POINT('Ctrl Pts',(-42.1937290228895,39.2210002667519,39.7475073209307));
#31362=CARTESIAN_POINT('Ctrl Pts',(-42.2101284445329,39.2752997179941,39.7621915324199));
#31363=CARTESIAN_POINT('Ctrl Pts',(-42.2265278661762,39.3295991692364,39.776875743909));
#31364=CARTESIAN_POINT('Ctrl Pts',(-42.2422690138752,39.384284527776,39.7908681014365));
#31365=CARTESIAN_POINT('Ctrl Pts',(-42.2573421623552,39.4393220076303,39.8041599601737));
#31366=CARTESIAN_POINT('Ctrl Pts',(-42.272428706985,39.4944084016404,39.8174636319526));
#31367=CARTESIAN_POINT('Ctrl Pts',(-42.2868460637406,39.5498475403269,39.8300655585839));
#31368=CARTESIAN_POINT('Ctrl Pts',(-42.3005853090107,39.605605111288,39.8419579400509));
#31369=CARTESIAN_POINT('Ctrl Pts',(-41.1499825689254,37.308793590838,38.7904723835153));
#31370=CARTESIAN_POINT('Ctrl Pts',(-41.1826798172707,37.3469444756699,38.8225970732428));
#31371=CARTESIAN_POINT('Ctrl Pts',(-41.2149173091049,37.3859147623074,38.8542165992436));
#31372=CARTESIAN_POINT('Ctrl Pts',(-41.2466744284671,37.4256795303103,38.8853107417414));
#31373=CARTESIAN_POINT('Ctrl Pts',(-41.2784315478292,37.4654442983132,38.9164048842392));
#31374=CARTESIAN_POINT('Ctrl Pts',(-41.3097082929889,37.506003545515,38.9469736415399));
#31375=CARTESIAN_POINT('Ctrl Pts',(-41.3404846619921,37.5473313359395,38.976997465407));
#31376=CARTESIAN_POINT('Ctrl Pts',(-41.3712610309953,37.5886591263641,39.0070212892741));
#31377=CARTESIAN_POINT('Ctrl Pts',(-41.401537022165,37.6307554577601,39.0365001780718));
#31378=CARTESIAN_POINT('Ctrl Pts',(-41.4312932731097,37.6735934117502,39.0654152800785));
#31379=CARTESIAN_POINT('Ctrl Pts',(-41.4610495240545,37.7164313657403,39.0943303820851));
#31380=CARTESIAN_POINT('Ctrl Pts',(-41.490286033153,37.7600109399911,39.1226816957252));
#31381=CARTESIAN_POINT('Ctrl Pts',(-41.5189841023157,37.8043042681135,39.1504510898775));
#31382=CARTESIAN_POINT('Ctrl Pts',(-41.5476821714784,37.8485975962359,39.1782204840298));
#31383=CARTESIAN_POINT('Ctrl Pts',(-41.5758417991416,37.8936046758173,39.2054079571812));
#31384=CARTESIAN_POINT('Ctrl Pts',(-41.6034449754087,37.9392967280569,39.2319961219765));
#31385=CARTESIAN_POINT('Ctrl Pts',(-41.6310481516758,37.9849887802964,39.2585842867719));
#31386=CARTESIAN_POINT('Ctrl Pts',(-41.6580948750427,38.0313658027053,39.2845731417624));
#31387=CARTESIAN_POINT('Ctrl Pts',(-41.6845678468182,38.0783981408362,39.3099460655747));
#31388=CARTESIAN_POINT('Ctrl Pts',(-41.7110408185938,38.125430478967,39.335318989387));
#31389=CARTESIAN_POINT('Ctrl Pts',(-41.7369400373351,38.1731181302579,39.3600759806385));
#31390=CARTESIAN_POINT('Ctrl Pts',(-41.7622489376609,38.2214306024981,39.384201205176));
#31391=CARTESIAN_POINT('Ctrl Pts',(-41.7875578379866,38.2697430747382,39.4083264297134));
#31392=CARTESIAN_POINT('Ctrl Pts',(-41.8122764185173,38.3186803652963,39.4318198862219));
#31393=CARTESIAN_POINT('Ctrl Pts',(-41.8363888683489,38.368211183151,39.4546665480009));
#31394=CARTESIAN_POINT('Ctrl Pts',(-41.8605013181804,38.4177420010058,39.4775132097799));
#31395=CARTESIAN_POINT('Ctrl Pts',(-41.8840076359986,38.4678663434596,39.4997130755842));
#31396=CARTESIAN_POINT('Ctrl Pts',(-41.9068927855816,38.5185521606546,39.5212519453676));
#31397=CARTESIAN_POINT('Ctrl Pts',(-41.9297779351646,38.5692379778496,39.542790815151));
#31398=CARTESIAN_POINT('Ctrl Pts',(-41.9520419152648,38.6204852670253,39.5636686877395));
#31399=CARTESIAN_POINT('Ctrl Pts',(-41.9736704835583,38.6722612604296,39.583872207888));
#31400=CARTESIAN_POINT('Ctrl Pts',(-41.9952990518517,38.7240372538339,39.6040757280365));
#31401=CARTESIAN_POINT('Ctrl Pts',(-42.0162922071592,38.7763419486468,39.6236048946434));
#31402=CARTESIAN_POINT('Ctrl Pts',(-42.0366365192564,38.829141901082,39.6424472143325));
#31403=CARTESIAN_POINT('Ctrl Pts',(-42.0569808313535,38.8819418535171,39.6612895340217));
#31404=CARTESIAN_POINT('Ctrl Pts',(-42.0766762991311,38.9352370606986,39.6794450057655));
#31405=CARTESIAN_POINT('Ctrl Pts',(-42.0957103216294,38.9889934455284,39.6969020140239));
#31406=CARTESIAN_POINT('Ctrl Pts',(-42.1147443441278,39.0427498303582,39.7143590222822));
#31407=CARTESIAN_POINT('Ctrl Pts',(-42.1331169203089,39.0969673899085,39.7311175661029));
#31408=CARTESIAN_POINT('Ctrl Pts',(-42.1508162945843,39.1516114573015,39.7471669226285));
#31409=CARTESIAN_POINT('Ctrl Pts',(-42.1685156688598,39.2062555246946,39.7632162791541));
#31410=CARTESIAN_POINT('Ctrl Pts',(-42.185541840264,39.2613260969543,39.778556447509));
#31411=CARTESIAN_POINT('Ctrl Pts',(-42.2018839136068,39.3167879617091,39.7931776112253));
#31412=CARTESIAN_POINT('Ctrl Pts',(-42.2182259869495,39.3722498264638,39.8077987749415));
#31413=CARTESIAN_POINT('Ctrl Pts',(-42.2338839613391,39.4281029806927,39.8217009332214));
#31414=CARTESIAN_POINT('Ctrl Pts',(-42.2488478159115,39.4843117115128,39.8348751885357));
#31415=CARTESIAN_POINT('Ctrl Pts',(-42.2638249694997,39.5405703974295,39.8480611523726));
#31416=CARTESIAN_POINT('Ctrl Pts',(-42.2781067681167,39.5971852891831,39.8605179181121));
#31417=CARTESIAN_POINT('Ctrl Pts',(-42.2916840536628,39.654120122484,39.872237497279));
#31418=CARTESIAN_POINT('Ctrl Pts',(-41.1304024802123,37.3095389174009,38.8095014520746));
#31419=CARTESIAN_POINT('Ctrl Pts',(-41.1636366786685,37.3483438138742,38.8421983002006));
#31420=CARTESIAN_POINT('Ctrl Pts',(-41.1963952250877,37.3879964418396,38.8743725191787));
#31421=CARTESIAN_POINT('Ctrl Pts',(-41.2286564451757,37.4284705667593,38.9060028222506));
#31422=CARTESIAN_POINT('Ctrl Pts',(-41.2609176652637,37.4689446916788,38.9376331253226));
#31423=CARTESIAN_POINT('Ctrl Pts',(-41.292681557139,37.5102403111923,38.968719510644));
#31424=CARTESIAN_POINT('Ctrl Pts',(-41.3239271041963,37.5523301043298,38.9992414107585));
#31425=CARTESIAN_POINT('Ctrl Pts',(-41.3551726512535,37.5944198974674,39.0297633108729));
#31426=CARTESIAN_POINT('Ctrl Pts',(-41.3858998516704,37.6373038617746,39.0597207240003));
#31427=CARTESIAN_POINT('Ctrl Pts',(-41.416088374312,37.6809536259616,39.0890938291726));
#31428=CARTESIAN_POINT('Ctrl Pts',(-41.4462768969536,37.7246033901487,39.1184669343448));
#31429=CARTESIAN_POINT('Ctrl Pts',(-41.4759267400592,37.7690189516703,39.1472557298488));
#31430=CARTESIAN_POINT('Ctrl Pts',(-41.5050182848403,37.8141709264161,39.1754411674048));
#31431=CARTESIAN_POINT('Ctrl Pts',(-41.5341098296213,37.859322901162,39.2036266049609));
#31432=CARTESIAN_POINT('Ctrl Pts',(-41.5626430743809,37.9052112864981,39.2312086829236));
#31433=CARTESIAN_POINT('Ctrl Pts',(-41.5905991386123,37.9518057243334,39.2581691508848));
#31434=CARTESIAN_POINT('Ctrl Pts',(-41.6185552028437,37.9984001621687,39.285129618846));
#31435=CARTESIAN_POINT('Ctrl Pts',(-41.6459340849161,38.0457006497853,39.3114684752316));
#31436=CARTESIAN_POINT('Ctrl Pts',(-41.6727176675642,38.093675895231,39.337168291625));
#31437=CARTESIAN_POINT('Ctrl Pts',(-41.6995012502123,38.1416511406767,39.3628681080184));
#31438=CARTESIAN_POINT('Ctrl Pts',(-41.7256895318736,38.1903011411542,39.3879288829204));
#31439=CARTESIAN_POINT('Ctrl Pts',(-41.7512651824761,38.2395937122107,39.412334032949));
#31440=CARTESIAN_POINT('Ctrl Pts',(-41.7768408330786,38.2888862832671,39.4367391829776));
#31441=CARTESIAN_POINT('Ctrl Pts',(-41.8018038511301,38.3388214220307,39.460488706711));
#31442=CARTESIAN_POINT('Ctrl Pts',(-41.826137716664,38.3893660940808,39.4835668877218));
#31443=CARTESIAN_POINT('Ctrl Pts',(-41.8504715821979,38.4399107661308,39.5066450687327));
#31444=CARTESIAN_POINT('Ctrl Pts',(-41.8741762937945,38.4910649685201,39.5290519056741));
#31445=CARTESIAN_POINT('Ctrl Pts',(-41.8972361634342,38.5427948605339,39.5507725698646));
#31446=CARTESIAN_POINT('Ctrl Pts',(-41.9202960330739,38.5945247525476,39.5724932340552));
#31447=CARTESIAN_POINT('Ctrl Pts',(-41.942711059411,38.6468303311674,39.5935277242253));
#31448=CARTESIAN_POINT('Ctrl Pts',(-41.9644664071168,38.6996769940964,39.613862119033));
#31449=CARTESIAN_POINT('Ctrl Pts',(-41.9862217548225,38.7525236570254,39.6341965138405));
#31450=CARTESIAN_POINT('Ctrl Pts',(-42.0073174226271,38.8059114011827,39.653830812099));
#31451=CARTESIAN_POINT('Ctrl Pts',(-42.0277394475087,38.8598049084259,39.6727520182178));
#31452=CARTESIAN_POINT('Ctrl Pts',(-42.0481614723905,38.913698415669,39.6916732243367));
#31453=CARTESIAN_POINT('Ctrl Pts',(-42.0679098531573,38.9680976828559,39.7098813372114));
#31454=CARTESIAN_POINT('Ctrl Pts',(-42.0869715175592,39.0229667226778,39.7273643041888));
#31455=CARTESIAN_POINT('Ctrl Pts',(-42.1060331819613,39.0778357624995,39.7448472711662));
#31456=CARTESIAN_POINT('Ctrl Pts',(-42.1244081288856,39.1331745717573,39.7616050912256));
#31457=CARTESIAN_POINT('Ctrl Pts',(-42.1420841941426,39.1889465415369,39.7776266705897));
#31458=CARTESIAN_POINT('Ctrl Pts',(-42.1597602593996,39.2447185113166,39.7936482499537));
#31459=CARTESIAN_POINT('Ctrl Pts',(-42.176737441957,39.3009236383667,39.808933587687));
#31460=CARTESIAN_POINT('Ctrl Pts',(-42.1930045017737,39.3575247405534,39.8234725635622));
#31461=CARTESIAN_POINT('Ctrl Pts',(-42.2092715615904,39.4141258427401,39.8380115394373));
#31462=CARTESIAN_POINT('Ctrl Pts',(-42.2248284977163,39.4711229167633,39.851804152605));
#31463=CARTESIAN_POINT('Ctrl Pts',(-42.2396650091271,39.5284782564109,39.8648412697745));
#31464=CARTESIAN_POINT('Ctrl Pts',(-42.2545147063783,39.5858845701953,39.8778899735862));
#31465=CARTESIAN_POINT('Ctrl Pts',(-42.2686426969318,39.6436497833537,39.8901818371599));
#31466=CARTESIAN_POINT('Ctrl Pts',(-42.2820396074624,39.7017356135328,39.9017087045122));
#31467=CARTESIAN_POINT('Ctrl Pts',(-41.1108115454791,37.3102715821929,38.8285198536332));
#31468=CARTESIAN_POINT('Ctrl Pts',(-41.1445718264716,37.3497169975554,38.8617768648758));
#31469=CARTESIAN_POINT('Ctrl Pts',(-41.1778405082576,37.3900385661193,38.8944937248055));
#31470=CARTESIAN_POINT('Ctrl Pts',(-41.2105948293949,37.4312087010667,38.9266480495201));
#31471=CARTESIAN_POINT('Ctrl Pts',(-41.2433491505323,37.4723788360139,38.9588023742347));
#31472=CARTESIAN_POINT('Ctrl Pts',(-41.2755891089758,37.5143975347744,38.9903941617266));
#31473=CARTESIAN_POINT('Ctrl Pts',(-41.307292647105,37.5572360494041,39.0214017978346));
#31474=CARTESIAN_POINT('Ctrl Pts',(-41.3389961852342,37.6000745640338,39.0524094339426));
#31475=CARTESIAN_POINT('Ctrl Pts',(-41.3701633010698,37.6437328918582,39.0828329167309));
#31476=CARTESIAN_POINT('Ctrl Pts',(-41.4007726709981,37.6881811631482,39.1126514313572));
#31477=CARTESIAN_POINT('Ctrl Pts',(-41.4313820409265,37.7326294344381,39.1424699459836));
#31478=CARTESIAN_POINT('Ctrl Pts',(-41.4614336630366,37.7778676464184,39.1716834905866));
#31479=CARTESIAN_POINT('Ctrl Pts',(-41.4909069769024,37.8238648484503,39.2002720781278));
#31480=CARTESIAN_POINT('Ctrl Pts',(-41.5203802907683,37.8698620504821,39.2288606656691));
#31481=CARTESIAN_POINT('Ctrl Pts',(-41.5492752945498,37.9166182396925,39.2568242943625));
#31482=CARTESIAN_POINT('Ctrl Pts',(-41.5775722191449,37.9641014268898,39.2841438323276));
#31483=CARTESIAN_POINT('Ctrl Pts',(-41.6058691437401,38.0115846140871,39.3114633702927));
#31484=CARTESIAN_POINT('Ctrl Pts',(-41.6335679873822,38.0597947963058,39.3381388158227));
#31485=CARTESIAN_POINT('Ctrl Pts',(-41.6606497993463,38.1086989895731,39.3641519183711));
#31486=CARTESIAN_POINT('Ctrl Pts',(-41.6877316113105,38.1576031828404,39.3901650209196));
#31487=CARTESIAN_POINT('Ctrl Pts',(-41.7141963899058,38.2072013841032,39.4155157788624));
#31488=CARTESIAN_POINT('Ctrl Pts',(-41.7400260287181,38.2574596597474,39.4401868479652));
#31489=CARTESIAN_POINT('Ctrl Pts',(-41.7658556675304,38.3077179353917,39.464857917068));
#31490=CARTESIAN_POINT('Ctrl Pts',(-41.791050164947,38.3586362822818,39.4888492957924));
#31491=CARTESIAN_POINT('Ctrl Pts',(-41.8155922836422,38.4101798635953,39.5121445699468));
#31492=CARTESIAN_POINT('Ctrl Pts',(-41.8401344023374,38.4617234449088,39.5354398441012));
#31493=CARTESIAN_POINT('Ctrl Pts',(-41.8640241407791,38.5138922574272,39.558039012231));
#31494=CARTESIAN_POINT('Ctrl Pts',(-41.8872451543187,38.5666506088055,39.5799266126618));
#31495=CARTESIAN_POINT('Ctrl Pts',(-41.9104661678583,38.6194089601839,39.6018142130926));
#31496=CARTESIAN_POINT('Ctrl Pts',(-41.933018455046,38.672756847126,39.6229902444558));
#31497=CARTESIAN_POINT('Ctrl Pts',(-41.9548865862779,38.7266577705944,39.6434402187408));
#31498=CARTESIAN_POINT('Ctrl Pts',(-41.9767547175098,38.780558694063,39.6638901930257));
#31499=CARTESIAN_POINT('Ctrl Pts',(-41.9979386914205,38.8350126506927,39.6836141089556));
#31500=CARTESIAN_POINT('Ctrl Pts',(-42.0184240145653,38.8899823847063,39.7025984720138));
#31501=CARTESIAN_POINT('Ctrl Pts',(-42.03890933771,38.9449521187198,39.721582835072));
#31502=CARTESIAN_POINT('Ctrl Pts',(-42.0586960088098,39.0004376266851,39.739827644073));
#31503=CARTESIAN_POINT('Ctrl Pts',(-42.0777704904129,39.0564009470683,39.7573204164618));
#31504=CARTESIAN_POINT('Ctrl Pts',(-42.0968449720159,39.1123642674515,39.7748131888505));
#31505=CARTESIAN_POINT('Ctrl Pts',(-42.1152072629313,39.1688053967588,39.7915539235346));
#31506=CARTESIAN_POINT('Ctrl Pts',(-42.1328448002259,39.2256857196479,39.8075311670013));
#31507=CARTESIAN_POINT('Ctrl Pts',(-42.1504823375205,39.2825660425371,39.823508410468));
#31508=CARTESIAN_POINT('Ctrl Pts',(-42.167395120093,39.339885555457,39.8387221617199));
#31509=CARTESIAN_POINT('Ctrl Pts',(-42.1835715767208,39.3976050421022,39.8531620119607));
#31510=CARTESIAN_POINT('Ctrl Pts',(-42.1997480333486,39.4553245287473,39.8676018622016));
#31511=CARTESIAN_POINT('Ctrl Pts',(-42.2151881630216,39.5134439855139,39.88126781053));
#31512=CARTESIAN_POINT('Ctrl Pts',(-42.2298814020625,39.5719236487986,39.8941505071107));
#31513=CARTESIAN_POINT('Ctrl Pts',(-42.2445876996116,39.6304552854542,39.9070446530932));
#31514=CARTESIAN_POINT('Ctrl Pts',(-42.2585457774315,39.6893477655214,39.919154153688));
#31515=CARTESIAN_POINT('Ctrl Pts',(-42.2717460683851,39.7485607250761,39.9304707087187));
#31516=CARTESIAN_POINT('Ctrl Pts',(-41.0716296760129,37.3117369117769,38.8665566567506));
#31517=CARTESIAN_POINT('Ctrl Pts',(-41.1064421220777,37.352463364918,38.900933994226));
#31518=CARTESIAN_POINT('Ctrl Pts',(-41.1407310745976,37.3941228146786,38.9347361360592));
#31519=CARTESIAN_POINT('Ctrl Pts',(-41.1744715978335,37.4366849696814,38.967938504059));
#31520=CARTESIAN_POINT('Ctrl Pts',(-41.2082121210694,37.4792471246843,39.0011408720588));
#31521=CARTESIAN_POINT('Ctrl Pts',(-41.2414042126494,37.5227119819385,39.0337434638919));
#31522=CARTESIAN_POINT('Ctrl Pts',(-41.2740237329226,37.5670479395526,39.065722571987));
#31523=CARTESIAN_POINT('Ctrl Pts',(-41.3066432531957,37.6113838971666,39.0977016800822));
#31524=CARTESIAN_POINT('Ctrl Pts',(-41.3386901998686,37.6565909520255,39.1290573021918));
#31525=CARTESIAN_POINT('Ctrl Pts',(-41.3701412643704,37.7026362375212,39.1597666357266));
#31526=CARTESIAN_POINT('Ctrl Pts',(-41.4015923288721,37.748681523017,39.1904759692612));
#31527=CARTESIAN_POINT('Ctrl Pts',(-41.4324475089912,37.7955650359149,39.2205390120622));
#31528=CARTESIAN_POINT('Ctrl Pts',(-41.4626843610267,37.8432526925187,39.2499338995739));
#31529=CARTESIAN_POINT('Ctrl Pts',(-41.4929212130622,37.8909403491225,39.2793287870856));
#31530=CARTESIAN_POINT('Ctrl Pts',(-41.5225397348876,37.9394321460814,39.3080555172401));
#31531=CARTESIAN_POINT('Ctrl Pts',(-41.5515183802102,37.9886928320026,39.3360931952132));
#31532=CARTESIAN_POINT('Ctrl Pts',(-41.5804970255328,38.037953517924,39.3641308731862));
#31533=CARTESIAN_POINT('Ctrl Pts',(-41.6088357923143,38.0879830893467,39.3914794970048));
#31534=CARTESIAN_POINT('Ctrl Pts',(-41.6365140629105,38.1387451782573,39.4181191718634));
#31535=CARTESIAN_POINT('Ctrl Pts',(-41.6641923335067,38.1895072671679,39.4447588467219));
#31536=CARTESIAN_POINT('Ctrl Pts',(-41.6912101059702,38.2410018700011,39.4706895707464));
#31537=CARTESIAN_POINT('Ctrl Pts',(-41.7175477212022,38.2931915548211,39.4958924779976));
#31538=CARTESIAN_POINT('Ctrl Pts',(-41.7438853364341,38.345381239641,39.5210953852488));
#31539=CARTESIAN_POINT('Ctrl Pts',(-41.7695427925807,38.398266002784,39.5455704739551));
#31540=CARTESIAN_POINT('Ctrl Pts',(-41.7945014175986,38.4518074026242,39.5692999343967));
#31541=CARTESIAN_POINT('Ctrl Pts',(-41.8194600426163,38.5053488024645,39.5930293948383));
#31542=CARTESIAN_POINT('Ctrl Pts',(-41.8437198347484,38.5595468352414,39.6160132253448));
#31543=CARTESIAN_POINT('Ctrl Pts',(-41.8672631360878,38.6143621053489,39.6382346982561));
#31544=CARTESIAN_POINT('Ctrl Pts',(-41.8908064374271,38.6691773754566,39.6604561711674));
#31545=CARTESIAN_POINT('Ctrl Pts',(-41.913633246316,38.7246098790432,39.6819152849169));
#31546=CARTESIAN_POINT('Ctrl Pts',(-41.9357269446002,38.7806193235906,39.7025964181565));
#31547=CARTESIAN_POINT('Ctrl Pts',(-41.9578206428844,38.8366287681381,39.7232775513959));
#31548=CARTESIAN_POINT('Ctrl Pts',(-41.9791812290074,38.8932151497128,39.7431807026688));
#31549=CARTESIAN_POINT('Ctrl Pts',(-41.9997931486782,38.9503373372671,39.7622913796056));
#31550=CARTESIAN_POINT('Ctrl Pts',(-42.020405068349,39.0074595248213,39.7814020565424));
#31551=CARTESIAN_POINT('Ctrl Pts',(-42.0402683201149,39.0651175143432,39.7997202577963));
#31552=CARTESIAN_POINT('Ctrl Pts',(-42.0593684361201,39.1232693958493,39.8172326410076));
#31553=CARTESIAN_POINT('Ctrl Pts',(-42.0784685521253,39.1814212773554,39.834745024219));
#31554=CARTESIAN_POINT('Ctrl Pts',(-42.0968055310227,39.2400670467618,39.8514515881527));
#31555=CARTESIAN_POINT('Ctrl Pts',(-42.1143660123925,39.2991640758699,39.8673401598247));
#31556=CARTESIAN_POINT('Ctrl Pts',(-42.1319264937623,39.358261104978,39.8832287314966));
#31557=CARTESIAN_POINT('Ctrl Pts',(-42.1487104763651,39.4178093896378,39.8982993097854));
#31558=CARTESIAN_POINT('Ctrl Pts',(-42.164705726615,39.4777656451997,39.9125409087579));
#31559=CARTESIAN_POINT('Ctrl Pts',(-42.1807009768649,39.5377219007617,39.9267825077303));
#31560=CARTESIAN_POINT('Ctrl Pts',(-42.1959074936322,39.5980861230151,39.9401951263803));
#31561=CARTESIAN_POINT('Ctrl Pts',(-42.2103141879332,39.6588144335738,39.952768981783));
#31562=CARTESIAN_POINT('Ctrl Pts',(-42.224733686078,39.7195967159722,39.9653540121073));
#31563=CARTESIAN_POINT('Ctrl Pts',(-42.2383519384309,39.7807437298567,39.9770987867444));
#31564=CARTESIAN_POINT('Ctrl Pts',(-42.2511589902305,39.8422109481628,39.9879947171316));
#31565=CARTESIAN_POINT('Ctrl Pts',(-41.032404678088,37.313151892693,38.9045510432682));
#31566=CARTESIAN_POINT('Ctrl Pts',(-41.0682260642792,37.3551057079579,38.9400009816298));
#31567=CARTESIAN_POINT('Ctrl Pts',(-41.1034918563529,37.3980497307461,38.9748404534198));
#31568=CARTESIAN_POINT('Ctrl Pts',(-41.138174829136,37.4419508125435,39.0090425656379));
#31569=CARTESIAN_POINT('Ctrl Pts',(-41.1728578019191,37.4858518943408,39.0432446778559));
#31570=CARTESIAN_POINT('Ctrl Pts',(-41.206957952664,37.5307100316709,39.0768094277934));
#31571=CARTESIAN_POINT('Ctrl Pts',(-41.240448954355,37.5764906009263,39.1097109046596));
#31572=CARTESIAN_POINT('Ctrl Pts',(-41.2739399560461,37.6222711701815,39.1426123815259));
#31573=CARTESIAN_POINT('Ctrl Pts',(-41.3068218060297,37.6689741677376,39.1748505827146));
#31574=CARTESIAN_POINT('Ctrl Pts',(-41.3390691159587,37.7165635481547,39.2064006195102));
#31575=CARTESIAN_POINT('Ctrl Pts',(-41.3713164258876,37.7641529285719,39.2379506563058));
#31576=CARTESIAN_POINT('Ctrl Pts',(-41.4029291932065,37.8126286880828,39.2688125262086));
#31577=CARTESIAN_POINT('Ctrl Pts',(-41.4338830073062,37.8619534148612,39.2989624008741));
#31578=CARTESIAN_POINT('Ctrl Pts',(-41.4648368214059,37.9112781416396,39.3291122755395));
#31579=CARTESIAN_POINT('Ctrl Pts',(-41.495131679833,37.9614518317811,39.3585501525783));
#31580=CARTESIAN_POINT('Ctrl Pts',(-41.5247441872853,38.0124357646158,39.3872533006856));
#31581=CARTESIAN_POINT('Ctrl Pts',(-41.5543566947377,38.0634196974505,39.4159564487929));
#31582=CARTESIAN_POINT('Ctrl Pts',(-41.5832868488677,38.1152138689433,39.4439248656935));
#31583=CARTESIAN_POINT('Ctrl Pts',(-41.6115123056906,38.1677783091347,39.4711369521065));
#31584=CARTESIAN_POINT('Ctrl Pts',(-41.6397377625135,38.2203427493262,39.4983490385196));
#31585=CARTESIAN_POINT('Ctrl Pts',(-41.667258519791,38.2736774540562,39.5248047922876));
#31586=CARTESIAN_POINT('Ctrl Pts',(-41.6940533192522,38.3277412655495,39.5504837794006));
#31587=CARTESIAN_POINT('Ctrl Pts',(-41.7208481187134,38.3818050770429,39.5761627665136));
#31588=CARTESIAN_POINT('Ctrl Pts',(-41.746916958233,38.4365979910208,39.601064984935));
#31589=CARTESIAN_POINT('Ctrl Pts',(-41.7722396979839,38.4920777251902,39.625171197384));
#31590=CARTESIAN_POINT('Ctrl Pts',(-41.7975624377349,38.5475574593596,39.649277409833));
#31591=CARTESIAN_POINT('Ctrl Pts',(-41.8221390757079,38.6037240093296,39.672587614397));
#31592=CARTESIAN_POINT('Ctrl Pts',(-41.8459506215336,38.6605340333161,39.6950838001461));
#31593=CARTESIAN_POINT('Ctrl Pts',(-41.8697621673592,38.7173440573026,39.7175799858952));
#31594=CARTESIAN_POINT('Ctrl Pts',(-41.8928086191474,38.7747975508094,39.7392621510436));
#31595=CARTESIAN_POINT('Ctrl Pts',(-41.9150721652353,38.8328501792156,39.7601135387513));
#31596=CARTESIAN_POINT('Ctrl Pts',(-41.9373357113232,38.8909028076218,39.7809649264589));
#31597=CARTESIAN_POINT('Ctrl Pts',(-41.9588163499428,38.9495545663332,39.8009855350698));
#31598=CARTESIAN_POINT('Ctrl Pts',(-41.9794974755781,39.0087601960735,39.8201598876478));
#31599=CARTESIAN_POINT('Ctrl Pts',(-42.0001786012135,39.0679658258137,39.8393342402259));
#31600=CARTESIAN_POINT('Ctrl Pts',(-42.0200602122213,39.1277253218975,39.8576623352476));
#31601=CARTESIAN_POINT('Ctrl Pts',(-42.0391269348214,39.1879925699966,39.8751299995309));
#31602=CARTESIAN_POINT('Ctrl Pts',(-42.0581936574215,39.2482598180956,39.8925976638143));
#31603=CARTESIAN_POINT('Ctrl Pts',(-42.076445490098,39.3090348134404,39.9092048959701));
#31604=CARTESIAN_POINT('Ctrl Pts',(-42.0938683145047,39.37027065757,39.9249388484198));
#31605=CARTESIAN_POINT('Ctrl Pts',(-42.1112911389115,39.4315065016996,39.9406728008696));
#31606=CARTESIAN_POINT('Ctrl Pts',(-42.1278849536622,39.4932031897676,39.9555334723607));
#31607=CARTESIAN_POINT('Ctrl Pts',(-42.1436369176166,39.5553131113054,39.9695093607319));
#31608=CARTESIAN_POINT('Ctrl Pts',(-42.159388881571,39.6174230328432,39.9834852491031));
#31609=CARTESIAN_POINT('Ctrl Pts',(-42.1742989934744,39.6799461829352,39.9965763532405));
#31610=CARTESIAN_POINT('Ctrl Pts',(-42.1883557092036,39.742834312327,40.0087725341494));
#31611=CARTESIAN_POINT('Ctrl Pts',(-42.2024249177355,39.8057783330818,40.0209795543245));
#31612=CARTESIAN_POINT('Ctrl Pts',(-42.2156392113969,39.8690879771839,40.0322900588763));
#31613=CARTESIAN_POINT('Ctrl Pts',(-42.2279883336041,39.9327143005348,40.042695264256));
#31614=CARTESIAN_POINT('Ctrl Pts',(-40.9931478523898,37.3145297174934,38.942514127347));
#31615=CARTESIAN_POINT('Ctrl Pts',(-41.0299452813326,37.3576697439994,38.9789998578758));
#31616=CARTESIAN_POINT('Ctrl Pts',(-41.0661548143688,37.4018575474671,39.0148396298158));
#31617=CARTESIAN_POINT('Ctrl Pts',(-41.101746827141,37.447056976221,39.0500041213249));
#31618=CARTESIAN_POINT('Ctrl Pts',(-41.1373388399133,37.492256404975,39.085168612834));
#31619=CARTESIAN_POINT('Ctrl Pts',(-41.1723133292438,37.5384674549797,39.1196578207726));
#31620=CARTESIAN_POINT('Ctrl Pts',(-41.2066416812102,37.5856523192672,39.1534435282449));
#31621=CARTESIAN_POINT('Ctrl Pts',(-41.2409700331766,37.6328371835547,39.1872292357172));
#31622=CARTESIAN_POINT('Ctrl Pts',(-41.2746522447139,37.6809958579121,39.2203114397068));
#31623=CARTESIAN_POINT('Ctrl Pts',(-41.3076607591598,37.7300889419479,39.2526630744396));
#31624=CARTESIAN_POINT('Ctrl Pts',(-41.3406692736057,37.7791820259837,39.2850147091724));
#31625=CARTESIAN_POINT('Ctrl Pts',(-41.3730040880132,37.8292095153147,39.3166357717601));
#31626=CARTESIAN_POINT('Ctrl Pts',(-41.4046387480755,37.8801304806027,39.3475003918427));
#31627=CARTESIAN_POINT('Ctrl Pts',(-41.4362734081378,37.9310514458908,39.3783650119252));
#31628=CARTESIAN_POINT('Ctrl Pts',(-41.4672079110304,37.9828658825895,39.4084731867469));
#31629=CARTESIAN_POINT('Ctrl Pts',(-41.497416948093,38.035531399393,39.4378002836969));
#31630=CARTESIAN_POINT('Ctrl Pts',(-41.5276259851557,38.0881969161966,39.467127380647));
#31631=CARTESIAN_POINT('Ctrl Pts',(-41.5571095536913,38.1417135084029,39.4956733971071));
#31632=CARTESIAN_POINT('Ctrl Pts',(-41.5858435321026,38.1960373921097,39.523414978526));
#31633=CARTESIAN_POINT('Ctrl Pts',(-41.6145775105139,38.2503612758166,39.5511565599449));
#31634=CARTESIAN_POINT('Ctrl Pts',(-41.6425618962356,38.3054924461737,39.5780937038458));
#31635=CARTESIAN_POINT('Ctrl Pts',(-41.6697737942072,38.3613857983331,39.6042043719556));
#31636=CARTESIAN_POINT('Ctrl Pts',(-41.6969856921787,38.4172791504924,39.6303150400654));
#31637=CARTESIAN_POINT('Ctrl Pts',(-41.7234250999708,38.4739346794634,39.6555992300529));
#31638=CARTESIAN_POINT('Ctrl Pts',(-41.7490703865264,38.5313060332639,39.6800362559877));
#31639=CARTESIAN_POINT('Ctrl Pts',(-41.774715673082,38.5886773870644,39.7044732819225));
#31640=CARTESIAN_POINT('Ctrl Pts',(-41.7995668361116,38.646764560572,39.7280631416226));
#31641=CARTESIAN_POINT('Ctrl Pts',(-41.8236035439601,38.7055200305232,39.7507865353521));
#31642=CARTESIAN_POINT('Ctrl Pts',(-41.8476402518086,38.7642755004743,39.7735099290817));
#31643=CARTESIAN_POINT('Ctrl Pts',(-41.8708625023299,38.823699261623,39.7953668548117));
#31644=CARTESIAN_POINT('Ctrl Pts',(-41.8932512965426,38.8837426971939,39.8163394305834));
#31645=CARTESIAN_POINT('Ctrl Pts',(-41.9156400907553,38.9437861327649,39.8373120063552));
#31646=CARTESIAN_POINT('Ctrl Pts',(-41.9371954266605,39.0044492373971,39.8574002302962));
#31647=CARTESIAN_POINT('Ctrl Pts',(-41.957899669041,39.0656823803626,39.8765876674877));
#31648=CARTESIAN_POINT('Ctrl Pts',(-41.9786039114215,39.126915523328,39.8957751046793));
#31649=CARTESIAN_POINT('Ctrl Pts',(-41.9984570584289,39.1887186991596,39.9140617534086));
#31650=CARTESIAN_POINT('Ctrl Pts',(-42.0174428674697,39.2510413443948,39.9314326526921));
#31651=CARTESIAN_POINT('Ctrl Pts',(-42.0364286765105,39.3133639896299,39.9488035519757));
#31652=CARTESIAN_POINT('Ctrl Pts',(-42.0545471458897,39.3762060987042,39.9652587002625));
#31653=CARTESIAN_POINT('Ctrl Pts',(-42.0717834522178,39.4395162581656,39.9807846349878));
#31654=CARTESIAN_POINT('Ctrl Pts',(-42.0890197585458,39.5028264176271,39.9963105697131));
#31655=CARTESIAN_POINT('Ctrl Pts',(-42.1053739002838,39.566604621823,40.0109072894906));
#31656=CARTESIAN_POINT('Ctrl Pts',(-42.1208324975039,39.6307986914473,40.0245628522043));
#31657=CARTESIAN_POINT('Ctrl Pts',(-42.136291094724,39.6949927610715,40.038218414918));
#31658=CARTESIAN_POINT('Ctrl Pts',(-42.1508541460461,39.7596026903925,40.0509328193486));
#31659=CARTESIAN_POINT('Ctrl Pts',(-42.1645097368995,39.8245756196391,40.0626956633721));
#31660=CARTESIAN_POINT('Ctrl Pts',(-42.1781774640589,39.8896062930991,40.0744689615368));
#31661=CARTESIAN_POINT('Ctrl Pts',(-42.1909361158139,39.9550006061874,40.0852890061059));
#31662=CARTESIAN_POINT('Ctrl Pts',(-42.202775234616,40.0207049625231,40.0951469283655));
#31663=CARTESIAN_POINT('Ctrl Pts',(-40.9538910266915,37.3159075422938,38.9804772114259));
#31664=CARTESIAN_POINT('Ctrl Pts',(-40.991664498386,37.3602337800409,39.0179987341218));
#31665=CARTESIAN_POINT('Ctrl Pts',(-41.0288177723846,37.405665364188,39.0548388062119));
#31666=CARTESIAN_POINT('Ctrl Pts',(-41.0653188251461,37.4521631398986,39.090965677012));
#31667=CARTESIAN_POINT('Ctrl Pts',(-41.1018198779075,37.4986609156093,39.1270925478121));
#31668=CARTESIAN_POINT('Ctrl Pts',(-41.1376687058236,37.5462248782887,39.1625062137518));
#31669=CARTESIAN_POINT('Ctrl Pts',(-41.1728344080653,37.5948140376083,39.1971761518302));
#31670=CARTESIAN_POINT('Ctrl Pts',(-41.2080001103071,37.6434031969279,39.2318460899087));
#31671=CARTESIAN_POINT('Ctrl Pts',(-41.242482683398,37.6930175480867,39.2657722966988));
#31672=CARTESIAN_POINT('Ctrl Pts',(-41.2762524023609,37.7436143357411,39.2989255293689));
#31673=CARTESIAN_POINT('Ctrl Pts',(-41.3100221213238,37.7942111233955,39.332078762039));
#31674=CARTESIAN_POINT('Ctrl Pts',(-41.3430789828199,37.8457903425465,39.3644590173116));
#31675=CARTESIAN_POINT('Ctrl Pts',(-41.3753944888448,37.8983075463442,39.3960383828113));
#31676=CARTESIAN_POINT('Ctrl Pts',(-41.4077099948697,37.9508247501419,39.427617748311));
#31677=CARTESIAN_POINT('Ctrl Pts',(-41.4392841422278,38.0042799333979,39.4583962209154));
#31678=CARTESIAN_POINT('Ctrl Pts',(-41.4700897089007,38.0586270341703,39.4883472667082));
#31679=CARTESIAN_POINT('Ctrl Pts',(-41.5008952755737,38.1129741349427,39.5182983125011));
#31680=CARTESIAN_POINT('Ctrl Pts',(-41.5309322585149,38.1682131478626,39.5474219285207));
#31681=CARTESIAN_POINT('Ctrl Pts',(-41.5601747585147,38.2242964750848,39.5756930049455));
#31682=CARTESIAN_POINT('Ctrl Pts',(-41.5894172585144,38.280379802307,39.6039640813703));
#31683=CARTESIAN_POINT('Ctrl Pts',(-41.6178652726802,38.3373074382913,39.6313826154041));
#31684=CARTESIAN_POINT('Ctrl Pts',(-41.6454942691621,38.3950303311166,39.6579249645107));
#31685=CARTESIAN_POINT('Ctrl Pts',(-41.6731232656441,38.4527532239419,39.6844673136173));
#31686=CARTESIAN_POINT('Ctrl Pts',(-41.6999332417085,38.5112713679061,39.7101334751709));
#31687=CARTESIAN_POINT('Ctrl Pts',(-41.7259010750688,38.5705343413378,39.7349013145914));
#31688=CARTESIAN_POINT('Ctrl Pts',(-41.7518689084292,38.6297973147694,39.7596691540119));
#31689=CARTESIAN_POINT('Ctrl Pts',(-41.7769945965153,38.6898051118144,39.7835386688482));
#31690=CARTESIAN_POINT('Ctrl Pts',(-41.8012564663866,38.7505060277302,39.8064892705582));
#31691=CARTESIAN_POINT('Ctrl Pts',(-41.825518336258,38.811206943646,39.8294398722682));
#31692=CARTESIAN_POINT('Ctrl Pts',(-41.8489163855125,38.8726009724366,39.8514715585798));
#31693=CARTESIAN_POINT('Ctrl Pts',(-41.87143042785,38.9346352151722,39.8725653224156));
#31694=CARTESIAN_POINT('Ctrl Pts',(-41.8939444701875,38.9966694579078,39.8936590862515));
#31695=CARTESIAN_POINT('Ctrl Pts',(-41.9155745033782,39.059343908461,39.9138149255225));
#31696=CARTESIAN_POINT('Ctrl Pts',(-41.9363018625039,39.1226045646516,39.9330154473277));
#31697=CARTESIAN_POINT('Ctrl Pts',(-41.9570292216295,39.1858652208423,39.9522159691328));
#31698=CARTESIAN_POINT('Ctrl Pts',(-41.9768539046365,39.2497120764218,39.9704611715696));
#31699=CARTESIAN_POINT('Ctrl Pts',(-41.995758800118,39.3140901187931,39.9877353058533));
#31700=CARTESIAN_POINT('Ctrl Pts',(-42.0146636955995,39.3784681611643,40.005009440137));
#31701=CARTESIAN_POINT('Ctrl Pts',(-42.0326488016815,39.4433773839681,40.0213125045549));
#31702=CARTESIAN_POINT('Ctrl Pts',(-42.0496985899308,39.5087618587613,40.0366304215558));
#31703=CARTESIAN_POINT('Ctrl Pts',(-42.0667483781801,39.5741463335546,40.0519483385566));
#31704=CARTESIAN_POINT('Ctrl Pts',(-42.0828628469054,39.6400060538784,40.0662811066205));
#31705=CARTESIAN_POINT('Ctrl Pts',(-42.0980280773912,39.7062842715891,40.0796163436766));
#31706=CARTESIAN_POINT('Ctrl Pts',(-42.1131933078771,39.7725624892997,40.0929515807328));
#31707=CARTESIAN_POINT('Ctrl Pts',(-42.1274092986177,39.8392591978499,40.1052892854568));
#31708=CARTESIAN_POINT('Ctrl Pts',(-42.1406637645954,39.9063169269512,40.1166187925947));
#31709=CARTESIAN_POINT('Ctrl Pts',(-42.1539300103823,39.9734342531166,40.1279583687489));
#31710=CARTESIAN_POINT('Ctrl Pts',(-42.1662330202308,40.0409132351909,40.1382879533356));
#31711=CARTESIAN_POINT('Ctrl Pts',(-42.1775621356279,40.1086956245114,40.1475985924751));
#31712=CARTESIAN_POINT('Ctrl Pts',(-40.914602250515,37.3172480677314,39.0184088723865));
#31713=CARTESIAN_POINT('Ctrl Pts',(-40.9533187469713,37.3627192224956,39.0569292557962));
#31714=CARTESIAN_POINT('Ctrl Pts',(-40.9913825425138,37.4093536520098,39.0947324752628));
#31715=CARTESIAN_POINT('Ctrl Pts',(-41.0287591046217,37.4571090521964,39.1317842371774));
#31716=CARTESIAN_POINT('Ctrl Pts',(-41.0661356667296,37.5048644523831,39.168835999092));
#31717=CARTESIAN_POINT('Ctrl Pts',(-41.1028249913097,37.5537408180141,39.2051362993978));
#31718=CARTESIAN_POINT('Ctrl Pts',(-41.1387937910383,37.6036938137,39.2406522060533));
#31719=CARTESIAN_POINT('Ctrl Pts',(-41.1747625907669,37.6536468093859,39.2761681127087));
#31720=CARTESIAN_POINT('Ctrl Pts',(-41.2100108617045,37.7046764296586,39.3108996218247));
#31721=CARTESIAN_POINT('Ctrl Pts',(-41.2445066219746,37.7567363880459,39.3448152225293));
#31722=CARTESIAN_POINT('Ctrl Pts',(-41.2790023822446,37.8087963464333,39.378730823234));
#31723=CARTESIAN_POINT('Ctrl Pts',(-41.3127456280685,37.861886637237,39.4118305118128));
#31724=CARTESIAN_POINT('Ctrl Pts',(-41.3457057409081,37.9159591066578,39.4440842555981));
#31725=CARTESIAN_POINT('Ctrl Pts',(-41.3786658537476,37.9700315760786,39.4763379993834));
#31726=CARTESIAN_POINT('Ctrl Pts',(-41.4108428299918,38.0250862181985,39.5077457948421));
#31727=CARTESIAN_POINT('Ctrl Pts',(-41.4422074698689,38.0810730990221,39.5382791418741));
#31728=CARTESIAN_POINT('Ctrl Pts',(-41.473572109746,38.1370599798457,39.5688124889061));
#31729=CARTESIAN_POINT('Ctrl Pts',(-41.5041244098191,38.1939790932459,39.5984713841659));
#31730=CARTESIAN_POINT('Ctrl Pts',(-41.5338366419473,38.2517788153802,39.6272289117157));
#31731=CARTESIAN_POINT('Ctrl Pts',(-41.5635488740755,38.3095785375145,39.6559864392654));
#31732=CARTESIAN_POINT('Ctrl Pts',(-41.5924210350022,38.3682588620578,39.6838425959535));
#31733=CARTESIAN_POINT('Ctrl Pts',(-41.620426918423,38.4277665687249,39.7107720987361));
#31734=CARTESIAN_POINT('Ctrl Pts',(-41.6484328018438,38.4872742753919,39.7377016015187));
#31735=CARTESIAN_POINT('Ctrl Pts',(-41.6755724046885,38.5476093576708,39.7637044474438));
#31736=CARTESIAN_POINT('Ctrl Pts',(-41.7018210899449,38.6087170951247,39.7887570321441));
#31737=CARTESIAN_POINT('Ctrl Pts',(-41.7280697752014,38.6698248325786,39.8138096168443));
#31738=CARTESIAN_POINT('Ctrl Pts',(-41.7534275399913,38.7317052185206,39.8379119375725));
#31739=CARTESIAN_POINT('Ctrl Pts',(-41.7778713612163,38.7943021313656,39.8610421113869));
#31740=CARTESIAN_POINT('Ctrl Pts',(-41.8023151824413,38.8568990442106,39.8841722852013));
#31741=CARTESIAN_POINT('Ctrl Pts',(-41.8258450574193,38.9202124771122,39.9063303095674));
#31742=CARTESIAN_POINT('Ctrl Pts',(-41.8484396186719,38.9841850088691,39.9274960626028));
#31743=CARTESIAN_POINT('Ctrl Pts',(-41.8710341799246,39.048157540626,39.9486618156382));
#31744=CARTESIAN_POINT('Ctrl Pts',(-41.8926934249723,39.1127891642374,39.9688352950196));
#31745=CARTESIAN_POINT('Ctrl Pts',(-41.9133976806671,39.1780212627951,39.9879981763989));
#31746=CARTESIAN_POINT('Ctrl Pts',(-41.934101936362,39.2432533613527,40.0071610577782));
#31747=CARTESIAN_POINT('Ctrl Pts',(-41.9538512004312,39.3090859277148,40.0253133390478));
#31748=CARTESIAN_POINT('Ctrl Pts',(-41.9726275297141,39.3754592552988,40.0424385265866));
#31749=CARTESIAN_POINT('Ctrl Pts',(-41.9914038589971,39.4418325828827,40.0595637141254));
#31750=CARTESIAN_POINT('Ctrl Pts',(-42.0092072514307,39.5087466644251,40.0756618060513));
#31751=CARTESIAN_POINT('Ctrl Pts',(-42.0260215263681,39.5761408117013,40.0907181693781));
#31752=CARTESIAN_POINT('Ctrl Pts',(-42.0428358013054,39.6435349589775,40.1057745327049));
#31753=CARTESIAN_POINT('Ctrl Pts',(-42.0586609568976,39.7114091646121,40.1197891657764));
#31754=CARTESIAN_POINT('Ctrl Pts',(-42.0734826043543,39.7797018685422,40.1327493227831));
#31755=CARTESIAN_POINT('Ctrl Pts',(-42.0883042518111,39.8479945724722,40.1457094797898));
#31756=CARTESIAN_POINT('Ctrl Pts',(-42.102122389501,39.9167057672238,40.1576151593043));
#31757=CARTESIAN_POINT('Ctrl Pts',(-42.1149244465968,39.9857731322772,40.1684555258249));
#31758=CARTESIAN_POINT('Ctrl Pts',(-42.1277378814269,40.0549018804439,40.1793055266415));
#31759=CARTESIAN_POINT('Ctrl Pts',(-42.1395334273784,40.1243874247088,40.1890883188462));
#31760=CARTESIAN_POINT('Ctrl Pts',(-42.1503003257741,40.1941666288214,40.1977949731605));
#31761=CARTESIAN_POINT('Ctrl Pts',(-40.8752893413701,37.3185604200591,39.0563167987067));
#31762=CARTESIAN_POINT('Ctrl Pts',(-40.9149228371848,37.3651437030407,39.0958065436101));
#31763=CARTESIAN_POINT('Ctrl Pts',(-40.9538709279309,37.4129485471481,39.1345431904534));
#31764=CARTESIAN_POINT('Ctrl Pts',(-40.992096465966,37.4619293574053,39.1724897932637));
#31765=CARTESIAN_POINT('Ctrl Pts',(-41.030322004001,37.5109101676627,39.2104363960739));
#31766=CARTESIAN_POINT('Ctrl Pts',(-41.0678249846864,37.5610669381261,39.2475929502463));
#31767=CARTESIAN_POINT('Ctrl Pts',(-41.1045696386867,37.6123518306155,39.2839240168577));
#31768=CARTESIAN_POINT('Ctrl Pts',(-41.1413142926869,37.6636367231049,39.3202550834691));
#31769=CARTESIAN_POINT('Ctrl Pts',(-41.1773006155432,37.7160497313968,39.3557606581107));
#31770=CARTESIAN_POINT('Ctrl Pts',(-41.2124942844676,37.7695408653723,39.3904068765195));
#31771=CARTESIAN_POINT('Ctrl Pts',(-41.2476879533919,37.8230319993478,39.4250530949283));
#31772=CARTESIAN_POINT('Ctrl Pts',(-41.2820889641137,37.8776012525156,39.4588399529));
#31773=CARTESIAN_POINT('Ctrl Pts',(-41.315664505873,37.9331965781883,39.491735225437));
#31774=CARTESIAN_POINT('Ctrl Pts',(-41.3492400476323,37.988791903861,39.5246304979741));
#31775=CARTESIAN_POINT('Ctrl Pts',(-41.3819901163548,38.045413295292,39.5566341810848));
#31776=CARTESIAN_POINT('Ctrl Pts',(-41.4138834759049,38.1030067485194,39.5877157505161));
#31777=CARTESIAN_POINT('Ctrl Pts',(-41.445776835455,38.160600201747,39.6187973199473));
#31778=CARTESIAN_POINT('Ctrl Pts',(-41.4768134819625,38.219165709782,39.6489567719273));
#31779=CARTESIAN_POINT('Ctrl Pts',(-41.5069638135077,38.2786474144165,39.6781653411812));
#31780=CARTESIAN_POINT('Ctrl Pts',(-41.5371141450529,38.338129119051,39.707373910435));
#31781=CARTESIAN_POINT('Ctrl Pts',(-41.5663781579772,38.398527013067,39.7356315934182));
#31782=CARTESIAN_POINT('Ctrl Pts',(-41.5947279410512,38.4597834905756,39.7629114387119));
#31783=CARTESIAN_POINT('Ctrl Pts',(-41.6230777241252,38.5210399680844,39.7901912840056));
#31784=CARTESIAN_POINT('Ctrl Pts',(-41.6505132739087,38.5831550216525,39.8164932882995));
#31785=CARTESIAN_POINT('Ctrl Pts',(-41.6770084231115,38.6460694076107,39.8417923654484));
#31786=CARTESIAN_POINT('Ctrl Pts',(-41.7035035723143,38.7089837935689,39.8670914425974));
#31787=CARTESIAN_POINT('Ctrl Pts',(-41.7290583177212,38.7726975042826,39.8913875895315));
#31788=CARTESIAN_POINT('Ctrl Pts',(-41.7536482859026,38.8371497713265,39.9146576332384));
#31789=CARTESIAN_POINT('Ctrl Pts',(-41.778238254084,38.9016020383702,39.9379276769454));
#31790=CARTESIAN_POINT('Ctrl Pts',(-41.8018634420553,38.966792853926,39.9601716146042));
#31791=CARTESIAN_POINT('Ctrl Pts',(-41.8245013167481,39.0326600407391,39.9813682305393));
#31792=CARTESIAN_POINT('Ctrl Pts',(-41.847139191441,39.0985272275523,40.0025648464744));
#31793=CARTESIAN_POINT('Ctrl Pts',(-41.8687897501085,39.1650707776294,40.0227141381135));
#31794=CARTESIAN_POINT('Ctrl Pts',(-41.889432343028,39.2322272235272,40.0417968876091));
#31795=CARTESIAN_POINT('Ctrl Pts',(-41.9100749359475,39.2993836694249,40.0608796371047));
#31796=CARTESIAN_POINT('Ctrl Pts',(-41.9297095606148,39.3671530029904,40.0788958421384));
#31797=CARTESIAN_POINT('Ctrl Pts',(-41.9483174900524,39.4354705876543,40.0958283193379));
#31798=CARTESIAN_POINT('Ctrl Pts',(-41.9669254194899,39.5037881723181,40.1127607965374));
#31799=CARTESIAN_POINT('Ctrl Pts',(-41.9845066514397,39.5726539997901,40.1286095438481));
#31800=CARTESIAN_POINT('Ctrl Pts',(-42.001044417395,39.6420023876939,40.1433594451603));
#31801=CARTESIAN_POINT('Ctrl Pts',(-42.0175821833503,39.7113507755977,40.1581093464725));
#31802=CARTESIAN_POINT('Ctrl Pts',(-42.0330764813043,39.7811817155179,40.1717603999964));
#31803=CARTESIAN_POINT('Ctrl Pts',(-42.0475125332119,39.8514286045806,40.1842995857241));
#31804=CARTESIAN_POINT('Ctrl Pts',(-42.0619485851195,39.9216754936432,40.1968387714518));
#31805=CARTESIAN_POINT('Ctrl Pts',(-42.0753263892288,39.9923383233238,40.2082660878617));
#31806=CARTESIAN_POINT('Ctrl Pts',(-42.0876331861499,40.0633496973136,40.2185706358861));
#31807=CARTESIAN_POINT('Ctrl Pts',(-42.0999509206462,40.1344241821404,40.2288843420019));
#31808=CARTESIAN_POINT('Ctrl Pts',(-42.1111957419127,40.2058478224516,40.2380732818885));
#31809=CARTESIAN_POINT('Ctrl Pts',(-42.1213569049585,40.2775523754548,40.2461286748427));
#31810=CARTESIAN_POINT('Ctrl Pts',(-40.8359764322253,37.3198727723867,39.0942247250269));
#31811=CARTESIAN_POINT('Ctrl Pts',(-40.8765269273983,37.3675681835857,39.134683831424));
#31812=CARTESIAN_POINT('Ctrl Pts',(-40.916359313348,37.4165434422864,39.1743539056441));
#31813=CARTESIAN_POINT('Ctrl Pts',(-40.9554338273102,37.4667496626143,39.21319534935));
#31814=CARTESIAN_POINT('Ctrl Pts',(-40.9945083412725,37.5169558829423,39.2520367930559));
#31815=CARTESIAN_POINT('Ctrl Pts',(-41.0328249780631,37.568393058238,39.2900496010948));
#31816=CARTESIAN_POINT('Ctrl Pts',(-41.0703454863351,37.6210098475309,39.3271958276621));
#31817=CARTESIAN_POINT('Ctrl Pts',(-41.1078659946071,37.6736266368238,39.3643420542294));
#31818=CARTESIAN_POINT('Ctrl Pts',(-41.1445903693819,37.727423033135,39.4006216943967));
#31819=CARTESIAN_POINT('Ctrl Pts',(-41.1804819469606,37.7823453426986,39.4359985305097));
#31820=CARTESIAN_POINT('Ctrl Pts',(-41.2163735245393,37.8372676522623,39.4713753666227));
#31821=CARTESIAN_POINT('Ctrl Pts',(-41.2514323001588,37.8933158677943,39.505849393987));
#31822=CARTESIAN_POINT('Ctrl Pts',(-41.2856232708379,37.9504340497188,39.5393861952759));
#31823=CARTESIAN_POINT('Ctrl Pts',(-41.319814241517,38.0075522316433,39.5729229965647));
#31824=CARTESIAN_POINT('Ctrl Pts',(-41.3531374027178,38.0657403723855,39.6055225673275));
#31825=CARTESIAN_POINT('Ctrl Pts',(-41.3855594819409,38.1249403980169,39.637152359158));
#31826=CARTESIAN_POINT('Ctrl Pts',(-41.4179815611641,38.1841404236482,39.6687821509885));
#31827=CARTESIAN_POINT('Ctrl Pts',(-41.4495025541058,38.2443523263182,39.6994421596887));
#31828=CARTESIAN_POINT('Ctrl Pts',(-41.4800909850681,38.3055160134528,39.7291017706466));
#31829=CARTESIAN_POINT('Ctrl Pts',(-41.5106794160303,38.3666797005875,39.7587613816045));
#31830=CARTESIAN_POINT('Ctrl Pts',(-41.5403352809521,38.4287951640761,39.7874205908828));
#31831=CARTESIAN_POINT('Ctrl Pts',(-41.5690289636793,38.4918004124265,39.8150507786877));
#31832=CARTESIAN_POINT('Ctrl Pts',(-41.5977226464065,38.5548056607768,39.8426809664925));
#31833=CARTESIAN_POINT('Ctrl Pts',(-41.6254541431291,38.618700685634,39.8692821291552));
#31834=CARTESIAN_POINT('Ctrl Pts',(-41.6521957562781,38.6834217200966,39.8948276987528));
#31835=CARTESIAN_POINT('Ctrl Pts',(-41.6789373694272,38.7481427545592,39.9203732683505));
#31836=CARTESIAN_POINT('Ctrl Pts',(-41.7046890954511,38.8136897900448,39.9448632414905));
#31837=CARTESIAN_POINT('Ctrl Pts',(-41.7294252105889,38.8799974112873,39.96827315509));
#31838=CARTESIAN_POINT('Ctrl Pts',(-41.7541613257267,38.9463050325299,39.9916830686895));
#31839=CARTESIAN_POINT('Ctrl Pts',(-41.7778818266912,39.0133732307397,40.014012919641));
#31840=CARTESIAN_POINT('Ctrl Pts',(-41.8005630148243,39.0811350726091,40.0352403984758));
#31841=CARTESIAN_POINT('Ctrl Pts',(-41.8232442029574,39.1488969144785,40.0564678773107));
#31842=CARTESIAN_POINT('Ctrl Pts',(-41.8448860752447,39.2173523910215,40.0765929812073));
#31843=CARTESIAN_POINT('Ctrl Pts',(-41.8654670053889,39.2864331842592,40.0955955988193));
#31844=CARTESIAN_POINT('Ctrl Pts',(-41.8860479355331,39.3555139774971,40.1145982164313));
#31845=CARTESIAN_POINT('Ctrl Pts',(-41.9055679207984,39.4252200782661,40.1324783452289));
#31846=CARTESIAN_POINT('Ctrl Pts',(-41.9240074503906,39.4954819200098,40.1492181120892));
#31847=CARTESIAN_POINT('Ctrl Pts',(-41.9424469799828,39.5657437617536,40.1659578789494));
#31848=CARTESIAN_POINT('Ctrl Pts',(-41.9598060514486,39.636561335155,40.1815572816448));
#31849=CARTESIAN_POINT('Ctrl Pts',(-41.9760673084219,39.7078639636864,40.1960007209425));
#31850=CARTESIAN_POINT('Ctrl Pts',(-41.9923285653951,39.7791665922179,40.2104441602401));
#31851=CARTESIAN_POINT('Ctrl Pts',(-42.007492005711,39.8509542664238,40.2237316342165));
#31852=CARTESIAN_POINT('Ctrl Pts',(-42.0215424620695,39.923155340619,40.2358498486652));
#31853=CARTESIAN_POINT('Ctrl Pts',(-42.0355929184279,39.9953564148142,40.2479680631138));
#31854=CARTESIAN_POINT('Ctrl Pts',(-42.0485303889566,40.0679708794239,40.258917016419));
#31855=CARTESIAN_POINT('Ctrl Pts',(-42.0603419257029,40.14092626235,40.2686857459474));
#31856=CARTESIAN_POINT('Ctrl Pts',(-42.0721639598656,40.2139464838368,40.2784631573623));
#31857=CARTESIAN_POINT('Ctrl Pts',(-42.0828580564471,40.2873082201942,40.2870582449307));
#31858=CARTESIAN_POINT('Ctrl Pts',(-42.092413484143,40.3609381220883,40.2944623765249));
#31859=CARTESIAN_POINT('Ctrl Pts',(-40.7966393248313,37.3211568753947,39.1321088525032));
#31860=CARTESIAN_POINT('Ctrl Pts',(-40.8380807309094,37.3699315504519,39.1735077559943));
#31861=CARTESIAN_POINT('Ctrl Pts',(-40.8787711225811,37.4200447175752,39.2140814723113));
#31862=CARTESIAN_POINT('Ctrl Pts',(-40.9186680157922,37.4714440583024,39.2537876412842));
#31863=CARTESIAN_POINT('Ctrl Pts',(-40.9585649090031,37.5228433990297,39.293493810257));
#31864=CARTESIAN_POINT('Ctrl Pts',(-40.997668297963,37.5755289059027,39.3323324261235));
#31865=CARTESIAN_POINT('Ctrl Pts',(-41.0359373537698,37.6294455773984,39.3702629383271));
#31866=CARTESIAN_POINT('Ctrl Pts',(-41.0742064095767,37.6833622488941,39.4081934505307));
#31867=CARTESIAN_POINT('Ctrl Pts',(-41.1116411266758,37.7385100771898,39.4452158535664));
#31868=CARTESIAN_POINT('Ctrl Pts',(-41.1482024164183,37.7948314923221,39.4812914910072));
#31869=CARTESIAN_POINT('Ctrl Pts',(-41.1847637061608,37.8511529074543,39.5173671284481));
#31870=CARTESIAN_POINT('Ctrl Pts',(-41.2204515632392,37.9086479012521,39.5524959950575));
#31871=CARTESIAN_POINT('Ctrl Pts',(-41.2552287207357,37.9672564552801,39.5866414091118));
#31872=CARTESIAN_POINT('Ctrl Pts',(-41.2900058782322,38.0258650093081,39.620786823166));
#31873=CARTESIAN_POINT('Ctrl Pts',(-41.3238723310975,38.0855871150639,39.6539487797078));
#31874=CARTESIAN_POINT('Ctrl Pts',(-41.3567927118309,38.1463604307069,39.686092648179));
#31875=CARTESIAN_POINT('Ctrl Pts',(-41.3897130925642,38.2071337463499,39.7182365166501));
#31876=CARTESIAN_POINT('Ctrl Pts',(-41.4216873963851,38.2689582630641,39.7493622923831));
#31877=CARTESIAN_POINT('Ctrl Pts',(-41.452682228942,38.3317694455081,39.7794374681786));
#31878=CARTESIAN_POINT('Ctrl Pts',(-41.4836770614989,38.3945806279522,39.809512643974));
#31879=CARTESIAN_POINT('Ctrl Pts',(-41.5136924182901,38.458378467015,39.8385372154639));
#31880=CARTESIAN_POINT('Ctrl Pts',(-41.5426969477387,38.5230963683275,39.8664808665812));
#31881=CARTESIAN_POINT('Ctrl Pts',(-41.5717014771873,38.5878142696401,39.8944245176985));
#31882=CARTESIAN_POINT('Ctrl Pts',(-41.5996951750797,38.6534522238148,39.9212872443838));
#31883=CARTESIAN_POINT('Ctrl Pts',(-41.6266487979873,38.7199417162167,39.9470409849153));
#31884=CARTESIAN_POINT('Ctrl Pts',(-41.6536024208948,38.7864312086186,39.9727947254468));
#31885=CARTESIAN_POINT('Ctrl Pts',(-41.6795159649007,38.853772229603,39.997439476082));
#31886=CARTESIAN_POINT('Ctrl Pts',(-41.7043623557101,38.9218944870306,40.0209494879652));
#31887=CARTESIAN_POINT('Ctrl Pts',(-41.7292087465196,38.9900167444581,40.0444594998485));
#31888=CARTESIAN_POINT('Ctrl Pts',(-41.7529879805209,39.0589202284475,40.0668347695621));
#31889=CARTESIAN_POINT('Ctrl Pts',(-41.775675209024,39.1285330158191,40.088051914823));
#31890=CARTESIAN_POINT('Ctrl Pts',(-41.7983624375271,39.1981458031907,40.1092690600839));
#31891=CARTESIAN_POINT('Ctrl Pts',(-41.8199576572337,39.2684678838435,40.1293280778035));
#31892=CARTESIAN_POINT('Ctrl Pts',(-41.8404382968954,39.3394258534289,40.1482080010584));
#31893=CARTESIAN_POINT('Ctrl Pts',(-41.8609189365571,39.4103838230143,40.1670879243132));
#31894=CARTESIAN_POINT('Ctrl Pts',(-41.8802849931938,39.4819776712398,40.184788750356));
#31895=CARTESIAN_POINT('Ctrl Pts',(-41.898516220103,39.5541326655168,40.2012919713592));
#31896=CARTESIAN_POINT('Ctrl Pts',(-41.9167474470122,39.6262876597936,40.2177951923624));
#31897=CARTESIAN_POINT('Ctrl Pts',(-41.9338438415398,39.6990037896545,40.2331008059224));
#31898=CARTESIAN_POINT('Ctrl Pts',(-41.9497875237805,39.7722051500215,40.2471928019667));
#31899=CARTESIAN_POINT('Ctrl Pts',(-41.9657312060212,39.8454065103885,40.261284798011));
#31900=CARTESIAN_POINT('Ctrl Pts',(-41.9805221736516,39.9190930906431,40.2741631744854));
#31901=CARTESIAN_POINT('Ctrl Pts',(-41.9941449509075,39.9931879713497,40.2858144524841));
#31902=CARTESIAN_POINT('Ctrl Pts',(-42.0077677281635,40.0672828520561,40.2974657304829));
#31903=CARTESIAN_POINT('Ctrl Pts',(-42.0202223130583,40.1417860224648,40.307889908305));
#31904=CARTESIAN_POINT('Ctrl Pts',(-42.0314956662869,40.2166197091016,40.3170760664048));
#31905=CARTESIAN_POINT('Ctrl Pts',(-42.0427790386252,40.2915199036276,40.326270388635));
#31906=CARTESIAN_POINT('Ctrl Pts',(-42.0528790770922,40.3667511912548,40.3342244882568));
#31907=CARTESIAN_POINT('Ctrl Pts',(-42.061785177892,40.4422348971029,40.3409300056503));
#31908=CARTESIAN_POINT('Ctrl Pts',(-40.7572837211926,37.3224193856698,39.1699747890253));
#31909=CARTESIAN_POINT('Ctrl Pts',(-40.7995949415344,37.3722465378174,39.2122892402931));
#31910=CARTESIAN_POINT('Ctrl Pts',(-40.8411220393881,37.4234711881076,39.2537421264551));
#31911=CARTESIAN_POINT('Ctrl Pts',(-40.8818197056895,37.4760374467455,39.2942882194172));
#31912=CARTESIAN_POINT('Ctrl Pts',(-40.9225173719909,37.5286037053833,39.3348343123792));
#31913=CARTESIAN_POINT('Ctrl Pts',(-40.9623856002765,37.5825115640208,39.3744736057022));
#31914=CARTESIAN_POINT('Ctrl Pts',(-41.0013808914287,37.6377022052889,39.4131628500528));
#31915=CARTESIAN_POINT('Ctrl Pts',(-41.0403761825809,37.6928928465569,39.4518520944035));
#31916=CARTESIAN_POINT('Ctrl Pts',(-41.0784985304068,37.7493662616906,39.4895912836375));
#31917=CARTESIAN_POINT('Ctrl Pts',(-41.1157063406701,37.8070608341135,39.5263392415726));
#31918=CARTESIAN_POINT('Ctrl Pts',(-41.1529141509335,37.8647554065364,39.5630871995076));
#31919=CARTESIAN_POINT('Ctrl Pts',(-41.1892074177253,37.9236711270859,39.5988439203076));
#31920=CARTESIAN_POINT('Ctrl Pts',(-41.2245465424691,37.9837437144538,39.6335703908066));
#31921=CARTESIAN_POINT('Ctrl Pts',(-41.2598856672129,38.0438163018217,39.6682968613056));
#31922=CARTESIAN_POINT('Ctrl Pts',(-41.2942706442964,38.1050457464678,39.7019930759885));
#31923=CARTESIAN_POINT('Ctrl Pts',(-41.3276639572251,38.1673652426437,39.7346222698504));
#31924=CARTESIAN_POINT('Ctrl Pts',(-41.3610572701538,38.2296847388195,39.7672514637123));
#31925=CARTESIAN_POINT('Ctrl Pts',(-41.3934589136244,38.2930942766282,39.7988136315712));
#31926=CARTESIAN_POINT('Ctrl Pts',(-41.4248335351027,38.3575246716821,39.8292743368216));
#31927=CARTESIAN_POINT('Ctrl Pts',(-41.4562081565809,38.4219550667359,39.8597350420719));
#31928=CARTESIAN_POINT('Ctrl Pts',(-41.4865557510842,38.4874063088027,39.889094279876));
#31929=CARTESIAN_POINT('Ctrl Pts',(-41.515843207194,38.5538069858481,39.9173200171841));
#31930=CARTESIAN_POINT('Ctrl Pts',(-41.5451306633038,38.6202076628934,39.9455457544922));
#31931=CARTESIAN_POINT('Ctrl Pts',(-41.573357976369,38.687557764372,39.9726379868217));
#31932=CARTESIAN_POINT('Ctrl Pts',(-41.6004943483514,38.7557838064568,39.9985671545895));
#31933=CARTESIAN_POINT('Ctrl Pts',(-41.6276307203338,38.8240098485415,40.0244963223574));
#31934=CARTESIAN_POINT('Ctrl Pts',(-41.6536761469238,38.8931118203972,40.0492624214457));
#31935=CARTESIAN_POINT('Ctrl Pts',(-41.678602210679,38.9630143267796,40.0728384302508));
#31936=CARTESIAN_POINT('Ctrl Pts',(-41.7035282744343,39.032916833162,40.096414439056));
#31937=CARTESIAN_POINT('Ctrl Pts',(-41.7273349713962,39.1036198629696,40.1188003538339));
#31938=CARTESIAN_POINT('Ctrl Pts',(-41.7499963267383,39.1750462740882,40.1399717499339));
#31939=CARTESIAN_POINT('Ctrl Pts',(-41.7726576820804,39.2464726852068,40.1611431460339));
#31940=CARTESIAN_POINT('Ctrl Pts',(-41.7941736922047,39.3186224662897,40.1811000200909));
#31941=CARTESIAN_POINT('Ctrl Pts',(-41.8145208815876,39.3914168967189,40.199820597719));
#31942=CARTESIAN_POINT('Ctrl Pts',(-41.8348680709705,39.4642113271482,40.2185411753471));
#31943=CARTESIAN_POINT('Ctrl Pts',(-41.8540464363803,39.5376503953638,40.2360254535732));
#31944=CARTESIAN_POINT('Ctrl Pts',(-41.872035052837,39.6116539740283,40.2522543557809));
#31945=CARTESIAN_POINT('Ctrl Pts',(-41.8900236692937,39.6856575526928,40.2684832579885));
#31946=CARTESIAN_POINT('Ctrl Pts',(-41.9068225339406,39.7602256300532,40.2834567816001));
#31947=CARTESIAN_POINT('Ctrl Pts',(-41.922413318,39.8352768469571,40.2971585894254));
#31948=CARTESIAN_POINT('Ctrl Pts',(-41.9380041020594,39.910328063861,40.3108603972508));
#31949=CARTESIAN_POINT('Ctrl Pts',(-41.9523868030549,39.98586240839,40.3232904871139));
#31950=CARTESIAN_POINT('Ctrl Pts',(-41.9655457284236,40.0617974671075,40.3344352968825));
#31951=CARTESIAN_POINT('Ctrl Pts',(-41.9787046537923,40.1377325258248,40.3455801066511));
#31952=CARTESIAN_POINT('Ctrl Pts',(-41.9906398014448,40.2140682866706,40.3554396345553));
#31953=CARTESIAN_POINT('Ctrl Pts',(-42.001338149269,40.2907214618238,40.3640031231439));
#31954=CARTESIAN_POINT('Ctrl Pts',(-42.0120460051711,40.3674427619232,40.37257422247));
#31955=CARTESIAN_POINT('Ctrl Pts',(-42.0215148601722,40.4444820285852,40.3798469764035));
#31956=CARTESIAN_POINT('Ctrl Pts',(-42.0297343634969,40.5217550572279,40.3858134344673));
#31957=CARTESIAN_POINT('Ctrl Pts',(-40.7179281175539,37.3236818959449,39.2078407255475));
#31958=CARTESIAN_POINT('Ctrl Pts',(-40.7611091521593,37.374561525183,39.251070724592));
#31959=CARTESIAN_POINT('Ctrl Pts',(-40.8034729561951,37.4268976586399,39.2934027805989));
#31960=CARTESIAN_POINT('Ctrl Pts',(-40.8449713955868,37.4806308351885,39.3347887975501));
#31961=CARTESIAN_POINT('Ctrl Pts',(-40.8864698349786,37.534364011737,39.3761748145014));
#31962=CARTESIAN_POINT('Ctrl Pts',(-40.9271029025901,37.5894942221389,39.4166147852808));
#31963=CARTESIAN_POINT('Ctrl Pts',(-40.9668244290877,37.6459588331793,39.4560627617786));
#31964=CARTESIAN_POINT('Ctrl Pts',(-41.0065459555852,37.7024234442197,39.4955107382762));
#31965=CARTESIAN_POINT('Ctrl Pts',(-41.0453559341377,37.7602224461914,39.5339667137086));
#31966=CARTESIAN_POINT('Ctrl Pts',(-41.0832102649219,37.8192901759049,39.5713869921379));
#31967=CARTESIAN_POINT('Ctrl Pts',(-41.1210645957061,37.8783579056185,39.6088072705671));
#31968=CARTESIAN_POINT('Ctrl Pts',(-41.1579632722114,37.9386943529196,39.6451918455577));
#31969=CARTESIAN_POINT('Ctrl Pts',(-41.1938643642025,38.0002309736275,39.6804993725014));
#31970=CARTESIAN_POINT('Ctrl Pts',(-41.2297654561936,38.0617675943353,39.7158068994451));
#31971=CARTESIAN_POINT('Ctrl Pts',(-41.2646689574953,38.1245043778716,39.7500373722691));
#31972=CARTESIAN_POINT('Ctrl Pts',(-41.2985352026194,38.1883700545804,39.7831518915218));
#31973=CARTESIAN_POINT('Ctrl Pts',(-41.3324014477434,38.2522357312893,39.8162664107745));
#31974=CARTESIAN_POINT('Ctrl Pts',(-41.3652304308637,38.3172302901924,39.8482649707593));
#31975=CARTESIAN_POINT('Ctrl Pts',(-41.3969848412633,38.383279897856,39.8791112054645));
#31976=CARTESIAN_POINT('Ctrl Pts',(-41.428739251663,38.4493295055196,39.9099574401697));
#31977=CARTESIAN_POINT('Ctrl Pts',(-41.4594190838782,38.5164341505905,39.9396513442881));
#31978=CARTESIAN_POINT('Ctrl Pts',(-41.4889894666493,38.5845176033686,39.968159167787));
#31979=CARTESIAN_POINT('Ctrl Pts',(-41.5185598494203,38.6526010561467,39.9966669912859));
#31980=CARTESIAN_POINT('Ctrl Pts',(-41.5470207776582,38.7216633049293,40.0239887292596));
#31981=CARTESIAN_POINT('Ctrl Pts',(-41.5743398987155,38.7916258966968,40.0500933242638));
#31982=CARTESIAN_POINT('Ctrl Pts',(-41.6016590197727,38.8615884884645,40.076197919268));
#31983=CARTESIAN_POINT('Ctrl Pts',(-41.6278363289469,38.9324514111914,40.1010853668093));
#31984=CARTESIAN_POINT('Ctrl Pts',(-41.6528420656479,39.0041341665286,40.1247273725364));
#31985=CARTESIAN_POINT('Ctrl Pts',(-41.677847802349,39.0758169218658,40.1483693782635));
#31986=CARTESIAN_POINT('Ctrl Pts',(-41.7016819622716,39.1483194974918,40.1707659381056));
#31987=CARTESIAN_POINT('Ctrl Pts',(-41.7243174444527,39.2215595323573,40.1918915850447));
#31988=CARTESIAN_POINT('Ctrl Pts',(-41.7469529266338,39.294799567223,40.2130172319838));
#31989=CARTESIAN_POINT('Ctrl Pts',(-41.7683897271757,39.3687770487358,40.2328719623783));
#31990=CARTESIAN_POINT('Ctrl Pts',(-41.7886034662798,39.4434079400089,40.2514331943797));
#31991=CARTESIAN_POINT('Ctrl Pts',(-41.8088172053839,39.5180388312821,40.2699944263809));
#31992=CARTESIAN_POINT('Ctrl Pts',(-41.8278078795668,39.5933231194876,40.2872621567905));
#31993=CARTESIAN_POINT('Ctrl Pts',(-41.845553885571,39.6691752825398,40.3032167402025));
#31994=CARTESIAN_POINT('Ctrl Pts',(-41.8632998915752,39.745027445592,40.3191713236146));
#31995=CARTESIAN_POINT('Ctrl Pts',(-41.8798012263413,39.8214474704518,40.3338127572778));
#31996=CARTESIAN_POINT('Ctrl Pts',(-41.8950391122194,39.8983485438927,40.3471243768842));
#31997=CARTESIAN_POINT('Ctrl Pts',(-41.9102769980975,39.9752496173336,40.3604359964905));
#31998=CARTESIAN_POINT('Ctrl Pts',(-41.9242514324582,40.052631726137,40.3724177997423));
#31999=CARTESIAN_POINT('Ctrl Pts',(-41.9369465059397,40.1304069628652,40.3830561412809));
#32000=CARTESIAN_POINT('Ctrl Pts',(-41.9496415794212,40.2081821995935,40.3936944828194));
#32001=CARTESIAN_POINT('Ctrl Pts',(-41.9610572898313,40.2863505508764,40.4029893608057));
#32002=CARTESIAN_POINT('Ctrl Pts',(-41.971180632251,40.3648232145459,40.410930179883));
#32003=CARTESIAN_POINT('Ctrl Pts',(-41.981312971717,40.4433656202187,40.4188780563049));
#32004=CARTESIAN_POINT('Ctrl Pts',(-41.9901506432521,40.5222128659156,40.4254694645501));
#32005=CARTESIAN_POINT('Ctrl Pts',(-41.9976835491019,40.601275217353,40.4306968632843));
#32006=CARTESIAN_POINT('Ctrl Pts',(-40.6785539801473,37.3249227696823,39.2456884342118));
#32007=CARTESIAN_POINT('Ctrl Pts',(-40.7225836966845,37.3768280462168,39.2898096944072));
#32008=CARTESIAN_POINT('Ctrl Pts',(-40.7657628716283,37.4302491946363,39.3329964106504));
#32009=CARTESIAN_POINT('Ctrl Pts',(-40.8080404421579,37.4851230437161,39.3751975128904));
#32010=CARTESIAN_POINT('Ctrl Pts',(-40.8503180126875,37.5399968927959,39.4173986151304));
#32011=CARTESIAN_POINT('Ctrl Pts',(-40.8916939709274,37.5963234323158,39.4586140955063));
#32012=CARTESIAN_POINT('Ctrl Pts',(-40.9321193846504,37.654036057902,39.4987952130883));
#32013=CARTESIAN_POINT('Ctrl Pts',(-40.9725447983734,37.7117486834884,39.5389763306701));
#32014=CARTESIAN_POINT('Ctrl Pts',(-41.0120196600483,37.7708473843928,39.5781230779729));
#32015=CARTESIAN_POINT('Ctrl Pts',(-41.0504972836104,37.8312622803774,39.6161891583012));
#32016=CARTESIAN_POINT('Ctrl Pts',(-41.0889749071725,37.891677176362,39.6542552386296));
#32017=CARTESIAN_POINT('Ctrl Pts',(-41.1264552854528,37.9534082561759,39.6912406448916));
#32018=CARTESIAN_POINT('Ctrl Pts',(-41.1628940888185,38.0163825287324,39.7271016339729));
#32019=CARTESIAN_POINT('Ctrl Pts',(-41.1993328921841,38.0793568012888,39.7629626230543));
#32020=CARTESIAN_POINT('Ctrl Pts',(-41.234730113845,38.1435742548608,39.7976991882729));
#32021=CARTESIAN_POINT('Ctrl Pts',(-41.2690438853101,38.2089589598693,39.8312702434172));
#32022=CARTESIAN_POINT('Ctrl Pts',(-41.3033576567751,38.2743436648777,39.8648412985615));
#32023=CARTESIAN_POINT('Ctrl Pts',(-41.3365879716492,38.3408956091474,39.897246837375));
#32024=CARTESIAN_POINT('Ctrl Pts',(-41.3686955214862,38.4085361038988,39.9284485276018));
#32025=CARTESIAN_POINT('Ctrl Pts',(-41.4008030713232,38.4761765986501,39.9596502178287));
#32026=CARTESIAN_POINT('Ctrl Pts',(-41.4317878501381,38.5449056312883,39.9896480536529));
#32027=CARTESIAN_POINT('Ctrl Pts',(-41.4616132023931,38.614641939638,40.0184065473303));
#32028=CARTESIAN_POINT('Ctrl Pts',(-41.4914385546482,38.6843782479877,40.0471650410077));
#32029=CARTESIAN_POINT('Ctrl Pts',(-41.5201044747827,38.755121819064,40.0746841871765));
#32030=CARTESIAN_POINT('Ctrl Pts',(-41.5475770467723,38.8267890091748,40.1009314264494));
#32031=CARTESIAN_POINT('Ctrl Pts',(-41.5750496187618,38.8984561992857,40.1271786657222));
#32032=CARTESIAN_POINT('Ctrl Pts',(-41.6013288374831,38.9710469950868,40.1521539932042));
#32033=CARTESIAN_POINT('Ctrl Pts',(-41.6263836065667,39.044475568871,40.1758278548012));
#32034=CARTESIAN_POINT('Ctrl Pts',(-41.6514383756503,39.1179041426551,40.1995017163983));
#32035=CARTESIAN_POINT('Ctrl Pts',(-41.6752686904225,39.1921704807498,40.2218741076939));
#32036=CARTESIAN_POINT('Ctrl Pts',(-41.6978463476587,39.2671867740911,40.2429185497343));
#32037=CARTESIAN_POINT('Ctrl Pts',(-41.7204240048949,39.3422030674324,40.2639629917746));
#32038=CARTESIAN_POINT('Ctrl Pts',(-41.7417490003819,39.417969302052,40.2836794806318));
#32039=CARTESIAN_POINT('Ctrl Pts',(-41.7617960907045,39.4943958948663,40.3020446750837));
#32040=CARTESIAN_POINT('Ctrl Pts',(-41.781843181027,39.5708224876806,40.3204098695356));
#32041=CARTESIAN_POINT('Ctrl Pts',(-41.8006123624423,39.6479094244583,40.3374237661525));
#32042=CARTESIAN_POINT('Ctrl Pts',(-41.818081411026,39.7255655596244,40.353066216633));
#32043=CARTESIAN_POINT('Ctrl Pts',(-41.8355504596097,39.8032216947905,40.3687086671135));
#32044=CARTESIAN_POINT('Ctrl Pts',(-41.8517193720981,39.8814470138844,40.3829796685342));
#32045=CARTESIAN_POINT('Ctrl Pts',(-41.8665689966161,39.9601490240587,40.3958623131708));
#32046=CARTESIAN_POINT('Ctrl Pts',(-41.8814186211341,40.0388510342329,40.4087449578074));
#32047=CARTESIAN_POINT('Ctrl Pts',(-41.8949489549049,40.1180297208319,40.4202392432495));
#32048=CARTESIAN_POINT('Ctrl Pts',(-41.9071439634125,40.1975914621405,40.4303315423613));
#32049=CARTESIAN_POINT('Ctrl Pts',(-41.9193389719201,40.277153203449,40.440423841473));
#32050=CARTESIAN_POINT('Ctrl Pts',(-41.9301986528813,40.3570979846507,40.4491141523626));
#32051=CARTESIAN_POINT('Ctrl Pts',(-41.9397101270951,40.4373312762363,40.4563921607536));
#32052=CARTESIAN_POINT('Ctrl Pts',(-41.9492300545616,40.5176358745705,40.4636766374209));
#32053=CARTESIAN_POINT('Ctrl Pts',(-41.9573993760106,40.5982294813707,40.4695462987562));
#32054=CARTESIAN_POINT('Ctrl Pts',(-41.9642083721993,40.6790166284688,40.4739941491783));
#32055=CARTESIAN_POINT('Ctrl Pts',(-40.6391656485255,37.3261470729264,39.2835221829441));
#32056=CARTESIAN_POINT('Ctrl Pts',(-40.6840266281348,37.3790556848234,39.3285143662084));
#32057=CARTESIAN_POINT('Ctrl Pts',(-40.7280035489272,37.4335399036566,39.3725351780446));
#32058=CARTESIAN_POINT('Ctrl Pts',(-40.7710423171585,37.4895327111958,39.4155304707204));
#32059=CARTESIAN_POINT('Ctrl Pts',(-40.8140810853897,37.5455255187351,39.4585257633961));
#32060=CARTESIAN_POINT('Ctrl Pts',(-40.8561816923719,37.6030269036775,39.5004955282322));
#32061=CARTESIAN_POINT('Ctrl Pts',(-40.8972923523177,37.6619661365324,39.5413881403836));
#32062=CARTESIAN_POINT('Ctrl Pts',(-40.9384030122634,37.7209053693873,39.5822807525349));
#32063=CARTESIAN_POINT('Ctrl Pts',(-40.9785237168741,37.7812824382571,39.6220962037469));
#32064=CARTESIAN_POINT('Ctrl Pts',(-41.0176051157382,37.8430230764203,39.6607855190843));
#32065=CARTESIAN_POINT('Ctrl Pts',(-41.0566865146023,37.9047637145835,39.6994748344218));
#32066=CARTESIAN_POINT('Ctrl Pts',(-41.0947285998308,37.9678679095771,39.7370380060749));
#32067=CARTESIAN_POINT('Ctrl Pts',(-41.1316845778148,38.0322580401824,39.7734288295218));
#32068=CARTESIAN_POINT('Ctrl Pts',(-41.1686405557988,38.0966481707877,39.8098196529687));
#32069=CARTESIAN_POINT('Ctrl Pts',(-41.2045104190784,38.1623242240067,39.8450381208633));
#32070=CARTESIAN_POINT('Ctrl Pts',(-41.2392500459829,38.2292054151105,39.8790409127831));
#32071=CARTESIAN_POINT('Ctrl Pts',(-41.2739896728873,38.2960866062143,39.9130437047028));
#32072=CARTESIAN_POINT('Ctrl Pts',(-41.3075990564042,38.364172921702,39.9458308137839));
#32073=CARTESIAN_POINT('Ctrl Pts',(-41.3400368553625,38.4333806121052,39.9773619102927));
#32074=CARTESIAN_POINT('Ctrl Pts',(-41.3724746543208,38.5025883025084,40.0088930068016));
#32075=CARTESIAN_POINT('Ctrl Pts',(-41.4037408621726,38.5729173538569,40.0391680843732));
#32076=CARTESIAN_POINT('Ctrl Pts',(-41.4337970199666,38.6442812580081,40.0681499031948));
#32077=CARTESIAN_POINT('Ctrl Pts',(-41.4638531777607,38.7156451621594,40.0971317220163));
#32078=CARTESIAN_POINT('Ctrl Pts',(-41.4926992794298,38.7880439047079,40.1248202762375));
#32079=CARTESIAN_POINT('Ctrl Pts',(-41.5202998428706,38.861388431691,40.1511815075944));
#32080=CARTESIAN_POINT('Ctrl Pts',(-41.5479004063115,38.9347329586739,40.1775427389512));
#32081=CARTESIAN_POINT('Ctrl Pts',(-41.5742554259526,39.009023255286,40.2025766421226));
#32082=CARTESIAN_POINT('Ctrl Pts',(-41.5993324838422,39.084167940861,40.2262524241938));
#32083=CARTESIAN_POINT('Ctrl Pts',(-41.6244095417318,39.1593126264361,40.2499282062651));
#32084=CARTESIAN_POINT('Ctrl Pts',(-41.648208632808,39.2353116858053,40.2722458624571));
#32085=CARTESIAN_POINT('Ctrl Pts',(-41.6707004830348,39.3120716364419,40.2931779409709));
#32086=CARTESIAN_POINT('Ctrl Pts',(-41.6931923332617,39.3888315870784,40.3141100194848));
#32087=CARTESIAN_POINT('Ctrl Pts',(-41.7143769380992,39.4663524134872,40.3336565160952));
#32088=CARTESIAN_POINT('Ctrl Pts',(-41.7342282394564,39.5445387612942,40.3517933876636));
#32089=CARTESIAN_POINT('Ctrl Pts',(-41.7540795408135,39.6227251091012,40.3699302592321));
#32090=CARTESIAN_POINT('Ctrl Pts',(-41.7725975346832,39.7015769625234,40.3866575020975));
#32091=CARTESIAN_POINT('Ctrl Pts',(-41.7897594430353,39.7809973299591,40.4019545409404));
#32092=CARTESIAN_POINT('Ctrl Pts',(-41.8069213513874,39.8604176973947,40.4172515797833));
#32093=CARTESIAN_POINT('Ctrl Pts',(-41.8227271707575,39.9404065628119,40.4311184115157));
#32094=CARTESIAN_POINT('Ctrl Pts',(-41.8371574592217,40.0208655360286,40.4435379792625));
#32095=CARTESIAN_POINT('Ctrl Pts',(-41.8515877476859,40.1013245092453,40.4559575470093));
#32096=CARTESIAN_POINT('Ctrl Pts',(-41.8646425023312,40.18225357402,40.4669298482633));
#32097=CARTESIAN_POINT('Ctrl Pts',(-41.8763056651767,40.2635531836801,40.4764413865623));
#32098=CARTESIAN_POINT('Ctrl Pts',(-41.8879688280222,40.3448527933402,40.4859529248613));
#32099=CARTESIAN_POINT('Ctrl Pts',(-41.8982403967134,40.4265229314745,40.4940036982851));
#32100=CARTESIAN_POINT('Ctrl Pts',(-41.9071077367231,40.5084631398541,40.5005838039923));
#32101=CARTESIAN_POINT('Ctrl Pts',(-41.915982957516,40.5904761719918,40.5071697577201));
#32102=CARTESIAN_POINT('Ctrl Pts',(-41.9234514507292,40.6727597380641,40.5122824271486));
#32103=CARTESIAN_POINT('Ctrl Pts',(-41.9295040118784,40.755212445608,40.5159155106514));
#32104=CARTESIAN_POINT('Ctrl Pts',(-40.5997773169037,37.3273713761706,39.3213559316764));
#32105=CARTESIAN_POINT('Ctrl Pts',(-40.6454695595851,37.38128332343,39.3672190380096));
#32106=CARTESIAN_POINT('Ctrl Pts',(-40.6902442262262,37.4368306126769,39.4120739454389));
#32107=CARTESIAN_POINT('Ctrl Pts',(-40.734044192159,37.4939423786756,39.4558634285503));
#32108=CARTESIAN_POINT('Ctrl Pts',(-40.7778441580919,37.5510541446742,39.4996529116618));
#32109=CARTESIAN_POINT('Ctrl Pts',(-40.8206694138164,37.6097303750392,39.5423769609582));
#32110=CARTESIAN_POINT('Ctrl Pts',(-40.862465319985,37.6698962151627,39.583981067679));
#32111=CARTESIAN_POINT('Ctrl Pts',(-40.9042612261534,37.7300620552863,39.6255851743997));
#32112=CARTESIAN_POINT('Ctrl Pts',(-40.9450277736999,37.7917174921214,39.6660693295208));
#32113=CARTESIAN_POINT('Ctrl Pts',(-40.984712947866,37.8547838724632,39.7053818798674));
#32114=CARTESIAN_POINT('Ctrl Pts',(-41.024398122032,37.9178502528052,39.7446944302139));
#32115=CARTESIAN_POINT('Ctrl Pts',(-41.0630019142087,37.9823275629784,39.7828353672583));
#32116=CARTESIAN_POINT('Ctrl Pts',(-41.1004750668111,38.0481335516325,39.8197560250706));
#32117=CARTESIAN_POINT('Ctrl Pts',(-41.1379482194135,38.1139395402866,39.856676682883));
#32118=CARTESIAN_POINT('Ctrl Pts',(-41.1742907243117,38.1810741931526,39.8923770534537));
#32119=CARTESIAN_POINT('Ctrl Pts',(-41.2094562066557,38.2494518703517,39.926811582149));
#32120=CARTESIAN_POINT('Ctrl Pts',(-41.2446216889996,38.3178295475508,39.9612461108442));
#32121=CARTESIAN_POINT('Ctrl Pts',(-41.2786101411592,38.3874502342565,39.9944147901928));
#32122=CARTESIAN_POINT('Ctrl Pts',(-41.3113781892388,38.4582251203117,40.0262752929836));
#32123=CARTESIAN_POINT('Ctrl Pts',(-41.3441462373184,38.5290000063668,40.0581357957744));
#32124=CARTESIAN_POINT('Ctrl Pts',(-41.3756938742071,38.6009290764255,40.0886881150935));
#32125=CARTESIAN_POINT('Ctrl Pts',(-41.4059808375401,38.6739205763783,40.1178932590592));
#32126=CARTESIAN_POINT('Ctrl Pts',(-41.4362678008732,38.7469120763311,40.147098403025));
#32127=CARTESIAN_POINT('Ctrl Pts',(-41.4652940840769,38.820965990352,40.1749563652985));
#32128=CARTESIAN_POINT('Ctrl Pts',(-41.493022638969,38.8959878542071,40.2014315887393));
#32129=CARTESIAN_POINT('Ctrl Pts',(-41.5207511938611,38.9710097180622,40.2279068121803));
#32130=CARTESIAN_POINT('Ctrl Pts',(-41.547182014422,39.0469995154852,40.252999291041));
#32131=CARTESIAN_POINT('Ctrl Pts',(-41.5722813611177,39.1238603128512,40.2766769935864));
#32132=CARTESIAN_POINT('Ctrl Pts',(-41.5973807078133,39.2007211102171,40.3003546961319));
#32133=CARTESIAN_POINT('Ctrl Pts',(-41.6211485751934,39.2784528908609,40.3226176172202));
#32134=CARTESIAN_POINT('Ctrl Pts',(-41.643554618411,39.3569564987926,40.3434373322076));
#32135=CARTESIAN_POINT('Ctrl Pts',(-41.6659606616286,39.4354601067243,40.3642570471951));
#32136=CARTESIAN_POINT('Ctrl Pts',(-41.6870048758165,39.5147355249225,40.3836335515585));
#32137=CARTESIAN_POINT('Ctrl Pts',(-41.7066603882083,39.5946816277222,40.4015421002435));
#32138=CARTESIAN_POINT('Ctrl Pts',(-41.7263159006,39.6746277305219,40.4194506489285));
#32139=CARTESIAN_POINT('Ctrl Pts',(-41.7445827069242,39.7552445005886,40.4358912380425));
#32140=CARTESIAN_POINT('Ctrl Pts',(-41.7614374750446,39.8364291002939,40.4508428652477));
#32141=CARTESIAN_POINT('Ctrl Pts',(-41.778292243165,39.9176136999991,40.4657944924529));
#32142=CARTESIAN_POINT('Ctrl Pts',(-41.7937349694168,39.9993661117394,40.4792571544972));
#32143=CARTESIAN_POINT('Ctrl Pts',(-41.8077459218272,40.0815820479985,40.4912136453542));
#32144=CARTESIAN_POINT('Ctrl Pts',(-41.8217568742376,40.1637979842576,40.5031701362111));
#32145=CARTESIAN_POINT('Ctrl Pts',(-41.8343360497575,40.246477427208,40.5136204532771));
#32146=CARTESIAN_POINT('Ctrl Pts',(-41.8454673669409,40.3295149052198,40.5225512307633));
#32147=CARTESIAN_POINT('Ctrl Pts',(-41.8565986841243,40.4125523832314,40.5314820082495));
#32148=CARTESIAN_POINT('Ctrl Pts',(-41.8662821405455,40.4959478782984,40.5388932442076));
#32149=CARTESIAN_POINT('Ctrl Pts',(-41.8745053463511,40.5795950034718,40.544775447231));
#32150=CARTESIAN_POINT('Ctrl Pts',(-41.8827358604704,40.6633164694133,40.5506628780192));
#32151=CARTESIAN_POINT('Ctrl Pts',(-41.8895035254478,40.7472899947576,40.5550185555409));
#32152=CARTESIAN_POINT('Ctrl Pts',(-41.8947996515575,40.8314082627473,40.5578368721246));
#32153=CARTESIAN_POINT('Ctrl Pts',(-40.5603747681421,37.3285790821591,39.3591756979305));
#32154=CARTESIAN_POINT('Ctrl Pts',(-40.6068808335252,37.3834720268057,39.4058893665872));
#32155=CARTESIAN_POINT('Ctrl Pts',(-40.6524355994228,37.440060415916,39.4515577822779));
#32156=CARTESIAN_POINT('Ctrl Pts',(-40.6969788080551,37.4982694003275,39.4961205382474));
#32157=CARTESIAN_POINT('Ctrl Pts',(-40.7415220166874,37.556478384739,39.5406832942169));
#32158=CARTESIAN_POINT('Ctrl Pts',(-40.7850536576694,37.6163079508829,39.5841403800759));
#32159=CARTESIAN_POINT('Ctrl Pts',(-40.8275161474155,37.6776789650634,39.626434312041));
#32160=CARTESIAN_POINT('Ctrl Pts',(-40.8699786371616,37.7390499792439,39.668728244006));
#32161=CARTESIAN_POINT('Ctrl Pts',(-40.9113719657712,37.8019624271558,39.7098590122159));
#32162=CARTESIAN_POINT('Ctrl Pts',(-40.9516413760227,37.8663330996633,39.7497722077611));
#32163=CARTESIAN_POINT('Ctrl Pts',(-40.9919107862741,37.9307037721708,39.7896854033063));
#32164=CARTESIAN_POINT('Ctrl Pts',(-41.0310562687772,37.9965326542701,39.82838101688));
#32165=CARTESIAN_POINT('Ctrl Pts',(-41.0690260373813,38.0637326812403,39.8658078582303));
#32166=CARTESIAN_POINT('Ctrl Pts',(-41.1069958059855,38.1309327082104,39.9032346995806));
#32167=CARTESIAN_POINT('Ctrl Pts',(-41.1437898518358,38.1995038643887,39.9393927599795));
#32168=CARTESIAN_POINT('Ctrl Pts',(-41.1793594967149,38.2693554595067,39.9742342031185));
#32169=CARTESIAN_POINT('Ctrl Pts',(-41.2149291415941,38.3392070546247,40.0090756462575));
#32170=CARTESIAN_POINT('Ctrl Pts',(-41.2492743772058,38.4103390724019,40.0426004640103));
#32171=CARTESIAN_POINT('Ctrl Pts',(-41.282349761923,38.4826574366354,40.0747643004416));
#32172=CARTESIAN_POINT('Ctrl Pts',(-41.3154251466403,38.5549758008688,40.106928136873));
#32173=CARTESIAN_POINT('Ctrl Pts',(-41.3472306727472,38.6284804947033,40.1377309844799));
#32174=CARTESIAN_POINT('Ctrl Pts',(-41.3777242553182,38.7030743045571,40.1671320849417));
#32175=CARTESIAN_POINT('Ctrl Pts',(-41.4082178378893,38.7776681144109,40.1965331854034));
#32176=CARTESIAN_POINT('Ctrl Pts',(-41.4373994698095,38.8533510228988,40.2245325318599));
#32177=CARTESIAN_POINT('Ctrl Pts',(-41.4652305341039,38.9300229359037,40.2510930713476));
#32178=CARTESIAN_POINT('Ctrl Pts',(-41.4930615983982,39.0066948489086,40.2776536108352));
#32179=CARTESIAN_POINT('Ctrl Pts',(-41.5195420885715,39.0843557485611,40.3027753371549));
#32180=CARTESIAN_POINT('Ctrl Pts',(-41.5446369576921,39.1629029246618,40.3264250006599));
#32181=CARTESIAN_POINT('Ctrl Pts',(-41.5697318268126,39.2414501007626,40.3500746641649));
#32182=CARTESIAN_POINT('Ctrl Pts',(-41.593441069022,39.3208835350051,40.3722522593337));
#32183=CARTESIAN_POINT('Ctrl Pts',(-41.6157333000996,39.4010981724733,40.3929284277542));
#32184=CARTESIAN_POINT('Ctrl Pts',(-41.6380255311772,39.4813128099415,40.4136045961748));
#32185=CARTESIAN_POINT('Ctrl Pts',(-41.6589007459169,39.5623086319402,40.4327793330178));
#32186=CARTESIAN_POINT('Ctrl Pts',(-41.6783313058059,39.6439785163979,40.4504272487505));
#32187=CARTESIAN_POINT('Ctrl Pts',(-41.697761865695,39.7256484008556,40.4680751644832));
#32188=CARTESIAN_POINT('Ctrl Pts',(-41.7157477661934,39.8079923287374,40.4841962549813));
#32189=CARTESIAN_POINT('Ctrl Pts',(-41.7322651876043,39.8909013938422,40.4987691667571));
#32190=CARTESIAN_POINT('Ctrl Pts',(-41.7487826090152,39.973810458947,40.513342078533));
#32191=CARTESIAN_POINT('Ctrl Pts',(-41.7638315474766,40.0572846419505,40.5263668081778));
#32192=CARTESIAN_POINT('Ctrl Pts',(-41.7773920651324,40.1412135402639,40.537826094759));
#32193=CARTESIAN_POINT('Ctrl Pts',(-41.7909525827882,40.2251424385774,40.5492853813402));
#32194=CARTESIAN_POINT('Ctrl Pts',(-41.8030246764649,40.3095260326383,40.5591792221737));
#32195=CARTESIAN_POINT('Ctrl Pts',(-41.8135923429232,40.3942527151709,40.5674944945855));
#32196=CARTESIAN_POINT('Ctrl Pts',(-41.8241600093816,40.4789793977035,40.5758097669973));
#32197=CARTESIAN_POINT('Ctrl Pts',(-41.8332232461447,40.5640491489585,40.5825464690351));
#32198=CARTESIAN_POINT('Ctrl Pts',(-41.8407700269778,40.6493494518621,40.5876956510615));
#32199=CARTESIAN_POINT('Ctrl Pts',(-41.848323514957,40.7347255647833,40.5928494093856));
#32200=CARTESIAN_POINT('Ctrl Pts',(-41.8543578485532,40.8203326194182,40.5964128234335));
#32201=CARTESIAN_POINT('Ctrl Pts',(-41.858864989028,40.9060571842964,40.5983811276797));
#32202=CARTESIAN_POINT('Ctrl Pts',(-40.5209614242509,37.3297741857869,39.3969848472346));
#32203=CARTESIAN_POINT('Ctrl Pts',(-40.5682667277247,37.3856292560404,39.4445317407691));
#32204=CARTESIAN_POINT('Ctrl Pts',(-40.614586797881,37.4432402480706,39.4909960961139));
#32205=CARTESIAN_POINT('Ctrl Pts',(-40.6598581425081,37.502528192884,39.5363142232817));
#32206=CARTESIAN_POINT('Ctrl Pts',(-40.7051294871352,37.5618161376976,39.5816323504493));
#32207=CARTESIAN_POINT('Ctrl Pts',(-40.7493520948838,37.6227810204313,39.625804238079));
#32208=CARTESIAN_POINT('Ctrl Pts',(-40.7924653485924,37.6853392748206,39.6687693385324));
#32209=CARTESIAN_POINT('Ctrl Pts',(-40.835578602301,37.7478975292098,39.7117344389858));
#32210=CARTESIAN_POINT('Ctrl Pts',(-40.8775824911613,37.8120491395717,39.7534927414919));
#32211=CARTESIAN_POINT('Ctrl Pts',(-40.9184194392716,37.8777061715048,39.7939870067811));
#32212=CARTESIAN_POINT('Ctrl Pts',(-40.9592563873819,37.9433632034379,39.8344812720702));
#32213=CARTESIAN_POINT('Ctrl Pts',(-40.9989263845046,38.0105256404827,39.8737114899907));
#32214=CARTESIAN_POINT('Ctrl Pts',(-41.0373750538685,38.0791014212136,39.911623886589));
#32215=CARTESIAN_POINT('Ctrl Pts',(-41.0758237232324,38.1476772019446,39.9495362831873));
#32216=CARTESIAN_POINT('Ctrl Pts',(-41.1130510551986,38.2176663091703,39.986130848959));
#32217=CARTESIAN_POINT('Ctrl Pts',(-41.1490060212252,38.2889728068698,40.0213574227123));
#32218=CARTESIAN_POINT('Ctrl Pts',(-41.1849609872517,38.3602793045694,40.0565839964655));
#32219=CARTESIAN_POINT('Ctrl Pts',(-41.219643578325,38.4329031748667,40.0904425693693));
#32220=CARTESIAN_POINT('Ctrl Pts',(-41.2530062540501,38.5067448701977,40.1228867305336));
#32221=CARTESIAN_POINT('Ctrl Pts',(-41.2863689297752,38.5805865655286,40.1553308916979));
#32222=CARTESIAN_POINT('Ctrl Pts',(-41.3184116817886,38.6556460673815,40.1863606329891));
#32223=CARTESIAN_POINT('Ctrl Pts',(-41.3490905881962,38.7318204896042,40.2159334210757));
#32224=CARTESIAN_POINT('Ctrl Pts',(-41.379769494604,38.8079949118268,40.2455062091623));
#32225=CARTESIAN_POINT('Ctrl Pts',(-41.4090845477151,38.8852842353228,40.2736220366305));
#32226=CARTESIAN_POINT('Ctrl Pts',(-41.4369955645689,38.9635825174611,40.3002423643315));
#32227=CARTESIAN_POINT('Ctrl Pts',(-41.4649065814228,39.0418807995995,40.3268626920326));
#32228=CARTESIAN_POINT('Ctrl Pts',(-41.4914135550221,39.1211880207514,40.3519875132929));
#32229=CARTESIAN_POINT('Ctrl Pts',(-41.5164801515192,39.2013954722972,40.3755823888195));
#32230=CARTESIAN_POINT('Ctrl Pts',(-41.5415467480163,39.281602923843,40.3991772643461));
#32231=CARTESIAN_POINT('Ctrl Pts',(-41.565172961127,39.3627105856755,40.4212421882239));
#32232=CARTESIAN_POINT('Ctrl Pts',(-41.5873264057423,39.4446072812604,40.4417469154463));
#32233=CARTESIAN_POINT('Ctrl Pts',(-41.6094798503576,39.5265039768455,40.4622516426688));
#32234=CARTESIAN_POINT('Ctrl Pts',(-41.6301605209237,39.6091896856524,40.4811961680955));
#32235=CARTESIAN_POINT('Ctrl Pts',(-41.6493400698688,39.6925510680742,40.4985545239373));
#32236=CARTESIAN_POINT('Ctrl Pts',(-41.6685196188139,39.7759124504959,40.5159128797791));
#32237=CARTESIAN_POINT('Ctrl Pts',(-41.6861980413298,39.8599494856346,40.5316850616842));
#32238=CARTESIAN_POINT('Ctrl Pts',(-41.7023511051097,39.9445469815827,40.5458494502833));
#32239=CARTESIAN_POINT('Ctrl Pts',(-41.7185041688897,40.0291444775307,40.5600138388823));
#32240=CARTESIAN_POINT('Ctrl Pts',(-41.7331318698843,40.1143024130801,40.5725704306242));
#32241=CARTESIAN_POINT('Ctrl Pts',(-41.7462141574959,40.1999040598739,40.5835020138387));
#32242=CARTESIAN_POINT('Ctrl Pts',(-41.7592964451075,40.2855057066677,40.5944335970531));
#32243=CARTESIAN_POINT('Ctrl Pts',(-41.7708333160563,40.3715510432463,40.6037401689996));
#32244=CARTESIAN_POINT('Ctrl Pts',(-41.7808089564319,40.4579221248672,40.6114089729004));
#32245=CARTESIAN_POINT('Ctrl Pts',(-41.7907845968073,40.5442932064881,40.6190777768011));
#32246=CARTESIAN_POINT('Ctrl Pts',(-41.7991990041087,40.6309900114988,40.6251088107337));
#32247=CARTESIAN_POINT('Ctrl Pts',(-41.806040644473,40.7178937021711,40.6294938077917));
#32248=CARTESIAN_POINT('Ctrl Pts',(-41.812888365295,40.8048746278599,40.6338827019837));
#32249=CARTESIAN_POINT('Ctrl Pts',(-41.8181605206493,40.8920627852852,40.6366226310933));
#32250=CARTESIAN_POINT('Ctrl Pts',(-41.8218498690737,40.9793384509368,40.6377098307341));
#32251=CARTESIAN_POINT('Ctrl Pts',(-40.4815480803598,37.3309692894148,39.4347939965387));
#32252=CARTESIAN_POINT('Ctrl Pts',(-40.5296526219241,37.3877864852751,39.4831741149509));
#32253=CARTESIAN_POINT('Ctrl Pts',(-40.5767379963392,37.4464200802252,39.53043440995));
#32254=CARTESIAN_POINT('Ctrl Pts',(-40.6227374769611,37.5067869854406,39.5765079083159));
#32255=CARTESIAN_POINT('Ctrl Pts',(-40.668736957583,37.567153890656,39.6225814066818));
#32256=CARTESIAN_POINT('Ctrl Pts',(-40.7136505320982,37.6292540899798,39.667468096082));
#32257=CARTESIAN_POINT('Ctrl Pts',(-40.7574145497693,37.6929995845778,39.7111043650238));
#32258=CARTESIAN_POINT('Ctrl Pts',(-40.8011785674403,37.7567450791758,39.7547406339656));
#32259=CARTESIAN_POINT('Ctrl Pts',(-40.8437930165514,37.8221358519875,39.7971264707679));
#32260=CARTESIAN_POINT('Ctrl Pts',(-40.8851975025205,37.8890792433462,39.838201805801));
#32261=CARTESIAN_POINT('Ctrl Pts',(-40.9266019884896,37.956022634705,39.8792771408341));
#32262=CARTESIAN_POINT('Ctrl Pts',(-40.966796500232,38.0245186266951,39.9190419631016));
#32263=CARTESIAN_POINT('Ctrl Pts',(-41.0057240703556,38.0944701611869,39.9574399149478));
#32264=CARTESIAN_POINT('Ctrl Pts',(-41.0446516404792,38.1644216956787,39.9958378667941));
#32265=CARTESIAN_POINT('Ctrl Pts',(-41.0823122585615,38.2358287539518,40.0328689379385));
#32266=CARTESIAN_POINT('Ctrl Pts',(-41.1186525457355,38.308590154233,40.068480642306));
#32267=CARTESIAN_POINT('Ctrl Pts',(-41.1549928329094,38.3813515545141,40.1040923466735));
#32268=CARTESIAN_POINT('Ctrl Pts',(-41.1900127794441,38.4554672773316,40.1382846747284));
#32269=CARTESIAN_POINT('Ctrl Pts',(-41.2236627461772,38.53083230376,40.1710091606256));
#32270=CARTESIAN_POINT('Ctrl Pts',(-41.2573127129103,38.6061973301884,40.2037336465228));
#32271=CARTESIAN_POINT('Ctrl Pts',(-41.2895926908299,38.6828116400597,40.2349902814984));
#32272=CARTESIAN_POINT('Ctrl Pts',(-41.3204569210743,38.7605666746512,40.2647347572098));
#32273=CARTESIAN_POINT('Ctrl Pts',(-41.3513211513187,38.8383217092427,40.2944792329211));
#32274=CARTESIAN_POINT('Ctrl Pts',(-41.3807696256207,38.9172174477468,40.322711541401));
#32275=CARTESIAN_POINT('Ctrl Pts',(-41.408760595034,38.9971420990185,40.3493916573154));
#32276=CARTESIAN_POINT('Ctrl Pts',(-41.4367515644473,39.0770667502903,40.3760717732299));
#32277=CARTESIAN_POINT('Ctrl Pts',(-41.4632850214728,39.1580202929416,40.4011996894309));
#32278=CARTESIAN_POINT('Ctrl Pts',(-41.4883233453464,39.2398880199326,40.4247397769792));
#32279=CARTESIAN_POINT('Ctrl Pts',(-41.51336166922,39.3217557469235,40.4482798645274));
#32280=CARTESIAN_POINT('Ctrl Pts',(-41.5369048532321,39.4045376363458,40.4702321171141));
#32281=CARTESIAN_POINT('Ctrl Pts',(-41.558919511385,39.4881163900476,40.4905654031384));
#32282=CARTESIAN_POINT('Ctrl Pts',(-41.580934169538,39.5716951437495,40.5108986891627));
#32283=CARTESIAN_POINT('Ctrl Pts',(-41.6014202959306,39.6560707393645,40.5296130031733));
#32284=CARTESIAN_POINT('Ctrl Pts',(-41.6203488339317,39.7411236197504,40.5466817991241));
#32285=CARTESIAN_POINT('Ctrl Pts',(-41.6392773719328,39.8261765001363,40.5637505950749));
#32286=CARTESIAN_POINT('Ctrl Pts',(-41.6566483164661,39.9119066425318,40.5791738683872));
#32287=CARTESIAN_POINT('Ctrl Pts',(-41.6724370226152,39.9981925693231,40.5929297338094));
#32288=CARTESIAN_POINT('Ctrl Pts',(-41.6882257287643,40.0844784961144,40.6066855992316));
#32289=CARTESIAN_POINT('Ctrl Pts',(-41.7024321922921,40.1713201842097,40.6187740530706));
#32290=CARTESIAN_POINT('Ctrl Pts',(-41.7150362498594,40.2585945794838,40.6291779329183));
#32291=CARTESIAN_POINT('Ctrl Pts',(-41.7276403074267,40.345868974758,40.639581812766));
#32292=CARTESIAN_POINT('Ctrl Pts',(-41.7386419556478,40.4335760538542,40.6483011158255));
#32293=CARTESIAN_POINT('Ctrl Pts',(-41.7480255699405,40.5215915345635,40.6553234512153));
#32294=CARTESIAN_POINT('Ctrl Pts',(-41.7574091842331,40.6096070152727,40.6623457866051));
#32295=CARTESIAN_POINT('Ctrl Pts',(-41.7651747620727,40.697930874039,40.6676711524323));
#32296=CARTESIAN_POINT('Ctrl Pts',(-41.7713112619682,40.78643795248,40.6712919645219));
#32297=CARTESIAN_POINT('Ctrl Pts',(-41.777453215633,40.8750236909366,40.6749159945816));
#32298=CARTESIAN_POINT('Ctrl Pts',(-41.7819631927455,40.9637929511522,40.6768324387531));
#32299=CARTESIAN_POINT('Ctrl Pts',(-41.7848347491195,41.0526197175773,40.6770385337885));
#32300=CARTESIAN_POINT('Ctrl Pts',(-40.4421239266209,37.3321517734995,39.4725925144174));
#32301=CARTESIAN_POINT('Ctrl Pts',(-40.4910131080268,37.3899122066288,39.521788505816));
#32302=CARTESIAN_POINT('Ctrl Pts',(-40.5388489780531,37.4495498910191,39.5698271574031));
#32303=CARTESIAN_POINT('Ctrl Pts',(-40.5855614742959,37.510977482102,39.6166381108269));
#32304=CARTESIAN_POINT('Ctrl Pts',(-40.6322739705388,37.5724050731848,39.6634490642507));
#32305=CARTESIAN_POINT('Ctrl Pts',(-40.6778630796419,37.6356225533988,39.709032306127));
#32306=CARTESIAN_POINT('Ctrl Pts',(-40.7222620279456,37.70053733785,39.753321072269));
#32307=CARTESIAN_POINT('Ctrl Pts',(-40.7666609762493,37.7654521223013,39.797609838411));
#32308=CARTESIAN_POINT('Ctrl Pts',(-40.809869751058,37.8320641924323,39.8406041161547));
#32309=CARTESIAN_POINT('Ctrl Pts',(-40.8518250628848,37.9002759939679,39.8822409308761));
#32310=CARTESIAN_POINT('Ctrl Pts',(-40.8937803747117,37.9684877955036,39.9238777455974));
#32311=CARTESIAN_POINT('Ctrl Pts',(-40.9344822115587,38.0382993089447,39.9641570853898));
#32312=CARTESIAN_POINT('Ctrl Pts',(-40.9738709533507,38.1096082961141,40.0030199495069));
#32313=CARTESIAN_POINT('Ctrl Pts',(-41.0132596951426,38.1809172832835,40.041882813624));
#32314=CARTESIAN_POINT('Ctrl Pts',(-41.0513353306142,38.2537237237974,40.0793291909511));
#32315=CARTESIAN_POINT('Ctrl Pts',(-41.0880420836084,38.3279209947579,40.1153042273124));
#32316=CARTESIAN_POINT('Ctrl Pts',(-41.1247488366024,38.4021182657185,40.1512792636738));
#32317=CARTESIAN_POINT('Ctrl Pts',(-41.1600866966196,38.4777063459167,40.1857829487792));
#32318=CARTESIAN_POINT('Ctrl Pts',(-41.1940038946856,38.5545745397419,40.2187647355886));
#32319=CARTESIAN_POINT('Ctrl Pts',(-41.2279210927516,38.6314427335672,40.2517465223981));
#32320=CARTESIAN_POINT('Ctrl Pts',(-41.2604176191636,38.7095910190472,40.2832064014761));
#32321=CARTESIAN_POINT('Ctrl Pts',(-41.2914458636761,38.7889049517819,40.3130982808877));
#32322=CARTESIAN_POINT('Ctrl Pts',(-41.3224741081885,38.8682188845166,40.3429901602992));
#32323=CARTESIAN_POINT('Ctrl Pts',(-41.3520340619235,38.9486984418346,40.371314031491));
#32324=CARTESIAN_POINT('Ctrl Pts',(-41.3800824127475,39.0302257654376,40.3980283925727));
#32325=CARTESIAN_POINT('Ctrl Pts',(-41.4081307635715,39.1117530890405,40.4247427536544));
#32326=CARTESIAN_POINT('Ctrl Pts',(-41.4346675034574,39.1943281556243,40.4498475969801));
#32327=CARTESIAN_POINT('Ctrl Pts',(-41.4596537451974,39.2778300378728,40.4733061322202));
#32328=CARTESIAN_POINT('Ctrl Pts',(-41.4846399869374,39.3613319201213,40.4967646674603));
#32329=CARTESIAN_POINT('Ctrl Pts',(-41.5080757233786,39.4457605941657,40.5185768878985));
#32330=CARTESIAN_POINT('Ctrl Pts',(-41.5299266061116,39.5309924175345,40.5387108225031));
#32331=CARTESIAN_POINT('Ctrl Pts',(-41.5517774888446,39.6162242409034,40.5588447571076));
#32332=CARTESIAN_POINT('Ctrl Pts',(-41.5720435116116,39.7022591892331,40.5773004001115));
#32333=CARTESIAN_POINT('Ctrl Pts',(-41.5906949654003,39.7889712667059,40.5940506934234));
#32334=CARTESIAN_POINT('Ctrl Pts',(-41.6093464191891,39.8756833441786,40.6108009867352));
#32335=CARTESIAN_POINT('Ctrl Pts',(-41.6263832986553,39.9630725260074,40.6258459255541));
#32336=CARTESIAN_POINT('Ctrl Pts',(-41.6417806212144,40.051010831727,40.6391634440034));
#32337=CARTESIAN_POINT('Ctrl Pts',(-41.6571779437735,40.1389491374466,40.6524809624527));
#32338=CARTESIAN_POINT('Ctrl Pts',(-41.6709357050106,40.2274365419188,40.6640710567117));
#32339=CARTESIAN_POINT('Ctrl Pts',(-41.6830337219766,40.3163434545426,40.6739167177927));
#32340=CARTESIAN_POINT('Ctrl Pts',(-41.6951317389425,40.4052503671663,40.6837623788737));
#32341=CARTESIAN_POINT('Ctrl Pts',(-41.7055700081645,40.4945767625257,40.6918636039474));
#32342=CARTESIAN_POINT('Ctrl Pts',(-41.7143332054998,40.5841918191118,40.6982084907992));
#32343=CARTESIAN_POINT('Ctrl Pts',(-41.7230964028351,40.6738068756978,40.7045533776511));
#32344=CARTESIAN_POINT('Ctrl Pts',(-41.730184525763,40.7637105678913,40.7091419244515));
#32345=CARTESIAN_POINT('Ctrl Pts',(-41.7355871539075,40.8537712261132,40.711967370708));
#32346=CARTESIAN_POINT('Ctrl Pts',(-41.7409945835981,40.9439119250834,40.7147953280591));
#32347=CARTESIAN_POINT('Ctrl Pts',(-41.7447135196681,41.0342098434169,40.7158570487623));
#32348=CARTESIAN_POINT('Ctrl Pts',(-41.746738461486,41.1245324961841,40.7151509296908));
#32349=CARTESIAN_POINT('Ctrl Pts',(-40.4026917455303,37.3333248863599,39.5103831374403));
#32350=CARTESIAN_POINT('Ctrl Pts',(-40.4523532259874,37.392012397429,39.5603800219979));
#32351=CARTESIAN_POINT('Ctrl Pts',(-40.500927035616,37.4526383953682,39.6091818138752));
#32352=CARTESIAN_POINT('Ctrl Pts',(-40.548339675232,37.5151111442932,39.6567146689183));
#32353=CARTESIAN_POINT('Ctrl Pts',(-40.595752314848,37.5775838932182,39.7042475239613));
#32354=CARTESIAN_POINT('Ctrl Pts',(-40.6420037699661,37.6419033740425,39.750511427648));
#32355=CARTESIAN_POINT('Ctrl Pts',(-40.6870240554598,37.7079722621093,39.7954363760154));
#32356=CARTESIAN_POINT('Ctrl Pts',(-40.7320443409536,37.7740411501762,39.8403613243828));
#32357=CARTESIAN_POINT('Ctrl Pts',(-40.7758334430686,37.8418594253004,39.8839473037057));
#32358=CARTESIAN_POINT('Ctrl Pts',(-40.8183251025737,37.9113244686443,39.9261283621071));
#32359=CARTESIAN_POINT('Ctrl Pts',(-40.8608167620789,37.9807895119883,39.9683094205084));
#32360=CARTESIAN_POINT('Ctrl Pts',(-40.9020109659924,38.0519013023294,40.0090855451013));
#32361=CARTESIAN_POINT('Ctrl Pts',(-40.9418453815386,38.1245522372661,40.0483950357245));
#32362=CARTESIAN_POINT('Ctrl Pts',(-40.9816797970848,38.1972031722028,40.0877045263477));
#32363=CARTESIAN_POINT('Ctrl Pts',(-41.0201544120938,38.2713932295392,40.1255473709915));
#32364=CARTESIAN_POINT('Ctrl Pts',(-41.0572110089203,38.3470101490115,40.1618663079706));
#32365=CARTESIAN_POINT('Ctrl Pts',(-41.0942676057469,38.4226270684837,40.1981852449497));
#32366=CARTESIAN_POINT('Ctrl Pts',(-41.1299061730698,38.4996708269898,40.2329802631682));
#32367=CARTESIAN_POINT('Ctrl Pts',(-41.1640727845932,38.5780248462043,40.2661987127418));
#32368=CARTESIAN_POINT('Ctrl Pts',(-41.1982393961167,38.6563788654189,40.2994171623154));
#32369=CARTESIAN_POINT('Ctrl Pts',(-41.2309340414024,38.7360431214034,40.3310590330955));
#32370=CARTESIAN_POINT('Ctrl Pts',(-41.2621072487336,38.8168970706418,40.361076446365));
#32371=CARTESIAN_POINT('Ctrl Pts',(-41.2932804560647,38.8977510198801,40.3910938596345));
#32372=CARTESIAN_POINT('Ctrl Pts',(-41.3229322159175,38.9797946376701,40.4194868062228));
#32373=CARTESIAN_POINT('Ctrl Pts',(-41.3510176608998,39.0629037801777,40.4462123235039));
#32374=CARTESIAN_POINT('Ctrl Pts',(-41.3791031058822,39.1460129226852,40.472937840785));
#32375=CARTESIAN_POINT('Ctrl Pts',(-41.4056222274137,39.2301875645192,40.497995920594));
#32376=CARTESIAN_POINT('Ctrl Pts',(-41.4305348982363,39.3153003372986,40.5213486464397));
#32377=CARTESIAN_POINT('Ctrl Pts',(-41.4554475690588,39.400413110078,40.5447013722854));
#32378=CARTESIAN_POINT('Ctrl Pts',(-41.4787537815612,39.4864639877996,40.5663487370333));
#32379=CARTESIAN_POINT('Ctrl Pts',(-41.5004182700804,39.5733227630668,40.5862579850963));
#32380=CARTESIAN_POINT('Ctrl Pts',(-41.5220827585996,39.6601815383338,40.6061672331594));
#32381=CARTESIAN_POINT('Ctrl Pts',(-41.5421055165168,39.7478481846099,40.624338358455));
#32382=CARTESIAN_POINT('Ctrl Pts',(-41.5604562465096,39.8361900496069,40.6407438654482));
#32383=CARTESIAN_POINT('Ctrl Pts',(-41.5788069765024,39.924531914604,40.6571493724415));
#32384=CARTESIAN_POINT('Ctrl Pts',(-41.5954856729644,40.0135489713325,40.6717892561202));
#32385=CARTESIAN_POINT('Ctrl Pts',(-41.6104670986208,40.1031065241387,40.6846413642276));
#32386=CARTESIAN_POINT('Ctrl Pts',(-41.6254485242772,40.1926640769449,40.697493472335));
#32387=CARTESIAN_POINT('Ctrl Pts',(-41.638732674551,40.2827620984677,40.7085578009445));
#32388=CARTESIAN_POINT('Ctrl Pts',(-41.6502994486055,40.3732642573977,40.7178176081302));
#32389=CARTESIAN_POINT('Ctrl Pts',(-41.6618662226601,40.4637664163277,40.7270774153159));
#32390=CARTESIAN_POINT('Ctrl Pts',(-41.6717156169618,40.5546726850152,40.7345326982488));
#32391=CARTESIAN_POINT('Ctrl Pts',(-41.6798327279554,40.6458455091562,40.7401721760098));
#32392=CARTESIAN_POINT('Ctrl Pts',(-41.687949838949,40.7370183332971,40.7458116537709));
#32393=CARTESIAN_POINT('Ctrl Pts',(-41.6943346641547,40.8284576850369,40.7496353246372));
#32394=CARTESIAN_POINT('Ctrl Pts',(-41.6989775424105,40.92002520344,40.7516374028428));
#32395=CARTESIAN_POINT('Ctrl Pts',(-41.7036245469903,41.0116741018023,40.7536412603807));
#32396=CARTESIAN_POINT('Ctrl Pts',(-41.7065265055382,41.1034513667184,40.7538202853523));
#32397=CARTESIAN_POINT('Ctrl Pts',(-41.7076790168147,41.1952178791612,40.7521742039289));
#32398=CARTESIAN_POINT('Ctrl Pts',(-40.3238273833491,37.3356711120808,39.5859643834861));
#32399=CARTESIAN_POINT('Ctrl Pts',(-40.3750334619085,37.3962127790296,39.6375630543615));
#32400=CARTESIAN_POINT('Ctrl Pts',(-40.4250831507418,37.4588154040666,39.6878911268195));
#32401=CARTESIAN_POINT('Ctrl Pts',(-40.4738960771041,37.5233784686756,39.736867785101));
#32402=CARTESIAN_POINT('Ctrl Pts',(-40.5227090034662,37.5879415332848,39.7858444433824));
#32403=CARTESIAN_POINT('Ctrl Pts',(-40.5702851506146,37.65446501533,39.83346967069));
#32404=CARTESIAN_POINT('Ctrl Pts',(-40.6165481104883,37.722842110628,39.8796669835082));
#32405=CARTESIAN_POINT('Ctrl Pts',(-40.6628110703621,37.7912192059259,39.9258642963265));
#32406=CARTESIAN_POINT('Ctrl Pts',(-40.7077608270898,37.8614498910366,39.9706336788078));
#32407=CARTESIAN_POINT('Ctrl Pts',(-40.7513251819515,37.9334214179972,40.0139032245691));
#32408=CARTESIAN_POINT('Ctrl Pts',(-40.7948895368132,38.0053929449577,40.0571727703304));
#32409=CARTESIAN_POINT('Ctrl Pts',(-40.8370684748596,38.0791052890989,40.0989424645244));
#32410=CARTESIAN_POINT('Ctrl Pts',(-40.8777942379143,38.1544401195702,40.1391452081597));
#32411=CARTESIAN_POINT('Ctrl Pts',(-40.9185200009691,38.2297749500413,40.1793479517951));
#32412=CARTESIAN_POINT('Ctrl Pts',(-40.9577925750527,38.3067322410228,40.2179837310723));
#32413=CARTESIAN_POINT('Ctrl Pts',(-40.9955488595443,38.3851884575184,40.2549904692869));
#32414=CARTESIAN_POINT('Ctrl Pts',(-41.0333051440358,38.4636446740141,40.2919972075016));
#32415=CARTESIAN_POINT('Ctrl Pts',(-41.06954512597,38.5435997891364,40.3273748919461));
#32416=CARTESIAN_POINT('Ctrl Pts',(-41.1042105644085,38.6249254591294,40.361066667048));
#32417=CARTESIAN_POINT('Ctrl Pts',(-41.1388760028468,38.7062511291223,40.39475844215));
#32418=CARTESIAN_POINT('Ctrl Pts',(-41.1719668858801,38.7889473261161,40.4267642963341));
#32419=CARTESIAN_POINT('Ctrl Pts',(-41.2034300188486,38.8728813083616,40.4570327773197));
#32420=CARTESIAN_POINT('Ctrl Pts',(-41.2348931518171,38.9568152906071,40.4873012583052));
#32421=CARTESIAN_POINT('Ctrl Pts',(-41.2647285239056,39.041987029341,40.5158323556863));
#32422=CARTESIAN_POINT('Ctrl Pts',(-41.2928881572047,39.1282598096577,40.5425801853663));
#32423=CARTESIAN_POINT('Ctrl Pts',(-41.3210477905038,39.2145325899743,40.5693280150463));
#32424=CARTESIAN_POINT('Ctrl Pts',(-41.3475316753265,39.3019063823089,40.5942925678218));
#32425=CARTESIAN_POINT('Ctrl Pts',(-41.3722972043141,39.3902409361501,40.6174336748788));
#32426=CARTESIAN_POINT('Ctrl Pts',(-41.3970627333016,39.4785754899914,40.6405747819357));
#32427=CARTESIAN_POINT('Ctrl Pts',(-41.4201098979263,39.5678707750675,40.6618924353029));
#32428=CARTESIAN_POINT('Ctrl Pts',(-41.4414015980179,39.6579834541311,40.6813523102829));
#32429=CARTESIAN_POINT('Ctrl Pts',(-41.4626932981095,39.7480961331947,40.7008121852628));
#32430=CARTESIAN_POINT('Ctrl Pts',(-41.482229526327,39.8390261753633,40.7184142751419));
#32431=CARTESIAN_POINT('Ctrl Pts',(-41.499978808728,39.930627615409,40.734130209498));
#32432=CARTESIAN_POINT('Ctrl Pts',(-41.517728091129,40.0222290554547,40.7498461438541));
#32433=CARTESIAN_POINT('Ctrl Pts',(-41.5336904215826,40.1145018619828,40.7636759172525));
#32434=CARTESIAN_POINT('Ctrl Pts',(-41.5478400534335,40.2072979089622,40.775597204676));
#32435=CARTESIAN_POINT('Ctrl Pts',(-41.5619896852844,40.3000939559416,40.7875184920995));
#32436=CARTESIAN_POINT('Ctrl Pts',(-41.5743266136316,40.3934132115655,40.7975312894101));
#32437=CARTESIAN_POINT('Ctrl Pts',(-41.5848309018635,40.4871058631079,40.8056193888052));
#32438=CARTESIAN_POINT('Ctrl Pts',(-41.5953351900953,40.5807985146504,40.8137074882003));
#32439=CARTESIAN_POINT('Ctrl Pts',(-41.6040068345563,40.6748645299942,40.8198708868516));
#32440=CARTESIAN_POINT('Ctrl Pts',(-41.6108317728666,40.769152889245,40.824099546431));
#32441=CARTESIAN_POINT('Ctrl Pts',(-41.6176567111769,40.8634412484956,40.8283282060105));
#32442=CARTESIAN_POINT('Ctrl Pts',(-41.6226349409381,40.9579519193281,40.8306221250085));
#32443=CARTESIAN_POINT('Ctrl Pts',(-41.6257583194165,41.0525331580936,40.8309774671124));
#32444=CARTESIAN_POINT('Ctrl Pts',(-41.6288844737746,41.1471984552401,40.831333125024));
#32445=CARTESIAN_POINT('Ctrl Pts',(-41.6301524772784,41.2419344133214,40.8297467585323));
#32446=CARTESIAN_POINT('Ctrl Pts',(-41.6295601274722,41.3365886451155,40.8262207524052));
#32447=CARTESIAN_POINT('Ctrl Pts',(-40.2449312129505,37.3379802045158,39.6615143463265));
#32448=CARTESIAN_POINT('Ctrl Pts',(-40.2976328145503,37.4003117501095,39.7146552060781));
#32449=CARTESIAN_POINT('Ctrl Pts',(-40.3491084470698,37.4648282580176,39.7664490162522));
#32450=CARTESIAN_POINT('Ctrl Pts',(-40.3992704605161,37.5314198852677,39.8168075871395));
#32451=CARTESIAN_POINT('Ctrl Pts',(-40.4494324739624,37.5980115125179,39.8671661580268));
#32452=CARTESIAN_POINT('Ctrl Pts',(-40.4982808489931,37.6666782334438,39.9160894702099));
#32453=CARTESIAN_POINT('Ctrl Pts',(-40.5457324008023,37.7373031500135,39.9634942126056));
#32454=CARTESIAN_POINT('Ctrl Pts',(-40.5931839526115,37.8079280665833,40.0108989550013));
#32455=CARTESIAN_POINT('Ctrl Pts',(-40.6392386628975,37.8805111515807,40.0567851093263));
#32456=CARTESIAN_POINT('Ctrl Pts',(-40.6838180944329,37.9549288486176,40.1010745259389));
#32457=CARTESIAN_POINT('Ctrl Pts',(-40.7283975259683,38.0293465456543,40.1453639425515));
#32458=CARTESIAN_POINT('Ctrl Pts',(-40.7715016615542,38.1055988260566,40.1880566043646));
#32459=CARTESIAN_POINT('Ctrl Pts',(-40.8130570778548,38.1835558943449,40.2290797885122));
#32460=CARTESIAN_POINT('Ctrl Pts',(-40.8546124941553,38.2615129626333,40.2701029726598));
#32461=CARTESIAN_POINT('Ctrl Pts',(-40.8946191751323,38.341174788773,40.3094566633089));
#32462=CARTESIAN_POINT('Ctrl Pts',(-40.9330089606741,38.4224057786039,40.3470738113249));
#32463=CARTESIAN_POINT('Ctrl Pts',(-40.9713987462159,38.5036367684348,40.3846909593409));
#32464=CARTESIAN_POINT('Ctrl Pts',(-41.0081716214994,38.5864368906626,40.4205715501982));
#32465=CARTESIAN_POINT('Ctrl Pts',(-41.0432649211462,38.6706652125133,40.4546544362353));
#32466=CARTESIAN_POINT('Ctrl Pts',(-41.078358220793,38.7548935343639,40.4887373222725));
#32467=CARTESIAN_POINT('Ctrl Pts',(-41.1117719312452,38.8405500233895,40.5210224903204));
#32468=CARTESIAN_POINT('Ctrl Pts',(-41.1434490947603,38.9274888863699,40.5514549019477));
#32469=CARTESIAN_POINT('Ctrl Pts',(-41.1751262582754,39.0144277493503,40.581887313575));
#32470=CARTESIAN_POINT('Ctrl Pts',(-41.2050668626066,39.1026489527938,40.6104669570138));
#32471=CARTESIAN_POINT('Ctrl Pts',(-41.2332198512222,39.1920023376887,40.6371450901319));
#32472=CARTESIAN_POINT('Ctrl Pts',(-41.2613728398378,39.2813557225836,40.6638232232499));
#32473=CARTESIAN_POINT('Ctrl Pts',(-41.2877382018437,39.3718412545073,40.6885998357202));
#32474=CARTESIAN_POINT('Ctrl Pts',(-41.3122709555114,39.4633049181251,40.7114326474576));
#32475=CARTESIAN_POINT('Ctrl Pts',(-41.3368037091791,39.5547685817429,40.7342654591949));
#32476=CARTESIAN_POINT('Ctrl Pts',(-41.359503845004,39.6472103418177,40.7551544613484));
#32477=CARTESIAN_POINT('Ctrl Pts',(-41.3803326090827,39.7404728492527,40.7740639797447));
#32478=CARTESIAN_POINT('Ctrl Pts',(-41.4011613731614,39.8337353566877,40.792973498141));
#32479=CARTESIAN_POINT('Ctrl Pts',(-41.4201187574111,39.9278185755504,40.8099035254352));
#32480=CARTESIAN_POINT('Ctrl Pts',(-41.4371723676855,40.0225623568698,40.8248251148608));
#32481=CARTESIAN_POINT('Ctrl Pts',(-41.4542259779599,40.1173061381893,40.8397467042862));
#32482=CARTESIAN_POINT('Ctrl Pts',(-41.4693758076255,40.212710445459,40.8526598500291));
#32483=CARTESIAN_POINT('Ctrl Pts',(-41.4825959326887,40.3086128732442,40.8635424314407));
#32484=CARTESIAN_POINT('Ctrl Pts',(-41.4958160577518,40.4045153010295,40.8744250128523));
#32485=CARTESIAN_POINT('Ctrl Pts',(-41.5071064730508,40.5009158123731,40.8832770256696));
#32486=CARTESIAN_POINT('Ctrl Pts',(-41.5164478132281,40.5976502964727,40.8900832509554));
#32487=CARTESIAN_POINT('Ctrl Pts',(-41.5257891534055,40.6943847805722,40.8968894762412));
#32488=CARTESIAN_POINT('Ctrl Pts',(-41.5331814147889,40.7914532001451,40.9016499112979));
#32489=CARTESIAN_POINT('Ctrl Pts',(-41.5386118569276,40.8886902959407,40.9043562911171));
#32490=CARTESIAN_POINT('Ctrl Pts',(-41.5440422990664,40.9859273917364,40.9070626709362));
#32491=CARTESIAN_POINT('Ctrl Pts',(-41.54751091979,41.0833331262726,40.9077149943948));
#32492=CARTESIAN_POINT('Ctrl Pts',(-41.5490116473865,41.1807416527115,40.9063119790764));
#32493=CARTESIAN_POINT('Ctrl Pts',(-41.5505137087437,41.2782367502626,40.9049077168384));
#32494=CARTESIAN_POINT('Ctrl Pts',(-41.550044376856,41.375734607059,40.9014444613216));
#32495=CARTESIAN_POINT('Ctrl Pts',(-41.5476042716421,41.4730689089368,40.8959279329355));
#32496=CARTESIAN_POINT('Ctrl Pts',(-40.166020457705,37.3402722704297,39.7370499650508));
#32497=CARTESIAN_POINT('Ctrl Pts',(-40.2201818127886,37.4043453509955,39.7916871518576));
#32498=CARTESIAN_POINT('Ctrl Pts',(-40.2730467145036,37.4707290102875,39.8448998436378));
#32499=CARTESIAN_POINT('Ctrl Pts',(-40.3245198289288,37.539303535333,39.8965920792831));
#32500=CARTESIAN_POINT('Ctrl Pts',(-40.375992943354,37.6078780603784,39.9482843149283));
#32501=CARTESIAN_POINT('Ctrl Pts',(-40.4260742481497,37.6786434214157,39.998456072004));
#32502=CARTESIAN_POINT('Ctrl Pts',(-40.4746734291945,37.7514720037299,40.0470168732713));
#32503=CARTESIAN_POINT('Ctrl Pts',(-40.5232726102392,37.8243005860441,40.0955776745386));
#32504=CARTESIAN_POINT('Ctrl Pts',(-40.5703896464407,37.8991923580274,40.1425274989219));
#32505=CARTESIAN_POINT('Ctrl Pts',(-40.615939569291,37.9760122636019,40.1877816794548));
#32506=CARTESIAN_POINT('Ctrl Pts',(-40.6614894921413,38.0528321691764,40.2330358599877));
#32507=CARTESIAN_POINT('Ctrl Pts',(-40.7054722818716,38.1315801750017,40.2765943770297));
#32508=CARTESIAN_POINT('Ctrl Pts',(-40.7478086221175,38.2121142708607,40.3183786793286));
#32509=CARTESIAN_POINT('Ctrl Pts',(-40.7901449623634,38.2926483667197,40.3601629816274));
#32510=CARTESIAN_POINT('Ctrl Pts',(-40.8308348347507,38.3749685176602,40.4001730510485));
#32511=CARTESIAN_POINT('Ctrl Pts',(-40.8698048611974,38.4589262716369,40.4383367354326));
#32512=CARTESIAN_POINT('Ctrl Pts',(-40.9087748876443,38.5428840256135,40.4765004198168));
#32513=CARTESIAN_POINT('Ctrl Pts',(-40.9460250512374,38.6284793461884,40.5128177026007));
#32514=CARTESIAN_POINT('Ctrl Pts',(-40.9814881768939,38.7155578750389,40.5472230910122));
#32515=CARTESIAN_POINT('Ctrl Pts',(-41.0169513025503,38.8026364038895,40.5816284794236));
#32516=CARTESIAN_POINT('Ctrl Pts',(-41.050627374879,38.8911981032232,40.6141219585304));
#32517=CARTESIAN_POINT('Ctrl Pts',(-41.0824556641344,38.9810832652986,40.6446449312166));
#32518=CARTESIAN_POINT('Ctrl Pts',(-41.1142839533898,39.070968427374,40.6751679039028));
#32519=CARTESIAN_POINT('Ctrl Pts',(-41.1442644457583,39.1621770131804,40.7037203569213));
#32520=CARTESIAN_POINT('Ctrl Pts',(-41.1723430759186,39.2545445417134,40.7302508002056));
#32521=CARTESIAN_POINT('Ctrl Pts',(-41.2004217060789,39.3469120702464,40.7567812434898));
#32522=CARTESIAN_POINT('Ctrl Pts',(-41.2265984618448,39.4404385014183,40.7812896655255));
#32523=CARTESIAN_POINT('Ctrl Pts',(-41.2508261373634,39.5349551743379,40.8037318690495));
#32524=CARTESIAN_POINT('Ctrl Pts',(-41.275053812882,39.6294718472575,40.8261740725734));
#32525=CARTESIAN_POINT('Ctrl Pts',(-41.2973323976383,39.7249787209044,40.8465500478457));
#32526=CARTESIAN_POINT('Ctrl Pts',(-41.3176217155464,39.8213035629566,40.8648230498508));
#32527=CARTESIAN_POINT('Ctrl Pts',(-41.3379110334544,39.9176284050089,40.883096051856));
#32528=CARTESIAN_POINT('Ctrl Pts',(-41.3562110757085,40.014771173661,40.8992660726636));
#32529=CARTESIAN_POINT('Ctrl Pts',(-41.3724888409272,40.1125566865002,40.9133039520663));
#32530=CARTESIAN_POINT('Ctrl Pts',(-41.3887666061459,40.2103421993392,40.927341831469));
#32531=CARTESIAN_POINT('Ctrl Pts',(-41.4030220872645,40.3087704139258,40.9392475633744));
#32532=CARTESIAN_POINT('Ctrl Pts',(-41.415229576661,40.407663829738,40.9489996775807));
#32533=CARTESIAN_POINT('Ctrl Pts',(-41.4274370660576,40.50655724555,40.958751791787));
#32534=CARTESIAN_POINT('Ctrl Pts',(-41.437596558434,40.6059158196674,40.9663502840617));
#32535=CARTESIAN_POINT('Ctrl Pts',(-41.4456897326694,40.7055603738042,40.9717814516636));
#32536=CARTESIAN_POINT('Ctrl Pts',(-41.4537829069049,40.8052049279409,40.9772126192656));
#32537=CARTESIAN_POINT('Ctrl Pts',(-41.459809759487,40.9051354188509,40.9804764598378));
#32538=CARTESIAN_POINT('Ctrl Pts',(-41.4637594218909,41.0051716368821,40.981567087533));
#32539=CARTESIAN_POINT('Ctrl Pts',(-41.467709084295,41.1052078549132,40.9826577152283));
#32540=CARTESIAN_POINT('Ctrl Pts',(-41.4695815548068,41.2053497566493,40.9815751295735));
#32541=CARTESIAN_POINT('Ctrl Pts',(-41.4693734567066,41.3054167511905,40.9783212828493));
#32542=CARTESIAN_POINT('Ctrl Pts',(-41.4691651736608,41.4055726795378,40.9750645442929));
#32543=CARTESIAN_POINT('Ctrl Pts',(-41.46687262227,41.5056535239781,40.9696326849821));
#32544=CARTESIAN_POINT('Ctrl Pts',(-41.4624999408153,41.6054784826541,40.9620355143906));
#32545=CARTESIAN_POINT('Ctrl Pts',(-40.0871097024595,37.3425643363436,39.8125855837751));
#32546=CARTESIAN_POINT('Ctrl Pts',(-40.1427308110269,37.4083789518815,39.868719097637));
#32547=CARTESIAN_POINT('Ctrl Pts',(-40.1969849819375,37.4766297625575,39.9233506710234));
#32548=CARTESIAN_POINT('Ctrl Pts',(-40.2497691973415,37.5471871853983,39.9763765714266));
#32549=CARTESIAN_POINT('Ctrl Pts',(-40.3025534127456,37.617744608239,40.0294024718299));
#32550=CARTESIAN_POINT('Ctrl Pts',(-40.3538676473064,37.6906086093875,40.0808226737981));
#32551=CARTESIAN_POINT('Ctrl Pts',(-40.4036144575867,37.7656408574462,40.130539533937));
#32552=CARTESIAN_POINT('Ctrl Pts',(-40.453361267867,37.8406731055049,40.1802563940759));
#32553=CARTESIAN_POINT('Ctrl Pts',(-40.501540629984,37.9178735644741,40.2282698885175));
#32554=CARTESIAN_POINT('Ctrl Pts',(-40.5480610441492,37.9970956785862,40.2744888329708));
#32555=CARTESIAN_POINT('Ctrl Pts',(-40.5945814583144,38.0763177926983,40.320707777424));
#32556=CARTESIAN_POINT('Ctrl Pts',(-40.6394429021891,38.1575615239468,40.365132149695));
#32557=CARTESIAN_POINT('Ctrl Pts',(-40.6825601663803,38.2406726473765,40.407677570145));
#32558=CARTESIAN_POINT('Ctrl Pts',(-40.7256774305715,38.3237837708061,40.450222990595));
#32559=CARTESIAN_POINT('Ctrl Pts',(-40.767050494369,38.4087622465473,40.4908894387881));
#32560=CARTESIAN_POINT('Ctrl Pts',(-40.8066007617208,38.4954467646698,40.5295996595404));
#32561=CARTESIAN_POINT('Ctrl Pts',(-40.8461510290726,38.5821312827923,40.5683098802926));
#32562=CARTESIAN_POINT('Ctrl Pts',(-40.8838784809754,38.6705218017141,40.6050638550033));
#32563=CARTESIAN_POINT('Ctrl Pts',(-40.9197114326415,38.7604505375645,40.639791745789));
#32564=CARTESIAN_POINT('Ctrl Pts',(-40.9555443843077,38.850379273415,40.6745196365747));
#32565=CARTESIAN_POINT('Ctrl Pts',(-40.9894828185128,38.941846183057,40.7072214267404));
#32566=CARTESIAN_POINT('Ctrl Pts',(-41.0214622335085,39.0346776442273,40.7378349604855));
#32567=CARTESIAN_POINT('Ctrl Pts',(-41.0534416485042,39.1275091053977,40.7684484942305));
#32568=CARTESIAN_POINT('Ctrl Pts',(-41.08346202891,39.2217050735669,40.7969737568287));
#32569=CARTESIAN_POINT('Ctrl Pts',(-41.111466300615,39.3170867457382,40.8233565102792));
#32570=CARTESIAN_POINT('Ctrl Pts',(-41.1394705723201,39.4124684179094,40.8497392637297));
#32571=CARTESIAN_POINT('Ctrl Pts',(-41.1654587218459,39.5090357483292,40.8739794953308));
#32572=CARTESIAN_POINT('Ctrl Pts',(-41.1893813192154,39.6066054305506,40.8960310906414));
#32573=CARTESIAN_POINT('Ctrl Pts',(-41.2133039165849,39.7041751127721,40.918082685952));
#32574=CARTESIAN_POINT('Ctrl Pts',(-41.2351609502726,39.8027470999911,40.9379456343429));
#32575=CARTESIAN_POINT('Ctrl Pts',(-41.2549108220101,39.9021342766605,40.955582119957));
#32576=CARTESIAN_POINT('Ctrl Pts',(-41.2746606937475,40.00152145333,40.973218605571));
#32577=CARTESIAN_POINT('Ctrl Pts',(-41.292303394006,40.1017237717717,40.9886286198919));
#32578=CARTESIAN_POINT('Ctrl Pts',(-41.3078053141689,40.2025510161305,41.0017827892718));
#32579=CARTESIAN_POINT('Ctrl Pts',(-41.3233072343318,40.3033782604891,41.0149369586518));
#32580=CARTESIAN_POINT('Ctrl Pts',(-41.3366683669035,40.4048303823926,41.0258352767197));
#32581=CARTESIAN_POINT('Ctrl Pts',(-41.3478632206334,40.5067147862316,41.0344569237207));
#32582=CARTESIAN_POINT('Ctrl Pts',(-41.3590580743634,40.6085991900705,41.0430785707216));
#32583=CARTESIAN_POINT('Ctrl Pts',(-41.3680866438171,40.7109158269618,41.0494235424537));
#32584=CARTESIAN_POINT('Ctrl Pts',(-41.3749316521107,40.8134704511357,41.0534796523719));
#32585=CARTESIAN_POINT('Ctrl Pts',(-41.3817766604043,40.9160250753096,41.05753576229));
#32586=CARTESIAN_POINT('Ctrl Pts',(-41.386438104185,41.0188176375568,41.0593030083776));
#32587=CARTESIAN_POINT('Ctrl Pts',(-41.3889069868543,41.1216529778233,41.058777883949));
#32588=CARTESIAN_POINT('Ctrl Pts',(-41.3913758695236,41.2244883180898,41.0582527595205));
#32589=CARTESIAN_POINT('Ctrl Pts',(-41.3916521898236,41.3273663870258,41.0554352647522));
#32590=CARTESIAN_POINT('Ctrl Pts',(-41.3897352660267,41.4300918496695,41.0503305866223));
#32591=CARTESIAN_POINT('Ctrl Pts',(-41.3878166385779,41.5329086088132,41.0452213717473));
#32592=CARTESIAN_POINT('Ctrl Pts',(-41.383700867684,41.6355724408973,41.0378209086425));
#32593=CARTESIAN_POINT('Ctrl Pts',(-41.3773956099884,41.7378880563715,41.0281430958457));
#32594=CARTESIAN_POINT('Ctrl Pts',(-40.0081842027545,37.3448391894026,39.8881067014052));
#32595=CARTESIAN_POINT('Ctrl Pts',(-40.065229152976,37.41234682335,39.9456905295488));
#32596=CARTESIAN_POINT('Ctrl Pts',(-40.1208357762505,37.4824178811549,40.0016939774043));
#32597=CARTESIAN_POINT('Ctrl Pts',(-40.1748929640454,37.5549123641953,40.0560051435073));
#32598=CARTESIAN_POINT('Ctrl Pts',(-40.2289501518402,37.6274068472357,40.1103163096102));
#32599=CARTESIAN_POINT('Ctrl Pts',(-40.2814578754243,37.7023247169942,40.1629351650944));
#32600=CARTESIAN_POINT('Ctrl Pts',(-40.3323112093966,37.7795163024568,40.2137565617103));
#32601=CARTESIAN_POINT('Ctrl Pts',(-40.3831645433688,37.8567078879194,40.2645779583263));
#32602=CARTESIAN_POINT('Ctrl Pts',(-40.4323634606956,37.9361731480789,40.3136018690566));
#32603=CARTESIAN_POINT('Ctrl Pts',(-40.4798096374514,38.0177533361164,40.3607303181027));
#32604=CARTESIAN_POINT('Ctrl Pts',(-40.5272558142073,38.0993335241538,40.4078587671488));
#32605=CARTESIAN_POINT('Ctrl Pts',(-40.5729492251636,38.1830285967346,40.4530917294489));
#32606=CARTESIAN_POINT('Ctrl Pts',(-40.6167985399401,38.2686713639595,40.4963387923452));
#32607=CARTESIAN_POINT('Ctrl Pts',(-40.6606478547166,38.3543141311843,40.5395858552415));
#32608=CARTESIAN_POINT('Ctrl Pts',(-40.7026530499896,38.4419045475642,40.580846995729));
#32609=CARTESIAN_POINT('Ctrl Pts',(-40.7427301531617,38.5312676464628,40.620039724875));
#32610=CARTESIAN_POINT('Ctrl Pts',(-40.7828072563337,38.6206307453612,40.659232454021));
#32611=CARTESIAN_POINT('Ctrl Pts',(-40.8209562460789,38.7117664793156,40.6963567509687));
#32612=CARTESIAN_POINT('Ctrl Pts',(-40.8571008425368,38.8044928022744,40.7313383795681));
#32613=CARTESIAN_POINT('Ctrl Pts',(-40.8932454389946,38.8972191252332,40.7663200081675));
#32614=CARTESIAN_POINT('Ctrl Pts',(-40.9273856229222,38.991535987948,40.7991589497917));
#32615=CARTESIAN_POINT('Ctrl Pts',(-40.9594531115379,39.0872549904745,40.8297895172827));
#32616=CARTESIAN_POINT('Ctrl Pts',(-40.9915206001535,39.182973993001,40.8604200847737));
#32617=CARTESIAN_POINT('Ctrl Pts',(-41.0215153763742,39.2800950845001,40.8888422618082));
#32618=CARTESIAN_POINT('Ctrl Pts',(-41.0493774270134,39.3784242619804,40.9149991724108));
#32619=CARTESIAN_POINT('Ctrl Pts',(-41.0772394776526,39.4767534394608,40.9411560830135));
#32620=CARTESIAN_POINT('Ctrl Pts',(-41.102968787854,39.5762906506965,40.9650477132315));
#32621=CARTESIAN_POINT('Ctrl Pts',(-41.126513853637,39.676837062824,40.9866262253897));
#32622=CARTESIAN_POINT('Ctrl Pts',(-41.15005891942,39.7773834749515,41.0082047375478));
#32623=CARTESIAN_POINT('Ctrl Pts',(-41.1714197282146,39.8789390345654,41.0274701201193));
#32624=CARTESIAN_POINT('Ctrl Pts',(-41.1905534909882,39.9813008713815,41.0443837648881));
#32625=CARTESIAN_POINT('Ctrl Pts',(-41.2096872537618,40.0836627081975,41.061297409657));
#32626=CARTESIAN_POINT('Ctrl Pts',(-41.2265939602815,40.1868307678413,41.0758593075667));
#32627=CARTESIAN_POINT('Ctrl Pts',(-41.2412397075264,40.290598951167,41.0880402342802));
#32628=CARTESIAN_POINT('Ctrl Pts',(-41.2558854547714,40.3943671344927,41.1002211609936));
#32629=CARTESIAN_POINT('Ctrl Pts',(-41.268270234886,40.4987353863741,41.1100211099617));
#32630=CARTESIAN_POINT('Ctrl Pts',(-41.2783691665588,40.6034952002683,41.1174203578003));
#32631=CARTESIAN_POINT('Ctrl Pts',(-41.2884680982315,40.7082550141624,41.124819605639));
#32632=CARTESIAN_POINT('Ctrl Pts',(-41.2962811760157,40.8134063344103,41.1298181483325));
#32633=CARTESIAN_POINT('Ctrl Pts',(-41.3017926401003,40.9187390781749,41.1324058427085));
#32634=CARTESIAN_POINT('Ctrl Pts',(-41.3073041041849,41.0240718219395,41.1349935370845));
#32635=CARTESIAN_POINT('Ctrl Pts',(-41.3105139515539,41.12958593325,41.1351703816769));
#32636=CARTESIAN_POINT('Ctrl Pts',(-41.3114156073819,41.235070590414,41.1329358546501));
#32637=CARTESIAN_POINT('Ctrl Pts',(-41.31231726321,41.3405552475781,41.1307013276233));
#32638=CARTESIAN_POINT('Ctrl Pts',(-41.3109107269242,41.4460103945356,41.1260554300668));
#32639=CARTESIAN_POINT('Ctrl Pts',(-41.3071986356094,41.5512253111845,41.119007264307));
#32640=CARTESIAN_POINT('Ctrl Pts',(-41.3034832452007,41.6565337368175,41.1119528345416));
#32641=CARTESIAN_POINT('Ctrl Pts',(-41.2974582017289,41.7616014489183,41.1024918683256));
#32642=CARTESIAN_POINT('Ctrl Pts',(-41.2891353760335,41.8662181092778,41.090643106539));
#32643=CARTESIAN_POINT('Ctrl Pts',(-39.929257160475,37.3471122416422,39.9636263019219));
#32644=CARTESIAN_POINT('Ctrl Pts',(-39.9876994389499,37.4162754036955,40.0226237631534));
#32645=CARTESIAN_POINT('Ctrl Pts',(-40.0446310452863,37.4881309212478,40.0799613539993));
#32646=CARTESIAN_POINT('Ctrl Pts',(-40.0999323645469,37.5625278237963,40.135518606537));
#32647=CARTESIAN_POINT('Ctrl Pts',(-40.1552336838076,37.6369247263448,40.1910758590747));
#32648=CARTESIAN_POINT('Ctrl Pts',(-40.2089046834089,37.7138629700548,40.24485274057));
#32649=CARTESIAN_POINT('Ctrl Pts',(-40.260832599042,37.7931809054704,40.2967362642528));
#32650=CARTESIAN_POINT('Ctrl Pts',(-40.3127605146749,37.8724988408859,40.3486197879357));
#32651=CARTESIAN_POINT('Ctrl Pts',(-40.3629453157436,37.9541964212729,40.3986099232363));
#32652=CARTESIAN_POINT('Ctrl Pts',(-40.4112815625419,38.0381019976722,40.4466016394471));
#32653=CARTESIAN_POINT('Ctrl Pts',(-40.4596178093403,38.1220075740716,40.4945933556579));
#32654=CARTESIAN_POINT('Ctrl Pts',(-40.5061054733888,38.2081210970459,40.5405866245016));
#32655=CARTESIAN_POINT('Ctrl Pts',(-40.550646882772,38.2962616396148,40.5844848128026));
#32656=CARTESIAN_POINT('Ctrl Pts',(-40.5951882921553,38.3844021821838,40.6283830011036));
#32657=CARTESIAN_POINT('Ctrl Pts',(-40.6377834206293,38.4745696924153,40.6701860829973));
#32658=CARTESIAN_POINT('Ctrl Pts',(-40.6783427746084,38.5665747257838,40.7098062290088));
#32659=CARTESIAN_POINT('Ctrl Pts',(-40.7189021285875,38.6585797591524,40.7494263750202));
#32660=CARTESIAN_POINT('Ctrl Pts',(-40.7574256841738,38.7524222614492,40.7868635618058));
#32661=CARTESIAN_POINT('Ctrl Pts',(-40.7938325022725,38.8479050668861,40.8220391327627));
#32662=CARTESIAN_POINT('Ctrl Pts',(-40.8302393203712,38.9433878723231,40.8572147037195));
#32663=CARTESIAN_POINT('Ctrl Pts',(-40.8645293795313,39.0405109246417,40.8901286381222));
#32664=CARTESIAN_POINT('Ctrl Pts',(-40.8966306353554,39.1390701655243,40.9207117828508));
#32665=CARTESIAN_POINT('Ctrl Pts',(-40.9287318911796,39.2376294064068,40.9512949275794));
#32666=CARTESIAN_POINT('Ctrl Pts',(-40.958644324754,39.3376247777812,40.9795472646133));
#32667=CARTESIAN_POINT('Ctrl Pts',(-40.9863050891974,39.4388461865069,41.0054094349843));
#32668=CARTESIAN_POINT('Ctrl Pts',(-41.0139658536407,39.5400675952327,41.0312716053553));
#32669=CARTESIAN_POINT('Ctrl Pts',(-41.0393749326551,39.6425149816702,41.0547435938255));
#32670=CARTESIAN_POINT('Ctrl Pts',(-41.062478941038,39.7459731009211,41.075776085072));
#32671=CARTESIAN_POINT('Ctrl Pts',(-41.0855829494209,39.849431220172,41.0968085763185));
#32672=CARTESIAN_POINT('Ctrl Pts',(-41.1063818735589,39.9539000112797,41.11540155795));
#32673=CARTESIAN_POINT('Ctrl Pts',(-41.124832014316,40.0591599823187,41.131515965579));
#32674=CARTESIAN_POINT('Ctrl Pts',(-41.1432821550731,40.1644199533577,41.147630373208));
#32675=CARTESIAN_POINT('Ctrl Pts',(-41.1593835015786,40.2704710423087,41.1612661973399));
#32676=CARTESIAN_POINT('Ctrl Pts',(-41.1731022244417,40.3770904327933,41.1723947887171));
#32677=CARTESIAN_POINT('Ctrl Pts',(-41.1868209473048,40.4837098232777,41.1835233800944));
#32678=CARTESIAN_POINT('Ctrl Pts',(-41.1981570384424,40.5908974524755,41.19214473216));
#32679=CARTESIAN_POINT('Ctrl Pts',(-41.207086680402,40.6984281161042,41.1982407312062));
#32680=CARTESIAN_POINT('Ctrl Pts',(-41.2160163223617,40.8059587797328,41.2043367302524));
#32681=CARTESIAN_POINT('Ctrl Pts',(-41.2225395098821,40.9138324144353,41.2079073726873));
#32682=CARTESIAN_POINT('Ctrl Pts',(-41.2266425375591,41.0218223746121,41.2089451564889));
#32683=CARTESIAN_POINT('Ctrl Pts',(-41.2307455652362,41.1298123347889,41.2099829402905));
#32684=CARTESIAN_POINT('Ctrl Pts',(-41.2324284306523,41.2379185568123,41.2084878648472));
#32685=CARTESIAN_POINT('Ctrl Pts',(-41.2316875980592,41.34591390641,41.2044630713555));
#32686=CARTESIAN_POINT('Ctrl Pts',(-41.2309467654661,41.4539092560078,41.2004382778638));
#32687=CARTESIAN_POINT('Ctrl Pts',(-41.2277822353002,41.561793669549,41.193883768695));
#32688=CARTESIAN_POINT('Ctrl Pts',(-41.22220065633,41.6693404787875,41.1848133150609));
#32689=CARTESIAN_POINT('Ctrl Pts',(-41.2166141167725,41.7769828694626,41.1757348001277));
#32690=CARTESIAN_POINT('Ctrl Pts',(-41.208606233529,41.8842869920002,41.1641358720405));
#32691=CARTESIAN_POINT('Ctrl Pts',(-41.1981938567826,41.9910269958237,41.1500409391072));
#32692=CARTESIAN_POINT('Ctrl Pts',(-39.8503301181955,37.3493852938817,40.0391459024386));
#32693=CARTESIAN_POINT('Ctrl Pts',(-39.9101697249238,37.4202039840409,40.0995569967581));
#32694=CARTESIAN_POINT('Ctrl Pts',(-39.9684263143221,37.4938439613405,40.1582287305944));
#32695=CARTESIAN_POINT('Ctrl Pts',(-40.0249717650485,37.5701432833972,40.2150320695668));
#32696=CARTESIAN_POINT('Ctrl Pts',(-40.081517215775,37.6464426054539,40.2718354085393));
#32697=CARTESIAN_POINT('Ctrl Pts',(-40.1363514913936,37.7254012231154,40.3267703160456));
#32698=CARTESIAN_POINT('Ctrl Pts',(-40.1893539886873,37.806845508484,40.3797159667953));
#32699=CARTESIAN_POINT('Ctrl Pts',(-40.242356485981,37.8882897938525,40.432661617545));
#32700=CARTESIAN_POINT('Ctrl Pts',(-40.2935271707916,37.9722196944668,40.483617977416));
#32701=CARTESIAN_POINT('Ctrl Pts',(-40.3427534876325,38.0584506592281,40.5324729607915));
#32702=CARTESIAN_POINT('Ctrl Pts',(-40.3919798044733,38.1446816239894,40.581327944167));
#32703=CARTESIAN_POINT('Ctrl Pts',(-40.439261721614,38.2332135973571,40.6280815195542));
#32704=CARTESIAN_POINT('Ctrl Pts',(-40.4844952256039,38.3238519152703,40.67263083326));
#32705=CARTESIAN_POINT('Ctrl Pts',(-40.5297287295939,38.4144902331834,40.7171801469658));
#32706=CARTESIAN_POINT('Ctrl Pts',(-40.572913791269,38.5072348372663,40.7595251702657));
#32707=CARTESIAN_POINT('Ctrl Pts',(-40.6139553960551,38.601881805105,40.7995727331425));
#32708=CARTESIAN_POINT('Ctrl Pts',(-40.6549970008413,38.6965287729436,40.8396202960194));
#32709=CARTESIAN_POINT('Ctrl Pts',(-40.6938951222687,38.7930780435828,40.8773703726429));
#32710=CARTESIAN_POINT('Ctrl Pts',(-40.7305641620082,38.8913173314979,40.9127398859572));
#32711=CARTESIAN_POINT('Ctrl Pts',(-40.7672332017477,38.989556619413,40.9481093992715));
#32712=CARTESIAN_POINT('Ctrl Pts',(-40.8016731361404,39.0894858613354,40.9810983264527));
#32713=CARTESIAN_POINT('Ctrl Pts',(-40.833808159173,39.190885340574,41.0116340484189));
#32714=CARTESIAN_POINT('Ctrl Pts',(-40.8659431822056,39.2922848198126,41.042169770385));
#32715=CARTESIAN_POINT('Ctrl Pts',(-40.8957732731339,39.3951544710623,41.0702522674185));
#32716=CARTESIAN_POINT('Ctrl Pts',(-40.9232327513814,39.4992681110334,41.0958196975579));
#32717=CARTESIAN_POINT('Ctrl Pts',(-40.9506922296289,39.6033817510046,41.1213871276972));
#32718=CARTESIAN_POINT('Ctrl Pts',(-40.9757810774562,39.7087393126439,41.1444394744195));
#32719=CARTESIAN_POINT('Ctrl Pts',(-40.998444028439,39.8151091390182,41.1649259447544));
#32720=CARTESIAN_POINT('Ctrl Pts',(-41.0211069794218,39.9214789653925,41.1854124150893));
#32721=CARTESIAN_POINT('Ctrl Pts',(-41.0413440189032,40.0288609879939,41.2033329957808));
#32722=CARTESIAN_POINT('Ctrl Pts',(-41.0591105376438,40.1370190932559,41.2186481662699));
#32723=CARTESIAN_POINT('Ctrl Pts',(-41.0768770563845,40.2451771985179,41.233963336759));
#32724=CARTESIAN_POINT('Ctrl Pts',(-41.0921730428756,40.3541113167763,41.246673087113));
#32725=CARTESIAN_POINT('Ctrl Pts',(-41.1049647413569,40.4635819144196,41.256749343154));
#32726=CARTESIAN_POINT('Ctrl Pts',(-41.1177564398381,40.5730525120629,41.266825599195));
#32727=CARTESIAN_POINT('Ctrl Pts',(-41.1280438419988,40.6830595185769,41.2742683543583));
#32728=CARTESIAN_POINT('Ctrl Pts',(-41.1358041942453,40.7933610319401,41.279061104612));
#32729=CARTESIAN_POINT('Ctrl Pts',(-41.1435645464919,40.9036625453032,41.2838538548657));
#32730=CARTESIAN_POINT('Ctrl Pts',(-41.1487978437484,41.0142584944603,41.2859965970421));
#32731=CARTESIAN_POINT('Ctrl Pts',(-41.1514924350179,41.1249056710494,41.2854844702693));
#32732=CARTESIAN_POINT('Ctrl Pts',(-41.1541870262875,41.2355528476383,41.2849723434964));
#32733=CARTESIAN_POINT('Ctrl Pts',(-41.1543429097509,41.3462511803745,41.2818053480175));
#32734=CARTESIAN_POINT('Ctrl Pts',(-41.1519595887366,41.4567572224059,41.2759902880609));
#32735=CARTESIAN_POINT('Ctrl Pts',(-41.1495762677222,41.5672632644374,41.2701752281043));
#32736=CARTESIAN_POINT('Ctrl Pts',(-41.1446537436761,41.6775769445624,41.2617121073232));
#32737=CARTESIAN_POINT('Ctrl Pts',(-41.1372026770507,41.7874556463905,41.2506193658148));
#32738=CARTESIAN_POINT('Ctrl Pts',(-41.1297449883444,41.8974320021077,41.2395167657139));
#32739=CARTESIAN_POINT('Ctrl Pts',(-41.1197542653291,42.0069725350821,41.2257798757554));
#32740=CARTESIAN_POINT('Ctrl Pts',(-41.1072523375316,42.1158358823698,41.2094387716753));
#32741=CARTESIAN_POINT('Ctrl Pts',(-39.7714014444761,37.3516564415591,40.1146638984432));
#32742=CARTESIAN_POINT('Ctrl Pts',(-39.8326117898446,37.4240930776539,40.1764518650056));
#32743=CARTESIAN_POINT('Ctrl Pts',(-39.8921658167799,37.4994816354714,40.2364199306906));
#32744=CARTESIAN_POINT('Ctrl Pts',(-39.9499264817845,37.5776486444628,40.2944300970907));
#32745=CARTESIAN_POINT('Ctrl Pts',(-40.0076871467891,37.6558156534542,40.3524402634908));
#32746=CARTESIAN_POINT('Ctrl Pts',(-40.0636544091168,37.7367610584931,40.408492489682));
#32747=CARTESIAN_POINT('Ctrl Pts',(-40.1176994696642,37.8202986143656,40.4624577781161));
#32748=CARTESIAN_POINT('Ctrl Pts',(-40.1717445302117,37.9038361702381,40.5164230665502));
#32749=CARTESIAN_POINT('Ctrl Pts',(-40.223867350847,37.989965818037,40.5683013791495));
#32750=CARTESIAN_POINT('Ctrl Pts',(-40.2739479686196,38.0784893933889,40.6179733119099));
#32751=CARTESIAN_POINT('Ctrl Pts',(-40.3240285863921,38.1670129687408,40.6676452446704));
#32752=CARTESIAN_POINT('Ctrl Pts',(-40.3720669659594,38.2579304092274,40.7151107625352));
#32753=CARTESIAN_POINT('Ctrl Pts',(-40.417952531741,38.3510325415251,40.7602606037133));
#32754=CARTESIAN_POINT('Ctrl Pts',(-40.4638380975226,38.4441346738228,40.8054104448913));
#32755=CARTESIAN_POINT('Ctrl Pts',(-40.5075708171276,38.5394214322887,40.8482445775075));
#32756=CARTESIAN_POINT('Ctrl Pts',(-40.5490500104958,38.6366735953907,40.8886643841204));
#32757=CARTESIAN_POINT('Ctrl Pts',(-40.590529203864,38.7339257584929,40.9290841907332));
#32758=CARTESIAN_POINT('Ctrl Pts',(-40.6297548417044,38.8331432576641,40.9670896427955));
#32759=CARTESIAN_POINT('Ctrl Pts',(-40.6666366022296,38.934097830037,41.002593220518));
#32760=CARTESIAN_POINT('Ctrl Pts',(-40.7035183627549,39.0350524024099,41.0380967982405));
#32761=CARTESIAN_POINT('Ctrl Pts',(-40.7380562199081,39.1377439768077,41.0710984765346));
#32762=CARTESIAN_POINT('Ctrl Pts',(-40.7701706254072,39.2419362974163,41.1015222356531));
#32763=CARTESIAN_POINT('Ctrl Pts',(-40.8022850309064,39.3461286180248,41.1319459947717));
#32764=CARTESIAN_POINT('Ctrl Pts',(-40.8319759620484,39.4518216113835,41.1597918131997));
#32765=CARTESIAN_POINT('Ctrl Pts',(-40.8591750098643,39.558772113834,41.1849955208619));
#32766=CARTESIAN_POINT('Ctrl Pts',(-40.8863740576804,39.6657226162845,41.2101992285241));
#32767=CARTESIAN_POINT('Ctrl Pts',(-40.9110812029252,39.773930552419,41.2327608075782));
#32768=CARTESIAN_POINT('Ctrl Pts',(-40.9332394906484,39.8831469675769,41.2526282328875));
#32769=CARTESIAN_POINT('Ctrl Pts',(-40.9553977783715,39.9923633827349,41.2724956581968));
#32770=CARTESIAN_POINT('Ctrl Pts',(-40.9750071928742,40.1025881999071,41.2896689156735));
#32771=CARTESIAN_POINT('Ctrl Pts',(-40.9920224953816,40.2135678168966,41.3041083646667));
#32772=CARTESIAN_POINT('Ctrl Pts',(-41.009037797889,40.3245474338861,41.31854781366));
#32773=CARTESIAN_POINT('Ctrl Pts',(-41.0234589763207,40.4362817724348,41.3302534439013));
#32774=CARTESIAN_POINT('Ctrl Pts',(-41.0352527164837,40.5485137476579,41.3391981819529));
#32775=CARTESIAN_POINT('Ctrl Pts',(-41.0470464566467,40.6607457228809,41.3481429200046));
#32776=CARTESIAN_POINT('Ctrl Pts',(-41.0562127501345,40.7734752556303,41.3543267594645));
#32777=CARTESIAN_POINT('Ctrl Pts',(-41.0627303610314,40.886442959227,41.3577353191749));
#32778=CARTESIAN_POINT('Ctrl Pts',(-41.0692479719283,40.9994106628236,41.3611438788854));
#32779=CARTESIAN_POINT('Ctrl Pts',(-41.0731168955402,41.1126164575932,41.361777156341));
#32780=CARTESIAN_POINT('Ctrl Pts',(-41.0743280725085,41.225799846588,41.3596335294917));
#32781=CARTESIAN_POINT('Ctrl Pts',(-41.0755392494769,41.3389832355827,41.3574899026424));
#32782=CARTESIAN_POINT('Ctrl Pts',(-41.0740926788428,41.452144138965,41.3525693728901));
#32783=CARTESIAN_POINT('Ctrl Pts',(-41.0699915202077,41.5650221462243,41.3448830855782));
#32784=CARTESIAN_POINT('Ctrl Pts',(-41.0658903615727,41.6779001534836,41.3371967982663));
#32785=CARTESIAN_POINT('Ctrl Pts',(-41.0591346177177,41.7904951849852,41.3267447586977));
#32786=CARTESIAN_POINT('Ctrl Pts',(-41.049739653545,41.9025481130374,41.3135508292975));
#32787=CARTESIAN_POINT('Ctrl Pts',(-41.040336339667,42.0147006273062,41.3003451738894));
#32788=CARTESIAN_POINT('Ctrl Pts',(-41.02828911873,42.126309994911,41.2843927620129));
#32789=CARTESIAN_POINT('Ctrl Pts',(-41.0136255646488,42.2371188766663,41.2657301618302));
#32790=CARTESIAN_POINT('Ctrl Pts',(-39.6924821306133,37.3539385160429,40.1901910998149));
#32791=CARTESIAN_POINT('Ctrl Pts',(-39.7550437057594,37.4279635608479,40.2533257828455));
#32792=CARTESIAN_POINT('Ctrl Pts',(-39.8158746486762,37.5050729659852,40.3145589119263));
#32793=CARTESIAN_POINT('Ctrl Pts',(-39.8748285637661,37.5850811601499,40.3737431235591));
#32794=CARTESIAN_POINT('Ctrl Pts',(-39.9337824788559,37.6650893543145,40.4329273351919));
#32795=CARTESIAN_POINT('Ctrl Pts',(-39.9908593205375,37.7479962756468,40.4900625836176));
#32796=CARTESIAN_POINT('Ctrl Pts',(-40.0459217278239,37.8336024005534,40.5450113672875));
#32797=CARTESIAN_POINT('Ctrl Pts',(-40.1009841351103,37.9192085254601,40.5999601509574));
#32798=CARTESIAN_POINT('Ctrl Pts',(-40.154032065429,38.0075137877534,40.652722427387));
#32799=CARTESIAN_POINT('Ctrl Pts',(-40.2049378537611,38.0983056722058,40.7031712190114));
#32800=CARTESIAN_POINT('Ctrl Pts',(-40.2558436420933,38.1890975566583,40.7536200106359));
#32801=CARTESIAN_POINT('Ctrl Pts',(-40.3046072490803,38.2823759930726,40.8017552784498));
#32802=CARTESIAN_POINT('Ctrl Pts',(-40.3511113203454,38.3779164977929,40.8474611802359));
#32803=CARTESIAN_POINT('Ctrl Pts',(-40.3976153916104,38.4734570025133,40.8931670820219));
#32804=CARTESIAN_POINT('Ctrl Pts',(-40.441859891198,38.5712595016707,40.9364435824419));
#32805=CARTESIAN_POINT('Ctrl Pts',(-40.4837383404043,38.671088624011,40.9771865323761));
#32806=CARTESIAN_POINT('Ctrl Pts',(-40.5256167896104,38.7709177463515,41.0179294823103));
#32807=CARTESIAN_POINT('Ctrl Pts',(-40.5651291560561,38.8727734146902,41.0561388502577));
#32808=CARTESIAN_POINT('Ctrl Pts',(-40.6021803493774,38.9764105034259,41.0917226816472));
#32809=CARTESIAN_POINT('Ctrl Pts',(-40.6392315426986,39.0800475921617,41.1273065130367));
#32810=CARTESIAN_POINT('Ctrl Pts',(-40.6738215342485,39.1854660211658,41.1602647803561));
#32811=CARTESIAN_POINT('Ctrl Pts',(-40.7058670798385,39.2924120907059,41.1905181663201));
#32812=CARTESIAN_POINT('Ctrl Pts',(-40.7379126254285,39.3993581602459,41.2207715522841));
#32813=CARTESIAN_POINT('Ctrl Pts',(-40.7674137002819,39.5078317876348,41.2483200335019));
#32814=CARTESIAN_POINT('Ctrl Pts',(-40.7942993071845,39.6175719205072,41.2730973118662));
#32815=CARTESIAN_POINT('Ctrl Pts',(-40.8211849140871,39.7273120533795,41.2978745902305));
#32816=CARTESIAN_POINT('Ctrl Pts',(-40.8454550322518,39.838318606888,41.3198806465843));
#32817=CARTESIAN_POINT('Ctrl Pts',(-40.8670512532719,39.9503244329335,41.3390625212065));
#32818=CARTESIAN_POINT('Ctrl Pts',(-40.8886474742919,40.0623302589791,41.3582443958287));
#32819=CARTESIAN_POINT('Ctrl Pts',(-40.9075697814698,40.1753352709624,41.3746020738885));
#32820=CARTESIAN_POINT('Ctrl Pts',(-40.9237726364277,40.2890675112993,41.3880961890381));
#32821=CARTESIAN_POINT('Ctrl Pts',(-40.9399754913854,40.4027997516363,41.4015903041876));
#32822=CARTESIAN_POINT('Ctrl Pts',(-40.9534588815956,40.5172591323928,41.4122208459937));
#32823=CARTESIAN_POINT('Ctrl Pts',(-40.9641903579644,40.6321701959042,41.4199622310205));
#32824=CARTESIAN_POINT('Ctrl Pts',(-40.9749218343331,40.7470812594156,41.4277036160472));
#32825=CARTESIAN_POINT('Ctrl Pts',(-40.9829013885633,40.8624439168365,41.4325558383094));
#32826=CARTESIAN_POINT('Ctrl Pts',(-40.9881098170792,40.9779805366789,41.4345072204607));
#32827=CARTESIAN_POINT('Ctrl Pts',(-40.9933182455951,41.0935171565213,41.436458602612));
#32828=CARTESIAN_POINT('Ctrl Pts',(-40.9957555443691,41.209227649457,41.4355091431444));
#32829=CARTESIAN_POINT('Ctrl Pts',(-40.9954158478053,41.3248335468961,41.4316611270233));
#32830=CARTESIAN_POINT('Ctrl Pts',(-40.9950761512415,41.4404394443352,41.4278131109023));
#32831=CARTESIAN_POINT('Ctrl Pts',(-40.9919594596027,41.5559406568948,41.4210665411031));
#32832=CARTESIAN_POINT('Ctrl Pts',(-40.9860732735097,41.6710592196427,41.4114376539052));
#32833=CARTESIAN_POINT('Ctrl Pts',(-40.9801870874168,41.7861777823904,41.4018087667073));
#32834=CARTESIAN_POINT('Ctrl Pts',(-40.9715314114214,41.9009136063195,41.3892975695548));
#32835=CARTESIAN_POINT('Ctrl Pts',(-40.9601270762523,42.0149905684778,41.3739341718642));
#32836=CARTESIAN_POINT('Ctrl Pts',(-40.9487126055641,42.129168915698,41.3585571200667));
#32837=CARTESIAN_POINT('Ctrl Pts',(-40.9345445966629,42.2426871411525,41.3403228076332));
#32838=CARTESIAN_POINT('Ctrl Pts',(-40.9176572009828,42.3552715649338,41.319275189134));
#32839=CARTESIAN_POINT('Ctrl Pts',(-39.6135628167506,37.3562205905267,40.2657183011866));
#32840=CARTESIAN_POINT('Ctrl Pts',(-39.6774756216741,37.4318340440419,40.3301997006854));
#32841=CARTESIAN_POINT('Ctrl Pts',(-39.7395834805726,37.510664296499,40.3926978931619));
#32842=CARTESIAN_POINT('Ctrl Pts',(-39.7997306457477,37.5925136758369,40.4530561500275));
#32843=CARTESIAN_POINT('Ctrl Pts',(-39.8598778109228,37.6743630551748,40.5134144068931));
#32844=CARTESIAN_POINT('Ctrl Pts',(-39.9180642319583,37.7592314928005,40.5716326775531));
#32845=CARTESIAN_POINT('Ctrl Pts',(-39.9741439859836,37.8469061867413,40.6275649564589));
#32846=CARTESIAN_POINT('Ctrl Pts',(-40.030223740009,37.9345808806821,40.6834972353646));
#32847=CARTESIAN_POINT('Ctrl Pts',(-40.0841967800109,38.0250617574698,40.7371434756245));
#32848=CARTESIAN_POINT('Ctrl Pts',(-40.1359277389027,38.1181219510228,40.7883691261129));
#32849=CARTESIAN_POINT('Ctrl Pts',(-40.1876586977945,38.2111821445759,40.8395947766013));
#32850=CARTESIAN_POINT('Ctrl Pts',(-40.2371475322013,38.3068215769179,40.8883997943643));
#32851=CARTESIAN_POINT('Ctrl Pts',(-40.2842701089497,38.4048004540608,40.9346617567584));
#32852=CARTESIAN_POINT('Ctrl Pts',(-40.3313926856981,38.5027793312036,40.9809237191525));
#32853=CARTESIAN_POINT('Ctrl Pts',(-40.3761489652685,38.6030975710527,41.0246425873763));
#32854=CARTESIAN_POINT('Ctrl Pts',(-40.4184266703127,38.7055036526314,41.0657086806318));
#32855=CARTESIAN_POINT('Ctrl Pts',(-40.4607043753569,38.8079097342101,41.1067747738874));
#32856=CARTESIAN_POINT('Ctrl Pts',(-40.500503470408,38.9124035717163,41.14518805772));
#32857=CARTESIAN_POINT('Ctrl Pts',(-40.5377240965251,39.0187231768149,41.1808521427764));
#32858=CARTESIAN_POINT('Ctrl Pts',(-40.5749447226423,39.1250427819136,41.2165162278329));
#32859=CARTESIAN_POINT('Ctrl Pts',(-40.609586848589,39.2331880655239,41.2494310841775));
#32860=CARTESIAN_POINT('Ctrl Pts',(-40.6415635342698,39.3428878839955,41.279514096987));
#32861=CARTESIAN_POINT('Ctrl Pts',(-40.6735402199505,39.4525877024671,41.3095971097965));
#32862=CARTESIAN_POINT('Ctrl Pts',(-40.7028514385154,39.563841963886,41.3368482538041));
#32863=CARTESIAN_POINT('Ctrl Pts',(-40.7294236045046,39.6763717271803,41.3611991028705));
#32864=CARTESIAN_POINT('Ctrl Pts',(-40.7559957704939,39.7889014904745,41.3855499519369));
#32865=CARTESIAN_POINT('Ctrl Pts',(-40.7798288615784,39.9027066613571,41.4070004855904));
#32866=CARTESIAN_POINT('Ctrl Pts',(-40.8008630158954,40.0175018982901,41.4254968095255));
#32867=CARTESIAN_POINT('Ctrl Pts',(-40.8218971702123,40.1322971352231,41.4439931334607));
#32868=CARTESIAN_POINT('Ctrl Pts',(-40.8401323700655,40.2480823420177,41.4595352321036));
#32869=CARTESIAN_POINT('Ctrl Pts',(-40.8555227774737,40.3645672057021,41.4720840134094));
#32870=CARTESIAN_POINT('Ctrl Pts',(-40.8709131848819,40.4810520693865,41.4846327947152));
#32871=CARTESIAN_POINT('Ctrl Pts',(-40.8834587868704,40.5982364923508,41.494188248086));
#32872=CARTESIAN_POINT('Ctrl Pts',(-40.893127999445,40.7158266441505,41.500726280088));
#32873=CARTESIAN_POINT('Ctrl Pts',(-40.9027972120195,40.8334167959504,41.5072643120899));
#32874=CARTESIAN_POINT('Ctrl Pts',(-40.9095900269921,40.9514125780428,41.5107849171542));
#32875=CARTESIAN_POINT('Ctrl Pts',(-40.913489273127,41.0695181141309,41.5112791217464));
#32876=CARTESIAN_POINT('Ctrl Pts',(-40.9173885192619,41.187623650219,41.5117733263386));
#32877=CARTESIAN_POINT('Ctrl Pts',(-40.918394193198,41.3058388413209,41.5092411299477));
#32878=CARTESIAN_POINT('Ctrl Pts',(-40.9165036231021,41.4238672472043,41.503688724555));
#32879=CARTESIAN_POINT('Ctrl Pts',(-40.9146130530062,41.5418956530876,41.4981363191623));
#32880=CARTESIAN_POINT('Ctrl Pts',(-40.9098262403625,41.6597371748247,41.489563709316));
#32881=CARTESIAN_POINT('Ctrl Pts',(-40.9021550268117,41.777096293061,41.4779922222321));
#32882=CARTESIAN_POINT('Ctrl Pts',(-40.8944838132608,41.8944554112973,41.4664207351483));
#32883=CARTESIAN_POINT('Ctrl Pts',(-40.8839282051252,42.0113320276539,41.4518503804119));
#32884=CARTESIAN_POINT('Ctrl Pts',(-40.8705144989597,42.1274330239181,41.4343175144308));
#32885=CARTESIAN_POINT('Ctrl Pts',(-40.8570888714613,42.2436372040898,41.4167690662439));
#32886=CARTESIAN_POINT('Ctrl Pts',(-40.8408000745959,42.3590642873939,41.3962528532535));
#32887=CARTESIAN_POINT('Ctrl Pts',(-40.8216888373169,42.4734242532013,41.3728202164377));
#32888=CARTESIAN_POINT('Ctrl Pts',(-39.5346528073732,37.3585135271757,40.341254653468));
#32889=CARTESIAN_POINT('Ctrl Pts',(-39.5998972885217,37.4356857994494,40.4070525688079));
#32890=CARTESIAN_POINT('Ctrl Pts',(-39.6632614971712,37.5162091132762,40.4707845113903));
#32891=CARTESIAN_POINT('Ctrl Pts',(-39.7245799035767,37.5998731232236,40.5322839864252));
#32892=CARTESIAN_POINT('Ctrl Pts',(-39.7858983099821,37.6835371331711,40.59378346146));
#32893=CARTESIAN_POINT('Ctrl Pts',(-39.8451708583676,37.7703417631542,40.6530504130031));
#32894=CARTESIAN_POINT('Ctrl Pts',(-39.9022426979749,37.8600602717383,40.7099299997107));
#32895=CARTESIAN_POINT('Ctrl Pts',(-39.9593145375822,37.9497787803222,40.7668095864183));
#32896=CARTESIAN_POINT('Ctrl Pts',(-40.0141856164902,38.042411085924,40.82130175654));
#32897=CARTESIAN_POINT('Ctrl Pts',(-40.0667125709269,38.1377152340127,40.8732641301578));
#32898=CARTESIAN_POINT('Ctrl Pts',(-40.1192395253635,38.2330193821015,40.9252265037756));
#32899=CARTESIAN_POINT('Ctrl Pts',(-40.1694223075328,38.3309952860207,40.9746590336024));
#32900=CARTESIAN_POINT('Ctrl Pts',(-40.2171297887776,38.4313870403645,41.0214325441754));
#32901=CARTESIAN_POINT('Ctrl Pts',(-40.2648372700223,38.5317787947084,41.0682060547483));
#32902=CARTESIAN_POINT('Ctrl Pts',(-40.3100694069207,38.634586308198,41.1123205034901));
#32903=CARTESIAN_POINT('Ctrl Pts',(-40.3527079902916,38.7395410595142,41.1536605936016));
#32904=CARTESIAN_POINT('Ctrl Pts',(-40.3953465736626,38.8444958108302,41.1950006837132));
#32905=CARTESIAN_POINT('Ctrl Pts',(-40.4353915646849,38.9515977045472,41.2335663775487));
#32906=CARTESIAN_POINT('Ctrl Pts',(-40.4727382906827,39.0605670041845,41.2692568588486));
#32907=CARTESIAN_POINT('Ctrl Pts',(-40.5100850166805,39.1695363038219,41.3049473401485));
#32908=CARTESIAN_POINT('Ctrl Pts',(-40.5447334436354,39.2803729103039,41.3377625763946));
#32909=CARTESIAN_POINT('Ctrl Pts',(-40.5765929818585,39.3927873312385,41.3676167582733));
#32910=CARTESIAN_POINT('Ctrl Pts',(-40.6084525200816,39.5052017521732,41.3974709401519));
#32911=CARTESIAN_POINT('Ctrl Pts',(-40.6375231405345,39.6191938853506,41.424364040442));
#32912=CARTESIAN_POINT('Ctrl Pts',(-40.6637288096024,39.7344659926158,41.448225704969));
#32913=CARTESIAN_POINT('Ctrl Pts',(-40.6899344786702,39.8497380998812,41.472087369496));
#32914=CARTESIAN_POINT('Ctrl Pts',(-40.7132751724454,39.9662900764232,41.4929175764786));
#32915=CARTESIAN_POINT('Ctrl Pts',(-40.7336898106128,40.0838174915083,41.5106617945233));
#32916=CARTESIAN_POINT('Ctrl Pts',(-40.7541044487802,40.2013449065934,41.5284060125681));
#32917=CARTESIAN_POINT('Ctrl Pts',(-40.7715930126886,40.3198476533541,41.5430642254468));
#32918=CARTESIAN_POINT('Ctrl Pts',(-40.786109694613,40.4390161966153,41.5545980097256));
#32919=CARTESIAN_POINT('Ctrl Pts',(-40.8006263765375,40.5581847398765,41.5661317940043));
#32920=CARTESIAN_POINT('Ctrl Pts',(-40.8121711631813,40.6780189712691,41.5745411390913));
#32921=CARTESIAN_POINT('Ctrl Pts',(-40.8207137591026,40.7982058659919,41.5798039307316));
#32922=CARTESIAN_POINT('Ctrl Pts',(-40.8292563550239,40.9183927607145,41.585066722372));
#32923=CARTESIAN_POINT('Ctrl Pts',(-40.834796752349,41.0389322094628,41.587182955667));
#32924=CARTESIAN_POINT('Ctrl Pts',(-40.8373203267629,41.1595093308912,41.5861469417492));
#32925=CARTESIAN_POINT('Ctrl Pts',(-40.8398439011769,41.2800864523198,41.5851109278313));
#32926=CARTESIAN_POINT('Ctrl Pts',(-40.8393506502698,41.4007011367585,41.5809226675212));
#32927=CARTESIAN_POINT('Ctrl Pts',(-40.835841698011,41.5210382891738,41.5735929279324));
#32928=CARTESIAN_POINT('Ctrl Pts',(-40.8323327457522,41.6413754415893,41.5662631883435));
#32929=CARTESIAN_POINT('Ctrl Pts',(-40.825808095209,41.761434952516,41.5557919760115));
#32930=CARTESIAN_POINT('Ctrl Pts',(-40.8162846137041,41.8809031572982,41.5422064588396));
#32931=CARTESIAN_POINT('Ctrl Pts',(-40.8067611321992,42.0003713620803,41.5286209416676));
#32932=CARTESIAN_POINT('Ctrl Pts',(-40.7942388282604,42.1192481520286,41.5119211318735));
#32933=CARTESIAN_POINT('Ctrl Pts',(-40.778750225565,42.2372229295778,41.492150457457));
#32934=CARTESIAN_POINT('Ctrl Pts',(-40.7632478574878,42.3553025563437,41.472362211999));
#32935=CARTESIAN_POINT('Ctrl Pts',(-40.7447739297299,42.4724784591441,41.4494976589433));
#32936=CARTESIAN_POINT('Ctrl Pts',(-40.723376581818,42.5884439120029,41.4236164196056));
#32937=CARTESIAN_POINT('Ctrl Pts',(-39.4557619421374,37.3608288129201,40.4168098339066));
#32938=CARTESIAN_POINT('Ctrl Pts',(-39.5223241949095,37.4395364367563,40.4838988547304));
#32939=CARTESIAN_POINT('Ctrl Pts',(-39.5869297733209,37.5217312603981,40.5488379555043));
#32940=CARTESIAN_POINT('Ctrl Pts',(-39.6494029164308,37.6071896709646,40.6114504679323));
#32941=CARTESIAN_POINT('Ctrl Pts',(-39.7118760595407,37.6926480815311,40.6740629803604));
#32942=CARTESIAN_POINT('Ctrl Pts',(-39.772216705614,37.7813699945731,40.7343488425698));
#32943=CARTESIAN_POINT('Ctrl Pts',(-39.830260696555,37.873114040115,40.7921440455055));
#32944=CARTESIAN_POINT('Ctrl Pts',(-39.888304687496,37.9648580856568,40.8499392484413));
#32945=CARTESIAN_POINT('Ctrl Pts',(-39.9440519659463,38.0596241730381,40.905243734991));
#32946=CARTESIAN_POINT('Ctrl Pts',(-39.9973508701712,38.1571544889698,40.9579070480451));
#32947=CARTESIAN_POINT('Ctrl Pts',(-40.0506497743961,38.2546848049014,41.0105703610992));
#32948=CARTESIAN_POINT('Ctrl Pts',(-40.1015002517261,38.3549792530051,41.0605924486165));
#32949=CARTESIAN_POINT('Ctrl Pts',(-40.149763962285,38.457764979961,41.1078372243739));
#32950=CARTESIAN_POINT('Ctrl Pts',(-40.1980276728438,38.5605507069169,41.1550820001313));
#32951=CARTESIAN_POINT('Ctrl Pts',(-40.2437045689378,38.6658276111535,41.199549417442));
#32952=CARTESIAN_POINT('Ctrl Pts',(-40.2866703855357,38.773309284466,41.2411185016893));
#32953=CARTESIAN_POINT('Ctrl Pts',(-40.3296362021336,38.8807909577785,41.2826875859365));
#32954=CARTESIAN_POINT('Ctrl Pts',(-40.369890896777,38.9904772939548,41.3213582960421));
#32955=CARTESIAN_POINT('Ctrl Pts',(-40.4073249556566,39.1020698888309,41.3570254274626));
#32956=CARTESIAN_POINT('Ctrl Pts',(-40.4447590145362,39.2136624837069,41.3926925588832));
#32957=CARTESIAN_POINT('Ctrl Pts',(-40.4793724006601,39.327161227008,41.4253560763727));
#32958=CARTESIAN_POINT('Ctrl Pts',(-40.5110709475265,39.4422573428303,41.4549271180914));
#32959=CARTESIAN_POINT('Ctrl Pts',(-40.542769494393,39.5573534586525,41.4844981598102));
#32960=CARTESIAN_POINT('Ctrl Pts',(-40.571553170678,39.674046833259,41.5109766965364));
#32961=CARTESIAN_POINT('Ctrl Pts',(-40.5973436697376,39.7920199996788,41.5342906928107));
#32962=CARTESIAN_POINT('Ctrl Pts',(-40.6231341687972,39.9099931660986,41.5576046890849));
#32963=CARTESIAN_POINT('Ctrl Pts',(-40.6459314651451,40.0292460077526,41.5777541218692));
#32964=CARTESIAN_POINT('Ctrl Pts',(-40.6656735382207,40.1494540945804,41.5946841741736));
#32965=CARTESIAN_POINT('Ctrl Pts',(-40.6854156112962,40.2696621814082,41.611614226478));
#32966=CARTESIAN_POINT('Ctrl Pts',(-40.7021024415902,40.390825394622,41.625324881573));
#32967=CARTESIAN_POINT('Ctrl Pts',(-40.7156886322023,40.5126141069537,41.6357788393107));
#32968=CARTESIAN_POINT('Ctrl Pts',(-40.7292748228144,40.6344028192854,41.6462327970483));
#32969=CARTESIAN_POINT('Ctrl Pts',(-40.7397603603196,40.7568169103839,41.6534300470975));
#32970=CARTESIAN_POINT('Ctrl Pts',(-40.7471167185743,40.8795233499408,41.6573510091775));
#32971=CARTESIAN_POINT('Ctrl Pts',(-40.754473076829,41.0022297894977,41.6612719712575));
#32972=CARTESIAN_POINT('Ctrl Pts',(-40.7587002485643,41.1252284562551,41.6619166414932));
#32973=CARTESIAN_POINT('Ctrl Pts',(-40.7597867336636,41.2481847295518,41.6592832660444));
#32974=CARTESIAN_POINT('Ctrl Pts',(-40.7608732187629,41.3711410028484,41.6566498905956));
#32975=CARTESIAN_POINT('Ctrl Pts',(-40.7588190161525,41.4940547611804,41.6507384720647));
#32976=CARTESIAN_POINT('Ctrl Pts',(-40.7536297143373,41.6165916148816,41.6415650925998));
#32977=CARTESIAN_POINT('Ctrl Pts',(-40.7484404125221,41.7391284685829,41.6323917131349));
#32978=CARTESIAN_POINT('Ctrl Pts',(-40.74011601663,41.8612882965639,41.619956381801));
#32979=CARTESIAN_POINT('Ctrl Pts',(-40.7286791733688,41.9827387602433,41.6042929291989));
#32980=CARTESIAN_POINT('Ctrl Pts',(-40.7172423301077,42.1041892239226,41.5886294765968));
#32981=CARTESIAN_POINT('Ctrl Pts',(-40.7026930507781,42.2249302032856,41.5697379182055));
#32982=CARTESIAN_POINT('Ctrl Pts',(-40.6850709170265,42.3446332197583,41.5476696489369));
#32983=CARTESIAN_POINT('Ctrl Pts',(-40.6674331217329,42.4644426214073,41.525581766656));
#32984=CARTESIAN_POINT('Ctrl Pts',(-40.6467170250815,42.583212095883,41.5003115462781));
#32985=CARTESIAN_POINT('Ctrl Pts',(-40.6229790784524,42.7006179510356,41.4719278505636));
#32986=CARTESIAN_POINT('Ctrl Pts',(-39.3768710769017,37.3631440986644,40.4923650143452));
#32987=CARTESIAN_POINT('Ctrl Pts',(-39.4447511012974,37.4433870740631,40.5607451406529));
#32988=CARTESIAN_POINT('Ctrl Pts',(-39.5105980494706,37.52725340752,40.6268913996182));
#32989=CARTESIAN_POINT('Ctrl Pts',(-39.574225929285,37.6145062187056,40.6906169494395));
#32990=CARTESIAN_POINT('Ctrl Pts',(-39.6378538090993,37.7017590298911,40.7543424992609));
#32991=CARTESIAN_POINT('Ctrl Pts',(-39.6992625528604,37.7923982259919,40.8156472721364));
#32992=CARTESIAN_POINT('Ctrl Pts',(-39.7582786951351,37.8861678084917,40.8743580913004));
#32993=CARTESIAN_POINT('Ctrl Pts',(-39.8172948374097,37.9799373909914,40.9330689104643));
#32994=CARTESIAN_POINT('Ctrl Pts',(-39.8739183154024,38.0768372601523,40.9891857134419));
#32995=CARTESIAN_POINT('Ctrl Pts',(-39.9279891694155,38.1765937439268,41.0425499659323));
#32996=CARTESIAN_POINT('Ctrl Pts',(-39.9820600234286,38.2763502277013,41.0959142184228));
#32997=CARTESIAN_POINT('Ctrl Pts',(-40.0335781959193,38.3789632199894,41.1465258636306));
#32998=CARTESIAN_POINT('Ctrl Pts',(-40.0823981357924,38.4841429195575,41.1942419045724));
#32999=CARTESIAN_POINT('Ctrl Pts',(-40.1312180756654,38.5893226191255,41.2419579455143));
#33000=CARTESIAN_POINT('Ctrl Pts',(-40.177339730955,38.6970689141089,41.286778331394));
#33001=CARTESIAN_POINT('Ctrl Pts',(-40.2206327807798,38.8070775094178,41.328576409777));
#33002=CARTESIAN_POINT('Ctrl Pts',(-40.2639258306046,38.9170861047267,41.3703744881599));
#33003=CARTESIAN_POINT('Ctrl Pts',(-40.3043902288691,39.0293568833625,41.4091502145356));
#33004=CARTESIAN_POINT('Ctrl Pts',(-40.3419116206305,39.1435727734772,41.4447939960767));
#33005=CARTESIAN_POINT('Ctrl Pts',(-40.3794330123919,39.2577886635919,41.4804377776179));
#33006=CARTESIAN_POINT('Ctrl Pts',(-40.4140113576848,39.3739495437122,41.5129495763508));
#33007=CARTESIAN_POINT('Ctrl Pts',(-40.4455489131946,39.491727354422,41.5422374779096));
#33008=CARTESIAN_POINT('Ctrl Pts',(-40.4770864687044,39.6095051651317,41.5715253794685));
#33009=CARTESIAN_POINT('Ctrl Pts',(-40.5055832008214,39.7288997811675,41.5975893526308));
#33010=CARTESIAN_POINT('Ctrl Pts',(-40.5309585298728,39.8495740067417,41.6203556806524));
#33011=CARTESIAN_POINT('Ctrl Pts',(-40.5563338589242,39.9702482323161,41.6431220086739));
#33012=CARTESIAN_POINT('Ctrl Pts',(-40.5785877578449,40.0922019390821,41.6625906672598));
#33013=CARTESIAN_POINT('Ctrl Pts',(-40.5976572658285,40.2150906976525,41.6787065538238));
#33014=CARTESIAN_POINT('Ctrl Pts',(-40.6167267738122,40.3379794562229,41.6948224403878));
#33015=CARTESIAN_POINT('Ctrl Pts',(-40.6326118704917,40.46180313589,41.7075855376992));
#33016=CARTESIAN_POINT('Ctrl Pts',(-40.6452675697915,40.5862120172922,41.7169596688957));
#33017=CARTESIAN_POINT('Ctrl Pts',(-40.6579232690913,40.7106208986944,41.7263338000923));
#33018=CARTESIAN_POINT('Ctrl Pts',(-40.667349557458,40.8356148494986,41.7323189551036));
#33019=CARTESIAN_POINT('Ctrl Pts',(-40.6735196780461,40.9608408338897,41.7348980876234));
#33020=CARTESIAN_POINT('Ctrl Pts',(-40.6796897986341,41.0860668182808,41.737477220143));
#33021=CARTESIAN_POINT('Ctrl Pts',(-40.6826037447796,41.2115247030474,41.7366503273193));
#33022=CARTESIAN_POINT('Ctrl Pts',(-40.6822531405642,41.3368601282123,41.7324195903396));
#33023=CARTESIAN_POINT('Ctrl Pts',(-40.6819025363488,41.4621955533772,41.72818885336));
#33024=CARTESIAN_POINT('Ctrl Pts',(-40.6782873820352,41.5874083856024,41.7205542766081));
#33025=CARTESIAN_POINT('Ctrl Pts',(-40.6714177306635,41.7121449405895,41.7095372572672));
#33026=CARTESIAN_POINT('Ctrl Pts',(-40.6645480792919,41.8368814955765,41.6985202379262));
#33027=CARTESIAN_POINT('Ctrl Pts',(-40.6544239380509,41.9611416406117,41.6841207875904));
#33028=CARTESIAN_POINT('Ctrl Pts',(-40.6410737330335,42.0845743631883,41.6663793995582));
#33029=CARTESIAN_POINT('Ctrl Pts',(-40.6277235280161,42.208007085765,41.6486380115259));
#33030=CARTESIAN_POINT('Ctrl Pts',(-40.6111472732959,42.3306122545426,41.6275547045377));
#33031=CARTESIAN_POINT('Ctrl Pts',(-40.5913916084879,42.4520435099388,41.6031888404167));
#33032=CARTESIAN_POINT('Ctrl Pts',(-40.5716183859781,42.573582686471,41.5788013213131));
#33033=CARTESIAN_POINT('Ctrl Pts',(-40.5486601204331,42.6939457326218,41.5511254336129));
#33034=CARTESIAN_POINT('Ctrl Pts',(-40.5225815750869,42.8127919900683,41.5202392815215));
#33035=CARTESIAN_POINT('Ctrl Pts',(-39.2979993170057,37.3654816882064,40.5679389847796));
#33036=CARTESIAN_POINT('Ctrl Pts',(-39.367183179944,37.4472365158672,40.6375847800584));
#33037=CARTESIAN_POINT('Ctrl Pts',(-39.4342564894374,37.5327527754326,40.7049115791748));
#33038=CARTESIAN_POINT('Ctrl Pts',(-39.4990225730245,37.6217797250398,40.7697219594771));
#33039=CARTESIAN_POINT('Ctrl Pts',(-39.5637886566116,37.7108066746471,40.8345323397794));
#33040=CARTESIAN_POINT('Ctrl Pts',(-39.6262474400391,37.8033442122469,40.8968262269577));
#33041=CARTESIAN_POINT('Ctrl Pts',(-39.6862157711,37.8991210217028,40.9564209445738));
#33042=CARTESIAN_POINT('Ctrl Pts',(-39.746184102161,37.9948978311585,41.0160156621899));
#33043=CARTESIAN_POINT('Ctrl Pts',(-39.8036619120932,38.0939138026928,41.0729111419033));
#33044=CARTESIAN_POINT('Ctrl Pts',(-39.8584806419644,38.1958786351937,41.1269405237714));
#33045=CARTESIAN_POINT('Ctrl Pts',(-39.9132993718355,38.2978434676945,41.1809699056395));
#33046=CARTESIAN_POINT('Ctrl Pts',(-39.9654589587768,38.4027570442984,41.2321331276911));
#33047=CARTESIAN_POINT('Ctrl Pts',(-40.0148064247347,38.5103117793659,41.2802801241842));
#33048=CARTESIAN_POINT('Ctrl Pts',(-40.0641538906926,38.6178665144333,41.3284271206772));
#33049=CARTESIAN_POINT('Ctrl Pts',(-40.1106891790595,38.7280622846981,41.3735578363725));
#33050=CARTESIAN_POINT('Ctrl Pts',(-40.1542757890722,38.840576021645,41.4155398791369));
#33051=CARTESIAN_POINT('Ctrl Pts',(-40.1978623990849,38.9530897585918,41.4575219219013));
#33052=CARTESIAN_POINT('Ctrl Pts',(-40.2385002807281,39.0679213332727,41.4963552435508));
#33053=CARTESIAN_POINT('Ctrl Pts',(-40.2760702105016,39.1847340866154,41.5319259015271));
#33054=CARTESIAN_POINT('Ctrl Pts',(-40.3136401402752,39.3015468399581,41.5674965595035));
#33055=CARTESIAN_POINT('Ctrl Pts',(-40.3481420750489,39.420340638087,41.5998045129599));
#33056=CARTESIAN_POINT('Ctrl Pts',(-40.3794747674399,39.5407672032934,41.6287549368956));
#33057=CARTESIAN_POINT('Ctrl Pts',(-40.410807459831,39.6611937684996,41.6577053608314));
#33058=CARTESIAN_POINT('Ctrl Pts',(-40.4389708738467,39.7832529627628,41.683298221976));
#33059=CARTESIAN_POINT('Ctrl Pts',(-40.4638823318658,39.9065869297263,41.7054583689751));
#33060=CARTESIAN_POINT('Ctrl Pts',(-40.4887937898849,40.0299208966897,41.7276185159742));
#33061=CARTESIAN_POINT('Ctrl Pts',(-40.5104532632632,40.1545294949953,41.7463459233285));
#33062=CARTESIAN_POINT('Ctrl Pts',(-40.5287971291004,40.280047385766,41.7615855542687));
#33063=CARTESIAN_POINT('Ctrl Pts',(-40.5471409949375,40.4055652765367,41.7768251852089));
#33064=CARTESIAN_POINT('Ctrl Pts',(-40.5621692321055,40.5319923159037,41.7885770221565));
#33065=CARTESIAN_POINT('Ctrl Pts',(-40.5738376458591,40.6589578224765,41.7968064661327));
#33066=CARTESIAN_POINT('Ctrl Pts',(-40.5855060596127,40.7859233290494,41.8050359101089));
#33067=CARTESIAN_POINT('Ctrl Pts',(-40.5938146364638,40.91342715729,41.8097429515589));
#33068=CARTESIAN_POINT('Ctrl Pts',(-40.5987388695419,41.0410954546661,41.8109136328711));
#33069=CARTESIAN_POINT('Ctrl Pts',(-40.60366310262,41.1687637520422,41.8120843141834));
#33070=CARTESIAN_POINT('Ctrl Pts',(-40.6052029861564,41.2965963721973,41.8097186338833));
#33071=CARTESIAN_POINT('Ctrl Pts',(-40.603353845636,41.4242184814935,41.8038233584774));
#33072=CARTESIAN_POINT('Ctrl Pts',(-40.6015047051155,41.5518405907898,41.7979280830714));
#33073=CARTESIAN_POINT('Ctrl Pts',(-40.5962665425231,41.6792520429083,41.7885032191744));
#33074=CARTESIAN_POINT('Ctrl Pts',(-40.5876545440908,41.8060792189963,41.7755762188468));
#33075=CARTESIAN_POINT('Ctrl Pts',(-40.5790425456584,41.9329063950843,41.7626492185191));
#33076=CARTESIAN_POINT('Ctrl Pts',(-40.567056721113,42.0591491497169,41.7462200964266));
#33077=CARTESIAN_POINT('Ctrl Pts',(-40.5517320295636,42.1844372677281,41.7263368305228));
#33078=CARTESIAN_POINT('Ctrl Pts',(-40.5364073380141,42.3097253857393,41.7064535646191));
#33079=CARTESIAN_POINT('Ctrl Pts',(-40.5177437968734,42.4340587234487,41.6831161775353));
#33080=CARTESIAN_POINT('Ctrl Pts',(-40.4957959345014,42.5570726384864,41.6563928932872));
#33081=CARTESIAN_POINT('Ctrl Pts',(-40.473828566128,42.6801958812373,41.6296458589165));
#33082=CARTESIAN_POINT('Ctrl Pts',(-40.4485710611385,42.8019972136734,41.5995069368439));
#33083=CARTESIAN_POINT('Ctrl Pts',(-40.420097395835,42.9221187503367,41.5660644338022));
#33084=CARTESIAN_POINT('Ctrl Pts',(-39.2191560456546,37.3678525356093,40.6435409735397));
#33085=CARTESIAN_POINT('Ctrl Pts',(-39.289634570114,37.4511005411706,40.7144304990469));
#33086=CARTESIAN_POINT('Ctrl Pts',(-39.3579239195882,37.5382500908353,40.7829146422872));
#33087=CARTESIAN_POINT('Ctrl Pts',(-39.423816267808,37.6290359607303,40.848784984172));
#33088=CARTESIAN_POINT('Ctrl Pts',(-39.4897086160278,37.7198218306253,40.9146553260567));
#33089=CARTESIAN_POINT('Ctrl Pts',(-39.5532038814973,37.8142439084663,40.9779117851173));
#33090=CARTESIAN_POINT('Ctrl Pts',(-39.614108827874,37.9120148377575,41.0383618517751));
#33091=CARTESIAN_POINT('Ctrl Pts',(-39.6750137742507,38.0097857670486,41.0988119184329));
#33092=CARTESIAN_POINT('Ctrl Pts',(-39.7333283262069,38.1109054268666,41.156455517923));
#33093=CARTESIAN_POINT('Ctrl Pts',(-39.7888750139637,38.2150660778376,41.2111172223887));
#33094=CARTESIAN_POINT('Ctrl Pts',(-39.8444217017204,38.3192267288085,41.2657789268544));
#33095=CARTESIAN_POINT('Ctrl Pts',(-39.8972004565773,38.4264282421062,41.3174586686899));
#33096=CARTESIAN_POINT('Ctrl Pts',(-39.9470506559512,38.5363443693372,41.365999169959));
#33097=CARTESIAN_POINT('Ctrl Pts',(-39.9969008553251,38.6462604965682,41.4145396712281));
#33098=CARTESIAN_POINT('Ctrl Pts',(-40.043822437561,38.7588911017878,41.4599408718959));
#33099=CARTESIAN_POINT('Ctrl Pts',(-40.0876726053202,38.8738934141444,41.5020646016294));
#33100=CARTESIAN_POINT('Ctrl Pts',(-40.1315227730794,38.988895726501,41.544188331363));
#33101=CARTESIAN_POINT('Ctrl Pts',(-40.1723014721277,39.1062696037593,41.5830345380635));
#33102=CARTESIAN_POINT('Ctrl Pts',(-40.2098845998788,39.2256578397782,41.6184850003352));
#33103=CARTESIAN_POINT('Ctrl Pts',(-40.2474677276301,39.345046075797,41.6539354626069));
#33104=CARTESIAN_POINT('Ctrl Pts',(-40.2818552376011,39.4664485229166,41.6859901366046));
#33105=CARTESIAN_POINT('Ctrl Pts',(-40.3129424776325,39.589495714773,41.7145514697324));
#33106=CARTESIAN_POINT('Ctrl Pts',(-40.3440297176639,39.7125429066293,41.7431128028603));
#33107=CARTESIAN_POINT('Ctrl Pts',(-40.3718166493068,39.837234691037,41.7681807597935));
#33108=CARTESIAN_POINT('Ctrl Pts',(-40.3962187080664,39.96319159113,41.7896790507446));
#33109=CARTESIAN_POINT('Ctrl Pts',(-40.420620766826,40.0891484912228,41.8111773416957));
#33110=CARTESIAN_POINT('Ctrl Pts',(-40.4416379225217,40.2163703512169,41.8291059400754));
#33111=CARTESIAN_POINT('Ctrl Pts',(-40.4592062132462,40.3444699944187,41.8434102834412));
#33112=CARTESIAN_POINT('Ctrl Pts',(-40.4767745039706,40.4725696376205,41.8577146268069));
#33113=CARTESIAN_POINT('Ctrl Pts',(-40.4908939079951,40.601546905596,41.8683946974671));
#33114=CARTESIAN_POINT('Ctrl Pts',(-40.5015214554703,40.7310092793855,41.8754179925605));
#33115=CARTESIAN_POINT('Ctrl Pts',(-40.5121490029456,40.8604716531751,41.882441287654));
#33116=CARTESIAN_POINT('Ctrl Pts',(-40.5192846807273,40.9904189726592,41.8858077984942));
#33117=CARTESIAN_POINT('Ctrl Pts',(-40.5229067726725,41.120455766702,41.8855072797153));
#33118=CARTESIAN_POINT('Ctrl Pts',(-40.5265288646176,41.2504925607449,41.8852067609363));
#33119=CARTESIAN_POINT('Ctrl Pts',(-40.5266373662463,41.3806186685165,41.8812392129097));
#33120=CARTESIAN_POINT('Ctrl Pts',(-40.5232319473535,41.5104380747713,41.8736167101495));
#33121=CARTESIAN_POINT('Ctrl Pts',(-40.5198265284606,41.6402574810262,41.8659942073892));
#33122=CARTESIAN_POINT('Ctrl Pts',(-40.5129071932581,41.7697700252033,41.8547167593229));
#33123=CARTESIAN_POINT('Ctrl Pts',(-40.5024949994896,41.8985815593266,41.8398186868216));
#33124=CARTESIAN_POINT('Ctrl Pts',(-40.4920828057211,42.02739309345,41.8249206143203));
#33125=CARTESIAN_POINT('Ctrl Pts',(-40.4781777662645,42.155503458205,41.8064019358099));
#33126=CARTESIAN_POINT('Ctrl Pts',(-40.4608221985893,42.2825227728951,41.7843190095351));
#33127=CARTESIAN_POINT('Ctrl Pts',(-40.4434666309142,42.4095420875853,41.7622360832603));
#33128=CARTESIAN_POINT('Ctrl Pts',(-40.422660556486,42.5354701951125,41.7365889365334));
#33129=CARTESIAN_POINT('Ctrl Pts',(-40.3984672948247,42.6599238560849,41.7074556218011));
#33130=CARTESIAN_POINT('Ctrl Pts',(-40.3742525315798,42.7844881243341,41.6782964150494));
#33131=CARTESIAN_POINT('Ctrl Pts',(-40.3466445877264,42.9075751698582,41.6456448770227));
#33132=CARTESIAN_POINT('Ctrl Pts',(-40.3157276232668,43.0288097293944,41.6096005440156));
#33133=CARTESIAN_POINT('Ctrl Pts',(-39.1403127743034,37.3702233830122,40.7191429622998));
#33134=CARTESIAN_POINT('Ctrl Pts',(-39.2120859602839,37.4549645664739,40.7912762180353));
#33135=CARTESIAN_POINT('Ctrl Pts',(-39.2815913497389,37.5437474062381,40.8609177053995));
#33136=CARTESIAN_POINT('Ctrl Pts',(-39.3486099625915,37.6362921964208,40.9278480088668));
#33137=CARTESIAN_POINT('Ctrl Pts',(-39.4156285754441,37.7288369866036,40.9947783123341));
#33138=CARTESIAN_POINT('Ctrl Pts',(-39.4801603229556,37.8251436046857,41.0589973432769));
#33139=CARTESIAN_POINT('Ctrl Pts',(-39.542001884648,37.9249086538123,41.1203027589764));
#33140=CARTESIAN_POINT('Ctrl Pts',(-39.6038434463403,38.0246737029389,41.1816081746759));
#33141=CARTESIAN_POINT('Ctrl Pts',(-39.6629947403206,38.1278970510403,41.2399998939428));
#33142=CARTESIAN_POINT('Ctrl Pts',(-39.719269385963,38.2342535204814,41.2952939210061));
#33143=CARTESIAN_POINT('Ctrl Pts',(-39.7755440316054,38.3406099899225,41.3505879480694));
#33144=CARTESIAN_POINT('Ctrl Pts',(-39.8289419543779,38.450099439914,41.4027842096886));
#33145=CARTESIAN_POINT('Ctrl Pts',(-39.8792948871678,38.5623769593085,41.4517182157338));
#33146=CARTESIAN_POINT('Ctrl Pts',(-39.9296478199576,38.6746544787031,41.500652221779));
#33147=CARTESIAN_POINT('Ctrl Pts',(-39.9769556960625,38.7897199188775,41.5463239074193));
#33148=CARTESIAN_POINT('Ctrl Pts',(-40.0210694215682,38.9072108066439,41.5885893241219));
#33149=CARTESIAN_POINT('Ctrl Pts',(-40.0651831470738,39.0247016944102,41.6308547408246));
#33150=CARTESIAN_POINT('Ctrl Pts',(-40.1061026635273,39.1446178742459,41.6697138325762));
#33151=CARTESIAN_POINT('Ctrl Pts',(-40.1436989892561,39.2665815929409,41.7050440991433));
#33152=CARTESIAN_POINT('Ctrl Pts',(-40.1812953149849,39.3885453116359,41.7403743657104));
#33153=CARTESIAN_POINT('Ctrl Pts',(-40.2155684001534,39.5125564077462,41.7721757602493));
#33154=CARTESIAN_POINT('Ctrl Pts',(-40.2464101878252,39.6382242262525,41.8003480025693));
#33155=CARTESIAN_POINT('Ctrl Pts',(-40.2772519754969,39.7638920447589,41.8285202448892));
#33156=CARTESIAN_POINT('Ctrl Pts',(-40.3046624247669,39.8912164193113,41.853063297611));
#33157=CARTESIAN_POINT('Ctrl Pts',(-40.328555084267,40.0197962525337,41.8738997325141));
#33158=CARTESIAN_POINT('Ctrl Pts',(-40.3524477437671,40.1483760857561,41.8947361674171));
#33159=CARTESIAN_POINT('Ctrl Pts',(-40.3728225817804,40.2782112074384,41.9118659568223));
#33160=CARTESIAN_POINT('Ctrl Pts',(-40.389615297392,40.4088926030714,41.9252350126137));
#33161=CARTESIAN_POINT('Ctrl Pts',(-40.4064080130036,40.5395739987043,41.938604068405));
#33162=CARTESIAN_POINT('Ctrl Pts',(-40.4196185838847,40.6711014952883,41.9482123727777));
#33163=CARTESIAN_POINT('Ctrl Pts',(-40.4292052650816,40.8030607362945,41.9540295189884));
#33164=CARTESIAN_POINT('Ctrl Pts',(-40.4387919462785,40.9350199773008,41.9598466651991));
#33165=CARTESIAN_POINT('Ctrl Pts',(-40.4447547249909,41.0674107880283,41.9618726454296));
#33166=CARTESIAN_POINT('Ctrl Pts',(-40.4470746758031,41.199816078738,41.9601009265594));
#33167=CARTESIAN_POINT('Ctrl Pts',(-40.4493946266152,41.3322213694475,41.9583292076891));
#33168=CARTESIAN_POINT('Ctrl Pts',(-40.4480717463362,41.4646409648356,41.9527597919361));
#33169=CARTESIAN_POINT('Ctrl Pts',(-40.4431100490709,41.5966576680492,41.9434100618216));
#33170=CARTESIAN_POINT('Ctrl Pts',(-40.4381483518057,41.7286743712627,41.9340603317071));
#33171=CARTESIAN_POINT('Ctrl Pts',(-40.429547843993,41.8602880074982,41.9209302994716));
#33172=CARTESIAN_POINT('Ctrl Pts',(-40.4173354548884,41.9910838996568,41.9040611547965));
#33173=CARTESIAN_POINT('Ctrl Pts',(-40.4051230657838,42.1218797918155,41.8871920101214));
#33174=CARTESIAN_POINT('Ctrl Pts',(-40.3892988114159,42.2518577666931,41.8665837751932));
#33175=CARTESIAN_POINT('Ctrl Pts',(-40.3699123676151,42.3806082780621,41.8423011885474));
#33176=CARTESIAN_POINT('Ctrl Pts',(-40.3505259238143,42.5093587894312,41.8180186019016));
#33177=CARTESIAN_POINT('Ctrl Pts',(-40.3275773160987,42.6368816667763,41.7900616955314));
#33178=CARTESIAN_POINT('Ctrl Pts',(-40.301138655148,42.7627750736833,41.7585183503151));
#33179=CARTESIAN_POINT('Ctrl Pts',(-40.2746764970317,42.8887803674308,41.7269469711824));
#33180=CARTESIAN_POINT('Ctrl Pts',(-40.2447181143144,43.0131531260429,41.6917828172015));
#33181=CARTESIAN_POINT('Ctrl Pts',(-40.2113578506985,43.1355007084522,41.6531366542289));
#33182=CARTESIAN_POINT('Ctrl Pts',(-39.0614979606134,37.3726274522223,40.794772939012));
#33183=CARTESIAN_POINT('Ctrl Pts',(-39.1345566113031,37.4588431187849,40.8681279710931));
#33184=CARTESIAN_POINT('Ctrl Pts',(-39.2052676996424,37.5492425921423,40.9389035914507));
#33185=CARTESIAN_POINT('Ctrl Pts',(-39.2734006183025,37.6435310639275,41.0068689724951));
#33186=CARTESIAN_POINT('Ctrl Pts',(-39.3415335369625,37.7378195357127,41.0748343535394));
#33187=CARTESIAN_POINT('Ctrl Pts',(-39.4070881892784,37.8359968721725,41.1399893988339));
#33188=CARTESIAN_POINT('Ctrl Pts',(-39.4698507733057,37.9377429133658,41.2021215990047));
#33189=CARTESIAN_POINT('Ctrl Pts',(-39.532613357333,38.039488954559,41.2642537991755));
#33190=CARTESIAN_POINT('Ctrl Pts',(-39.5925837840149,38.1448035561639,41.3233630660502));
#33191=CARTESIAN_POINT('Ctrl Pts',(-39.6495664502885,38.2533432931017,41.3792565936186));
#33192=CARTESIAN_POINT('Ctrl Pts',(-39.706549116562,38.3618830300396,41.435150121187));
#33193=CARTESIAN_POINT('Ctrl Pts',(-39.7605439415582,38.4736477483594,41.4878278301146));
#33194=CARTESIAN_POINT('Ctrl Pts',(-39.8113747960734,38.5882729958286,41.537117874583));
#33195=CARTESIAN_POINT('Ctrl Pts',(-39.8622056505885,38.7028982432979,41.5864079190514));
#33196=CARTESIAN_POINT('Ctrl Pts',(-39.909872462468,38.8203838573381,41.6323102290807));
#33197=CARTESIAN_POINT('Ctrl Pts',(-39.9542197245262,38.9403467335296,41.6746750393716));
#33198=CARTESIAN_POINT('Ctrl Pts',(-39.9985669865844,39.060309609721,41.7170398496625));
#33199=CARTESIAN_POINT('Ctrl Pts',(-40.0395946358509,39.1827495779158,41.7558671000453));
#33200=CARTESIAN_POINT('Ctrl Pts',(-40.0771688010238,39.3072673780001,41.7910300822715));
#33201=CARTESIAN_POINT('Ctrl Pts',(-40.1147429661966,39.4317851780843,41.8261930644977));
#33202=CARTESIAN_POINT('Ctrl Pts',(-40.1488635938993,39.5583806334479,41.8576917285996));
#33203=CARTESIAN_POINT('Ctrl Pts',(-40.1794193216837,39.6866409300556,41.8854232497566));
#33204=CARTESIAN_POINT('Ctrl Pts',(-40.209975049468,39.8149012266631,41.9131547709135));
#33205=CARTESIAN_POINT('Ctrl Pts',(-40.2369658338992,39.9448261825921,41.9371191096854));
#33206=CARTESIAN_POINT('Ctrl Pts',(-40.2603035477718,40.0759921200064,41.9572379955189));
#33207=CARTESIAN_POINT('Ctrl Pts',(-40.2836412616445,40.2071580574208,41.9773568813524));
#33208=CARTESIAN_POINT('Ctrl Pts',(-40.3033258717486,40.339564790269,41.9936302855921));
#33209=CARTESIAN_POINT('Ctrl Pts',(-40.3192930611983,40.4727805378766,42.006005002883));
#33210=CARTESIAN_POINT('Ctrl Pts',(-40.3352602506479,40.6059962854843,42.0183797201739));
#33211=CARTESIAN_POINT('Ctrl Pts',(-40.3475099966744,40.740020858882,42.0268557328322));
#33212=CARTESIAN_POINT('Ctrl Pts',(-40.3560022127269,40.8744171883912,42.0314052483924));
#33213=CARTESIAN_POINT('Ctrl Pts',(-40.3644944287794,41.0088135179004,42.0359547639526));
#33214=CARTESIAN_POINT('Ctrl Pts',(-40.3692291026792,41.1435814128636,42.036577775818));
#33215=CARTESIAN_POINT('Ctrl Pts',(-40.3701906404258,41.2782813629928,42.0332720865946));
#33216=CARTESIAN_POINT('Ctrl Pts',(-40.3711521781724,41.412981313122,42.0299663973711));
#33217=CARTESIAN_POINT('Ctrl Pts',(-40.3683405782567,41.5476131273126,42.0227320115925));
#33218=CARTESIAN_POINT('Ctrl Pts',(-40.3617648419301,41.6817377190824,42.0115923424155));
#33219=CARTESIAN_POINT('Ctrl Pts',(-40.3551891056035,41.8158623108523,42.0004526732384));
#33220=CARTESIAN_POINT('Ctrl Pts',(-40.3448492420369,41.9494794898936,41.9854077362983));
#33221=CARTESIAN_POINT('Ctrl Pts',(-40.330778790245,42.0821534553238,41.9665064039702));
#33222=CARTESIAN_POINT('Ctrl Pts',(-40.3167083384531,42.2148274207539,41.947605071642));
#33223=CARTESIAN_POINT('Ctrl Pts',(-40.2989073182277,42.3465579843004,41.9248473705619));
#33224=CARTESIAN_POINT('Ctrl Pts',(-40.2774335890346,42.476915471224,41.898307315156));
#33225=CARTESIAN_POINT('Ctrl Pts',(-40.2559598598415,42.6072729581475,41.8717672597502));
#33226=CARTESIAN_POINT('Ctrl Pts',(-40.2308134519652,42.7362571834365,41.8414448874824));
#33227=CARTESIAN_POINT('Ctrl Pts',(-40.2020761695918,42.8634473992982,41.8074388738828));
#33228=CARTESIAN_POINT('Ctrl Pts',(-40.1733133471698,42.9907506545297,41.7734026376885));
#33229=CARTESIAN_POINT('Ctrl Pts',(-40.1409533053408,43.1162565292245,41.7356762577682));
#33230=CARTESIAN_POINT('Ctrl Pts',(-40.1051015420806,43.2395548537019,41.6943827565721));
#33231=CARTESIAN_POINT('Ctrl Pts',(-38.9827210478865,37.375075767461,40.8704401911112));
#33232=CARTESIAN_POINT('Ctrl Pts',(-39.0570601865467,37.4627511375271,40.9449975555894));
#33233=CARTESIAN_POINT('Ctrl Pts',(-39.1289707770862,37.554754637862,41.0168865246252));
#33234=CARTESIAN_POINT('Ctrl Pts',(-39.1982100815384,37.650775705829,41.0858644332364));
#33235=CARTESIAN_POINT('Ctrl Pts',(-39.2674493859905,37.746796773796,41.1548423418474));
#33236=CARTESIAN_POINT('Ctrl Pts',(-39.3340172989842,37.8468352632664,41.2209090850606));
#33237=CARTESIAN_POINT('Ctrl Pts',(-39.3976891170407,37.9505534890766,41.283841651122));
#33238=CARTESIAN_POINT('Ctrl Pts',(-39.4613609350971,38.0542717148869,41.3467742171832));
#33239=CARTESIAN_POINT('Ctrl Pts',(-39.5221365613181,38.1616695191946,41.4065725103194));
#33240=CARTESIAN_POINT('Ctrl Pts',(-39.5798108443924,38.272384375083,41.4630346782584));
#33241=CARTESIAN_POINT('Ctrl Pts',(-39.6374851274667,38.3830992309714,41.5194968461974));
#33242=CARTESIAN_POINT('Ctrl Pts',(-39.6920579796234,38.4971309699505,41.5726228030128));
#33243=CARTESIAN_POINT('Ctrl Pts',(-39.7433451873401,38.6140946719095,41.6222332192534));
#33244=CARTESIAN_POINT('Ctrl Pts',(-39.7946323950568,38.7310583738686,41.6718436354939));
#33245=CARTESIAN_POINT('Ctrl Pts',(-39.8426338802826,38.8509538608077,41.7179384356605));
#33246=CARTESIAN_POINT('Ctrl Pts',(-39.8871876114888,38.9733764192277,41.7603620243398));
#33247=CARTESIAN_POINT('Ctrl Pts',(-39.9317413426949,39.0957989776476,41.802785613019));
#33248=CARTESIAN_POINT('Ctrl Pts',(-39.9728472520778,39.220748421241,41.8415379256489));
#33249=CARTESIAN_POINT('Ctrl Pts',(-40.0103665844861,39.3478029766131,41.8764881517675));
#33250=CARTESIAN_POINT('Ctrl Pts',(-40.0478859168944,39.4748575319852,41.911438377886));
#33251=CARTESIAN_POINT('Ctrl Pts',(-40.0818186152298,39.6040170057794,41.9425864643046));
#33252=CARTESIAN_POINT('Ctrl Pts',(-40.1120501378908,39.7348454134234,41.9698272690252));
#33253=CARTESIAN_POINT('Ctrl Pts',(-40.1422816605518,39.8656738210674,41.9970680737459));
#33254=CARTESIAN_POINT('Ctrl Pts',(-40.168811961531,39.9981709634615,42.0204015553124));
#33255=CARTESIAN_POINT('Ctrl Pts',(-40.191551486407,40.1318895895581,42.039748950335));
#33256=CARTESIAN_POINT('Ctrl Pts',(-40.2142910112829,40.2656082156547,42.0590963453575));
#33257=CARTESIAN_POINT('Ctrl Pts',(-40.2332397254499,40.4005481219555,42.0744576243926));
#33258=CARTESIAN_POINT('Ctrl Pts',(-40.2483336665301,40.5362538117355,42.0857809346378));
#33259=CARTESIAN_POINT('Ctrl Pts',(-40.2634276076103,40.6719595015155,42.0971042448829));
#33260=CARTESIAN_POINT('Ctrl Pts',(-40.2746667526333,40.8084307682524,42.104389569106));
#33261=CARTESIAN_POINT('Ctrl Pts',(-40.2820131632761,40.9452069460336,42.1076123153132));
#33262=CARTESIAN_POINT('Ctrl Pts',(-40.2893595739188,41.0819831238149,42.1108350615203));
#33263=CARTESIAN_POINT('Ctrl Pts',(-40.2928132390013,41.2190640044892,42.1099952248072));
#33264=CARTESIAN_POINT('Ctrl Pts',(-40.2923625004959,41.3559868643603,42.1050956400864));
#33265=CARTESIAN_POINT('Ctrl Pts',(-40.2919117619906,41.4929097242314,42.1001960553657));
#33266=CARTESIAN_POINT('Ctrl Pts',(-40.2875566205834,41.6296743549245,42.0912367300939));
#33267=CARTESIAN_POINT('Ctrl Pts',(-40.2793117772825,41.765819100262,42.0782479069429));
#33268=CARTESIAN_POINT('Ctrl Pts',(-40.2710669339815,41.9019638455995,42.0652590837918));
#33269=CARTESIAN_POINT('Ctrl Pts',(-40.2589324013341,42.0374884983907,42.0482407825286));
#33270=CARTESIAN_POINT('Ctrl Pts',(-40.242949140091,42.1719355880683,42.0272504493207));
#33271=CARTESIAN_POINT('Ctrl Pts',(-40.2269658788481,42.3063826777458,42.0062601161129));
#33272=CARTESIAN_POINT('Ctrl Pts',(-40.2071339133334,42.4397519997028,41.9812977829045));
#33273=CARTESIAN_POINT('Ctrl Pts',(-40.1835201873859,42.5715933588039,41.9524477113593));
#33274=CARTESIAN_POINT('Ctrl Pts',(-40.1599064614385,42.7034347179049,41.9235976398141));
#33275=CARTESIAN_POINT('Ctrl Pts',(-40.1325110109945,42.8337479135088,41.8908598738373));
#33276=CARTESIAN_POINT('Ctrl Pts',(-40.1014263108327,42.9620930665946,41.8543449214736));
#33277=CARTESIAN_POINT('Ctrl Pts',(-40.070313984372,43.0905522854922,41.8177975167142));
#33278=CARTESIAN_POINT('Ctrl Pts',(-40.0355058950823,43.2170397664827,41.77746626436));
#33279=CARTESIAN_POINT('Ctrl Pts',(-39.9971197373371,43.3411277792636,41.7334875353997));
#33280=CARTESIAN_POINT('Ctrl Pts',(-38.9039441351597,37.3775240826997,40.9461074432104));
#33281=CARTESIAN_POINT('Ctrl Pts',(-38.9795637617903,37.4666591562693,41.0218671400858));
#33282=CARTESIAN_POINT('Ctrl Pts',(-39.05267385453,37.5602666835818,41.0948694577997));
#33283=CARTESIAN_POINT('Ctrl Pts',(-39.1230195447743,37.6580203477305,41.1648598939777));
#33284=CARTESIAN_POINT('Ctrl Pts',(-39.1933652350185,37.7557740118792,41.2348503301556));
#33285=CARTESIAN_POINT('Ctrl Pts',(-39.26094640869,37.8576736543604,41.3018287712874));
#33286=CARTESIAN_POINT('Ctrl Pts',(-39.3255274607756,37.9633640647876,41.3655617032392));
#33287=CARTESIAN_POINT('Ctrl Pts',(-39.3901085128612,38.0690544752149,41.429294635191));
#33288=CARTESIAN_POINT('Ctrl Pts',(-39.4516893386213,38.1785354822252,41.4897819545887));
#33289=CARTESIAN_POINT('Ctrl Pts',(-39.5100552384964,38.2914254570642,41.5468127628983));
#33290=CARTESIAN_POINT('Ctrl Pts',(-39.5684211383714,38.4043154319032,41.6038435712078));
#33291=CARTESIAN_POINT('Ctrl Pts',(-39.6235720176885,38.5206141915416,41.657417775911));
#33292=CARTESIAN_POINT('Ctrl Pts',(-39.6753155786067,38.6399163479905,41.7073485639237));
#33293=CARTESIAN_POINT('Ctrl Pts',(-39.727059139525,38.7592185044393,41.7572793519365));
#33294=CARTESIAN_POINT('Ctrl Pts',(-39.7753952980973,38.8815238642774,41.8035666422404));
#33295=CARTESIAN_POINT('Ctrl Pts',(-39.8201554984513,39.0064061049258,41.846049009308));
#33296=CARTESIAN_POINT('Ctrl Pts',(-39.8649156988054,39.1312883455742,41.8885313763755));
#33297=CARTESIAN_POINT('Ctrl Pts',(-39.9060998683047,39.2587472645661,41.9272087512526));
#33298=CARTESIAN_POINT('Ctrl Pts',(-39.9435643679485,39.388338575226,41.9619462212635));
#33299=CARTESIAN_POINT('Ctrl Pts',(-39.9810288675922,39.517929885886,41.9966836912744));
#33300=CARTESIAN_POINT('Ctrl Pts',(-40.0147736365603,39.6496533781108,42.0274812000097));
#33301=CARTESIAN_POINT('Ctrl Pts',(-40.044680954098,39.7830498967912,42.0542312882939));
#33302=CARTESIAN_POINT('Ctrl Pts',(-40.0745882716357,39.9164464154717,42.0809813765782));
#33303=CARTESIAN_POINT('Ctrl Pts',(-40.1006580891627,40.0515157443309,42.1036840009393));
#33304=CARTESIAN_POINT('Ctrl Pts',(-40.122799425042,40.1877870591098,42.1222599051509));
#33305=CARTESIAN_POINT('Ctrl Pts',(-40.1449407609214,40.3240583738885,42.1408358093627));
#33306=CARTESIAN_POINT('Ctrl Pts',(-40.1631535791511,40.461531453642,42.1552849631931));
#33307=CARTESIAN_POINT('Ctrl Pts',(-40.1773742718619,40.5997270855943,42.1655568663926));
#33308=CARTESIAN_POINT('Ctrl Pts',(-40.1915949645728,40.7379227175466,42.175828769592));
#33309=CARTESIAN_POINT('Ctrl Pts',(-40.2018235085922,40.8768406776228,42.1819234053797));
#33310=CARTESIAN_POINT('Ctrl Pts',(-40.2080241138252,41.0159967036761,42.1838193822339));
#33311=CARTESIAN_POINT('Ctrl Pts',(-40.2142247190582,41.1551527297295,42.185715359088));
#33312=CARTESIAN_POINT('Ctrl Pts',(-40.2163973753233,41.2945465961149,42.1834126737962));
#33313=CARTESIAN_POINT('Ctrl Pts',(-40.214534360566,41.4336923657278,42.1769191935783));
#33314=CARTESIAN_POINT('Ctrl Pts',(-40.2126713458088,41.5728381353406,42.1704257133604));
#33315=CARTESIAN_POINT('Ctrl Pts',(-40.2067726629101,41.7117355825366,42.1597414485952));
#33316=CARTESIAN_POINT('Ctrl Pts',(-40.1968587126348,41.8499004814415,42.1449034714703));
#33317=CARTESIAN_POINT('Ctrl Pts',(-40.1869447623595,41.9880653803465,42.1300654943453));
#33318=CARTESIAN_POINT('Ctrl Pts',(-40.1730155606313,42.1254975068878,42.1110738287589));
#33319=CARTESIAN_POINT('Ctrl Pts',(-40.1551194899372,42.2617177208127,42.0879944946714));
#33320=CARTESIAN_POINT('Ctrl Pts',(-40.137223419243,42.3979379347377,42.0649151605838));
#33321=CARTESIAN_POINT('Ctrl Pts',(-40.1153605084391,42.5329460151051,42.0377481952471));
#33322=CARTESIAN_POINT('Ctrl Pts',(-40.0896067857373,42.6662712463838,42.0065881075625));
#33323=CARTESIAN_POINT('Ctrl Pts',(-40.0638530630355,42.7995964776624,41.9754280198779));
#33324=CARTESIAN_POINT('Ctrl Pts',(-40.0342085700239,42.931238643581,41.9402748601922));
#33325=CARTESIAN_POINT('Ctrl Pts',(-40.0007764520737,43.060738733891,41.9012509690643));
#33326=CARTESIAN_POINT('Ctrl Pts',(-39.9673146215742,43.1903539164548,41.8621923957399));
#33327=CARTESIAN_POINT('Ctrl Pts',(-39.9300584848238,43.317823003741,41.8192562709516));
#33328=CARTESIAN_POINT('Ctrl Pts',(-39.8891379325936,43.4427007048253,41.7725923142273));
#33329=CARTESIAN_POINT('Ctrl Pts',(-38.8252050953863,37.3800166112679,41.0218119431493));
#33330=CARTESIAN_POINT('Ctrl Pts',(-38.9021002180776,37.4705965953422,41.0987545205423));
#33331=CARTESIAN_POINT('Ctrl Pts',(-38.9764036011982,37.5657955295521,41.1728493947268));
#33332=CARTESIAN_POINT('Ctrl Pts',(-39.0478477421773,37.6652706909476,41.2438298005602));
#33333=CARTESIAN_POINT('Ctrl Pts',(-39.1192918831564,37.764745852343,41.3148102063937));
#33334=CARTESIAN_POINT('Ctrl Pts',(-39.1878766584313,37.8684970689033,41.3826760211015));
#33335=CARTESIAN_POINT('Ctrl Pts',(-39.2533551414358,37.9761508429034,41.4471828923901));
#33336=CARTESIAN_POINT('Ctrl Pts',(-39.3188336244404,38.0838046169035,41.5116897636787));
#33337=CARTESIAN_POINT('Ctrl Pts',(-39.3812057019163,38.1953607621915,41.5728375799556));
#33338=CARTESIAN_POINT('Ctrl Pts',(-39.440246800283,38.3104176938053,41.6304061603406));
#33339=CARTESIAN_POINT('Ctrl Pts',(-39.4992878986496,38.4254746254192,41.6879747407256));
#33340=CARTESIAN_POINT('Ctrl Pts',(-39.5549979157674,38.5440321444137,41.7419639856107));
#33341=CARTESIAN_POINT('Ctrl Pts',(-39.6071762472742,38.6656634681541,41.7921794702661));
#33342=CARTESIAN_POINT('Ctrl Pts',(-39.6593545787809,38.7872947918946,41.8423949549214));
#33343=CARTESIAN_POINT('Ctrl Pts',(-39.7080011343898,38.9119997100725,41.8888365924393));
#33344=CARTESIAN_POINT('Ctrl Pts',(-39.7529407228233,39.0393293132054,41.9313371137559));
#33345=CARTESIAN_POINT('Ctrl Pts',(-39.7978803112568,39.1666589163385,41.9738376350724));
#33346=CARTESIAN_POINT('Ctrl Pts',(-39.8391128547301,39.2966129842659,42.0123969666053));
#33347=CARTESIAN_POINT('Ctrl Pts',(-39.8764898361686,39.4287237106721,42.046876199188));
#33348=CARTESIAN_POINT('Ctrl Pts',(-39.913866817607,39.5608344370783,42.0813554317706));
#33349=CARTESIAN_POINT('Ctrl Pts',(-39.9473881722875,39.6951015935328,42.1117545056753));
#33350=CARTESIAN_POINT('Ctrl Pts',(-39.976933126641,39.8310418428766,42.1379638719202));
#33351=CARTESIAN_POINT('Ctrl Pts',(-40.0064780809946,39.9669820922203,42.1641732381651));
#33352=CARTESIAN_POINT('Ctrl Pts',(-40.0320465838252,40.1045951993949,42.1861928513067));
#33353=CARTESIAN_POINT('Ctrl Pts',(-40.0535464748672,40.243385774172,42.2039433116964));
#33354=CARTESIAN_POINT('Ctrl Pts',(-40.0750463659091,40.3821763489492,42.2216937720859));
#33355=CARTESIAN_POINT('Ctrl Pts',(-40.0924776078616,40.5221441513319,42.2351750488915));
#33356=CARTESIAN_POINT('Ctrl Pts',(-40.1057773177963,40.6627853025867,42.2443384641273));
#33357=CARTESIAN_POINT('Ctrl Pts',(-40.1190770277309,40.8034264538415,42.2535018793631));
#33358=CARTESIAN_POINT('Ctrl Pts',(-40.1282451825109,40.9447407107577,42.2583474170307));
#33359=CARTESIAN_POINT('Ctrl Pts',(-40.1332486300361,41.0862193318304,42.258857472199));
#33360=CARTESIAN_POINT('Ctrl Pts',(-40.1382520775612,41.2276979529032,42.2593675273673));
#33361=CARTESIAN_POINT('Ctrl Pts',(-40.1390908090258,41.3693406934561,42.2555420989869));
#33362=CARTESIAN_POINT('Ctrl Pts',(-40.1357616428395,41.5106376100576,42.2473947830991));
#33363=CARTESIAN_POINT('Ctrl Pts',(-40.1324324766533,41.651934526659,42.2392474672111));
#33364=CARTESIAN_POINT('Ctrl Pts',(-40.1249354184051,41.7928853749258,42.2267782777238));
#33365=CARTESIAN_POINT('Ctrl Pts',(-40.1132972811551,41.9329826791417,42.2100319151659));
#33366=CARTESIAN_POINT('Ctrl Pts',(-40.101659143905,42.0730799833576,42.1932855526079));
#33367=CARTESIAN_POINT('Ctrl Pts',(-40.0858799475973,42.2123235011892,42.1722620457457));
#33368=CARTESIAN_POINT('Ctrl Pts',(-40.0660163083583,42.3502118766985,42.1470368793923));
#33369=CARTESIAN_POINT('Ctrl Pts',(-40.0461526691193,42.4881002522078,42.121811713039));
#33370=CARTESIAN_POINT('Ctrl Pts',(-40.0222046211057,42.6246332468531,42.0923849306128));
#33371=CARTESIAN_POINT('Ctrl Pts',(-39.9942581775686,42.759319232706,42.0588622595791));
#33372=CARTESIAN_POINT('Ctrl Pts',(-39.9663117340315,42.8940052185588,42.0253395885454));
#33373=CARTESIAN_POINT('Ctrl Pts',(-39.9343669430954,43.0268439625842,41.9877210866631));
#33374=CARTESIAN_POINT('Ctrl Pts',(-39.8985385977431,43.1573571033234,41.9461419648695));
#33375=CARTESIAN_POINT('Ctrl Pts',(-39.8626784102122,43.2879862366576,41.9045258899368));
#33376=CARTESIAN_POINT('Ctrl Pts',(-39.8229278240937,43.4162854048886,41.8589422238337));
#33377=CARTESIAN_POINT('Ctrl Pts',(-39.7794299686218,43.541791724316,41.8095551265968));
#33378=CARTESIAN_POINT('Ctrl Pts',(-38.7465138697966,37.3825649586746,41.0975634680728));
#33379=CARTESIAN_POINT('Ctrl Pts',(-38.8246834400008,37.4745783163285,41.1756711667335));
#33380=CARTESIAN_POINT('Ctrl Pts',(-38.9001777621614,37.5713594409668,41.2508394067609));
#33381=CARTESIAN_POINT('Ctrl Pts',(-38.9727161601587,37.6725485154566,41.3227887243575));
#33382=CARTESIAN_POINT('Ctrl Pts',(-39.045254558156,37.7737375899464,41.3947380419541));
#33383=CARTESIAN_POINT('Ctrl Pts',(-39.1148368980517,37.8793344274476,41.4634683042695));
#33384=CARTESIAN_POINT('Ctrl Pts',(-39.1812044835543,37.9889464353815,41.5287239829036));
#33385=CARTESIAN_POINT('Ctrl Pts',(-39.2475720690568,38.0985584433153,41.5939796615378));
#33386=CARTESIAN_POINT('Ctrl Pts',(-39.3107247776221,38.2121854192892,41.6557606359997));
#33387=CARTESIAN_POINT('Ctrl Pts',(-39.3704278173254,38.3294049159214,41.7138372142582));
#33388=CARTESIAN_POINT('Ctrl Pts',(-39.4301308570288,38.4466244125535,41.7719137925167));
#33389=CARTESIAN_POINT('Ctrl Pts',(-39.4863841176318,38.5674362134046,41.8262858673365));
#33390=CARTESIAN_POINT('Ctrl Pts',(-39.5389784582816,38.6913911590341,41.8767512918204));
#33391=CARTESIAN_POINT('Ctrl Pts',(-39.5915727989315,38.8153461046634,41.9272167163044));
#33392=CARTESIAN_POINT('Ctrl Pts',(-39.6405081225157,38.9424439661952,41.9737753972707));
#33393=CARTESIAN_POINT('Ctrl Pts',(-39.6856024951302,39.0722122135953,42.0162542368022));
#33394=CARTESIAN_POINT('Ctrl Pts',(-39.7306968677448,39.2019804609954,42.0587330763338));
#33395=CARTESIAN_POINT('Ctrl Pts',(-39.7719502061255,39.3344188546537,42.0971319959957));
#33396=CARTESIAN_POINT('Ctrl Pts',(-39.8092091367918,39.4690350092704,42.1313082345913));
#33397=CARTESIAN_POINT('Ctrl Pts',(-39.8464680674581,39.6036511638872,42.1654844731869));
#33398=CARTESIAN_POINT('Ctrl Pts',(-39.8797325216134,39.7404448309009,42.1954379676116));
#33399=CARTESIAN_POINT('Ctrl Pts',(-39.9088788272033,39.8789074327843,42.221057355443));
#33400=CARTESIAN_POINT('Ctrl Pts',(-39.9380251327931,40.0173700346678,42.2466767432743));
#33401=CARTESIAN_POINT('Ctrl Pts',(-39.9630532360005,40.1575013157574,42.2679619772076));
#33402=CARTESIAN_POINT('Ctrl Pts',(-39.9838700862395,40.2987802897971,42.2848339220615));
#33403=CARTESIAN_POINT('Ctrl Pts',(-40.0046869364786,40.4400592638367,42.3017058669153));
#33404=CARTESIAN_POINT('Ctrl Pts',(-40.0212924953122,40.5824856699626,42.3141644915366));
#33405=CARTESIAN_POINT('Ctrl Pts',(-40.0336250258616,40.7255299890016,42.3221634767014));
#33406=CARTESIAN_POINT('Ctrl Pts',(-40.0459575564109,40.8685743080405,42.3301624618662));
#33407=CARTESIAN_POINT('Ctrl Pts',(-40.0540170359046,41.012236275869,42.3337017928048));
#33408=CARTESIAN_POINT('Ctrl Pts',(-40.0577735004543,41.1559817796882,42.3327683108365));
#33409=CARTESIAN_POINT('Ctrl Pts',(-40.0615299650041,41.2997272835074,42.3318348288682));
#33410=CARTESIAN_POINT('Ctrl Pts',(-40.0609834076738,41.4435560578991,42.3264285357167));
#33411=CARTESIAN_POINT('Ctrl Pts',(-40.0561358604786,41.5869333699035,42.3165695311371));
#33412=CARTESIAN_POINT('Ctrl Pts',(-40.0512883132832,41.730310681908,42.3067105265574));
#33413=CARTESIAN_POINT('Ctrl Pts',(-40.0421397851736,41.8732362667868,42.2923988287537));
#33414=CARTESIAN_POINT('Ctrl Pts',(-40.0287242889509,42.0151787494982,42.2736876463871));
#33415=CARTESIAN_POINT('Ctrl Pts',(-40.0153087927281,42.1571212322096,42.2549764640206));
#33416=CARTESIAN_POINT('Ctrl Pts',(-39.9976263531632,42.2980803506645,42.2318658316403));
#33417=CARTESIAN_POINT('Ctrl Pts',(-39.9757427108098,42.4375320408366,42.2044416709745));
#33418=CARTESIAN_POINT('Ctrl Pts',(-39.9538590684562,42.5769837310087,42.1770175103087));
#33419=CARTESIAN_POINT('Ctrl Pts',(-39.9277742637211,42.7149277354081,42.1452798719946));
#33420=CARTESIAN_POINT('Ctrl Pts',(-39.8975852758416,42.8508511997324,42.1093467516234));
#33421=CARTESIAN_POINT('Ctrl Pts',(-39.8673962879621,42.9867746640567,42.0734136312522));
#33422=CARTESIAN_POINT('Ctrl Pts',(-39.8331031726806,43.1206773373308,42.0332850951724));
#33423=CARTESIAN_POINT('Ctrl Pts',(-39.7948334264531,43.2520613902913,41.989110335025));
#33424=CARTESIAN_POINT('Ctrl Pts',(-39.7565296682699,43.3835622098636,41.9448963148841));
#33425=CARTESIAN_POINT('Ctrl Pts',(-39.7142422783854,43.5125396872975,41.8966289570872));
#33426=CARTESIAN_POINT('Ctrl Pts',(-39.6681287411246,43.6385134433798,41.8444880178527));
#33427=CARTESIAN_POINT('Ctrl Pts',(-38.6678226442069,37.3851133060814,41.1733149929962));
#33428=CARTESIAN_POINT('Ctrl Pts',(-38.7472666619239,37.4785600373149,41.2525878129248));
#33429=CARTESIAN_POINT('Ctrl Pts',(-38.8239519231248,37.5769233523815,41.3288294187951));
#33430=CARTESIAN_POINT('Ctrl Pts',(-38.8975845781402,37.6798263399656,41.4017476481549));
#33431=CARTESIAN_POINT('Ctrl Pts',(-38.9712172331556,37.7827293275497,41.4746658775147));
#33432=CARTESIAN_POINT('Ctrl Pts',(-39.0417971376721,37.890171785992,41.5442605874375));
#33433=CARTESIAN_POINT('Ctrl Pts',(-39.1090538256727,38.0017420278596,41.6102650734172));
#33434=CARTESIAN_POINT('Ctrl Pts',(-39.1763105136732,38.1133122697273,41.6762695593968));
#33435=CARTESIAN_POINT('Ctrl Pts',(-39.2402438533279,38.229010076387,41.7386836920437));
#33436=CARTESIAN_POINT('Ctrl Pts',(-39.3006088343679,38.3483921380374,41.7972682681757));
#33437=CARTESIAN_POINT('Ctrl Pts',(-39.3609738154079,38.4677741996879,41.8558528443076));
#33438=CARTESIAN_POINT('Ctrl Pts',(-39.4177703194962,38.5908402823956,41.9106077490624));
#33439=CARTESIAN_POINT('Ctrl Pts',(-39.4707806692892,38.717118849914,41.9613231133749));
#33440=CARTESIAN_POINT('Ctrl Pts',(-39.5237910190821,38.8433974174324,42.0120384776873));
#33441=CARTESIAN_POINT('Ctrl Pts',(-39.5730151106415,38.972888222318,42.058714202102));
#33442=CARTESIAN_POINT('Ctrl Pts',(-39.6182642674372,39.1050951139852,42.1011713598486));
#33443=CARTESIAN_POINT('Ctrl Pts',(-39.6635134242329,39.2373020056522,42.1436285175952));
#33444=CARTESIAN_POINT('Ctrl Pts',(-39.704787557521,39.3722247250415,42.1818670253862));
#33445=CARTESIAN_POINT('Ctrl Pts',(-39.7419284374151,39.5093463078688,42.2157402699947));
#33446=CARTESIAN_POINT('Ctrl Pts',(-39.7790693173092,39.646467890696,42.2496135146032));
#33447=CARTESIAN_POINT('Ctrl Pts',(-39.8120768709394,39.7857880682689,42.2791214295479));
#33448=CARTESIAN_POINT('Ctrl Pts',(-39.8408245277656,39.9267730226921,42.3041508389658));
#33449=CARTESIAN_POINT('Ctrl Pts',(-39.8695721845917,40.0677579771153,42.3291802483837));
#33450=CARTESIAN_POINT('Ctrl Pts',(-39.8940598881757,40.2104074321199,42.3497311031085));
#33451=CARTESIAN_POINT('Ctrl Pts',(-39.9141936976119,40.3541748054221,42.3657245324266));
#33452=CARTESIAN_POINT('Ctrl Pts',(-39.9343275070481,40.4979421787244,42.3817179617447));
#33453=CARTESIAN_POINT('Ctrl Pts',(-39.9501073827628,40.6428271885933,42.3931539341818));
#33454=CARTESIAN_POINT('Ctrl Pts',(-39.9614727339269,40.7882746754164,42.3999884892756));
#33455=CARTESIAN_POINT('Ctrl Pts',(-39.9728380850908,40.9337221622395,42.4068230443694));
#33456=CARTESIAN_POINT('Ctrl Pts',(-39.9797888892982,41.0797318409803,42.4090561685789));
#33457=CARTESIAN_POINT('Ctrl Pts',(-39.9822983708726,41.225744227546,42.406679149474));
#33458=CARTESIAN_POINT('Ctrl Pts',(-39.9848078524469,41.3717566141116,42.4043021303692));
#33459=CARTESIAN_POINT('Ctrl Pts',(-39.9828760063219,41.517771422342,42.3973149724465));
#33460=CARTESIAN_POINT('Ctrl Pts',(-39.9765100781176,41.6632291297494,42.3857442791751));
#33461=CARTESIAN_POINT('Ctrl Pts',(-39.9701441499132,41.8086868371569,42.3741735859036));
#33462=CARTESIAN_POINT('Ctrl Pts',(-39.9593441519422,41.9535871586478,42.3580193797836));
#33463=CARTESIAN_POINT('Ctrl Pts',(-39.9441512967467,42.0973748198546,42.3373433776084));
#33464=CARTESIAN_POINT('Ctrl Pts',(-39.9289584415512,42.2411624810616,42.3166673754332));
#33465=CARTESIAN_POINT('Ctrl Pts',(-39.9093727587292,42.3838372001397,42.291469617535));
#33466=CARTESIAN_POINT('Ctrl Pts',(-39.8854691132612,42.5248522049747,42.2618464625567));
#33467=CARTESIAN_POINT('Ctrl Pts',(-39.8615654677932,42.6658672098096,42.2322233075785));
#33468=CARTESIAN_POINT('Ctrl Pts',(-39.8333439063365,42.805222223963,42.1981748133764));
#33469=CARTESIAN_POINT('Ctrl Pts',(-39.8009123741146,42.9423831667588,42.1598312436677));
#33470=CARTESIAN_POINT('Ctrl Pts',(-39.7684808418927,43.0795441095547,42.121487673959));
#33471=CARTESIAN_POINT('Ctrl Pts',(-39.7318394022657,43.2145107120774,42.0788491036817));
#33472=CARTESIAN_POINT('Ctrl Pts',(-39.6911282551631,43.3467656772593,42.0320787051806));
#33473=CARTESIAN_POINT('Ctrl Pts',(-39.6503809263276,43.4791381830696,41.9852667398315));
#33474=CARTESIAN_POINT('Ctrl Pts',(-39.605556732677,43.6087939697063,41.9343156903406));
#33475=CARTESIAN_POINT('Ctrl Pts',(-39.5568275136275,43.7352351624437,41.8794209091086));
#33476=CARTESIAN_POINT('Ctrl Pts',(-38.5891792041831,37.3877174389177,41.2491135147587));
#33477=CARTESIAN_POINT('Ctrl Pts',(-38.6698966078566,37.4825859979437,41.3295336941693));
#33478=CARTESIAN_POINT('Ctrl Pts',(-38.7477704437814,37.5825222780497,41.4068294727545));
#33479=CARTESIAN_POINT('Ctrl Pts',(-38.8224931492366,37.6871315856152,41.4806955534571));
#33480=CARTESIAN_POINT('Ctrl Pts',(-38.8972158546918,37.7917408931808,41.5545616341598));
#33481=CARTESIAN_POINT('Ctrl Pts',(-38.968787274099,37.9010230104245,41.6249978631657));
#33482=CARTESIAN_POINT('Ctrl Pts',(-39.0369247236146,38.0145463475696,41.6917260218454));
#33483=CARTESIAN_POINT('Ctrl Pts',(-39.1050621731301,38.1280696847148,41.7584541805251));
#33484=CARTESIAN_POINT('Ctrl Pts',(-39.1697655108715,38.2458340054359,41.8214741299099));
#33485=CARTESIAN_POINT('Ctrl Pts',(-39.2307791639605,38.3673742313302,41.8805369267837));
#33486=CARTESIAN_POINT('Ctrl Pts',(-39.2917928170496,38.4889144572246,41.9395997236574));
#33487=CARTESIAN_POINT('Ctrl Pts',(-39.3491166584187,38.6142303352866,41.9947052449932));
#33488=CARTESIAN_POINT('Ctrl Pts',(-39.4025242443065,38.7428269703345,42.0456357889521));
#33489=CARTESIAN_POINT('Ctrl Pts',(-39.4559318301942,38.8714236053824,42.0965663329109));
#33490=CARTESIAN_POINT('Ctrl Pts',(-39.5054230493503,39.003300729726,42.1433217933784));
#33491=CARTESIAN_POINT('Ctrl Pts',(-39.5508023754224,39.137937538607,42.1857174293239));
#33492=CARTESIAN_POINT('Ctrl Pts',(-39.5961817014946,39.272574347488,42.2281130652695));
#33493=CARTESIAN_POINT('Ctrl Pts',(-39.6374490399275,39.4099705606428,42.2661487883285));
#33494=CARTESIAN_POINT('Ctrl Pts',(-39.6744413261037,39.5495835754794,42.2996742776115));
#33495=CARTESIAN_POINT('Ctrl Pts',(-39.71143361228,39.689196590316,42.3331997668946));
#33496=CARTESIAN_POINT('Ctrl Pts',(-39.7441507690855,39.8310261162079,42.3622149524842));
#33497=CARTESIAN_POINT('Ctrl Pts',(-39.7724634818109,39.9745120365822,42.3866051213487));
#33498=CARTESIAN_POINT('Ctrl Pts',(-39.8007761945363,40.1179979569567,42.4109952902132));
#33499=CARTESIAN_POINT('Ctrl Pts',(-39.8246844041175,40.263139973116,42.4307603914344));
#33500=CARTESIAN_POINT('Ctrl Pts',(-39.8440935676073,40.4093648766837,42.4458222265642));
#33501=CARTESIAN_POINT('Ctrl Pts',(-39.8635027310971,40.5555897802513,42.4608840616941));
#33502=CARTESIAN_POINT('Ctrl Pts',(-39.8784128079477,40.7028972668148,42.4712425992159));
#33503=CARTESIAN_POINT('Ctrl Pts',(-39.888764774443,40.8507055618155,42.4768567738399));
#33504=CARTESIAN_POINT('Ctrl Pts',(-39.8991167409382,40.9985138568162,42.4824709484638));
#33505=CARTESIAN_POINT('Ctrl Pts',(-39.904910575367,41.1468226525277,42.4833407483241));
#33506=CARTESIAN_POINT('Ctrl Pts',(-39.9061232404223,41.2950462015824,42.4794625668233));
#33507=CARTESIAN_POINT('Ctrl Pts',(-39.9073359054777,41.443269750637,42.4755843853227));
#33508=CARTESIAN_POINT('Ctrl Pts',(-39.9039673984572,41.5914077444216,42.4669582303403));
#33509=CARTESIAN_POINT('Ctrl Pts',(-39.8960308516571,41.7388750876526,42.4536179838878));
#33510=CARTESIAN_POINT('Ctrl Pts',(-39.888094304857,41.8863424308836,42.4402777374353));
#33511=CARTESIAN_POINT('Ctrl Pts',(-39.8755897346058,42.0331388164954,42.4222234270757));
#33512=CARTESIAN_POINT('Ctrl Pts',(-39.8585663405558,42.1786844212221,42.3995261574783));
#33513=CARTESIAN_POINT('Ctrl Pts',(-39.8415429465059,42.3242300259488,42.3768288878809));
#33514=CARTESIAN_POINT('Ctrl Pts',(-39.8200007638886,42.4685245466947,42.349488706076));
#33515=CARTESIAN_POINT('Ctrl Pts',(-39.79402467282,42.6109980107428,42.3176133796576));
#33516=CARTESIAN_POINT('Ctrl Pts',(-39.7680485817515,42.7534714747909,42.2857380532391));
#33517=CARTESIAN_POINT('Ctrl Pts',(-39.7376386360887,42.8941235854065,42.2493276483347));
#33518=CARTESIAN_POINT('Ctrl Pts',(-39.7029147279111,43.0323987214329,42.2085257463487));
#33519=CARTESIAN_POINT('Ctrl Pts',(-39.6681908197334,43.1706738574592,42.1677238443626));
#33520=CARTESIAN_POINT('Ctrl Pts',(-39.6291530211,43.3065717308636,42.1225305299992));
#33521=CARTESIAN_POINT('Ctrl Pts',(-39.5859552912035,43.4395554600322,42.0731240666598));
#33522=CARTESIAN_POINT('Ctrl Pts',(-39.5427191696421,43.572657377513,42.0236736936891));
#33523=CARTESIAN_POINT('Ctrl Pts',(-39.4953158091684,43.7028396910567,41.9700027824006));
#33524=CARTESIAN_POINT('Ctrl Pts',(-39.4439325208564,43.8295871275298,41.9123234371075));
#33525=CARTESIAN_POINT('Ctrl Pts',(-38.5105944106268,37.3903900363275,41.3249697149968));
#33526=CARTESIAN_POINT('Ctrl Pts',(-38.5925880147889,37.4866716395425,41.4065204448413));
#33527=CARTESIAN_POINT('Ctrl Pts',(-38.6716518465919,37.588174582779,41.4848520562084));
#33528=CARTESIAN_POINT('Ctrl Pts',(-38.747464047146,37.6944856603538,41.559645670985));
#33529=CARTESIAN_POINT('Ctrl Pts',(-38.8232762477,37.8007967379286,41.6344392857616));
#33530=CARTESIAN_POINT('Ctrl Pts',(-38.8958366491455,37.911915714453,41.7056947383436));
#33531=CARTESIAN_POINT('Ctrl Pts',(-38.9648498672373,38.0273902385848,41.7731219567681));
#33532=CARTESIAN_POINT('Ctrl Pts',(-39.0338630853291,38.1428647627166,41.8405491751926));
#33533=CARTESIAN_POINT('Ctrl Pts',(-39.0993289672618,38.2626945787777,41.9041480101658));
#33534=CARTESIAN_POINT('Ctrl Pts',(-39.1609810096845,38.3863918746968,41.9636595588496));
#33535=CARTESIAN_POINT('Ctrl Pts',(-39.2226330521072,38.5100891706157,42.0231711075335));
#33536=CARTESIAN_POINT('Ctrl Pts',(-39.2804711185133,38.6376536725081,42.0785952381606));
#33537=CARTESIAN_POINT('Ctrl Pts',(-39.334259757427,38.7685660813717,42.1297063260836));
#33538=CARTESIAN_POINT('Ctrl Pts',(-39.3880483963409,38.8994784902351,42.1808174140066));
#33539=CARTESIAN_POINT('Ctrl Pts',(-39.4377874886664,39.0337385162099,42.2276153460581));
#33540=CARTESIAN_POINT('Ctrl Pts',(-39.4832745528305,39.1707996036594,42.2699096137572));
#33541=CARTESIAN_POINT('Ctrl Pts',(-39.5287616169945,39.307860691109,42.3122038814564));
#33542=CARTESIAN_POINT('Ctrl Pts',(-39.569996552282,39.4477225365593,42.3499943911576));
#33543=CARTESIAN_POINT('Ctrl Pts',(-39.6068114964706,39.5898157800732,42.3831273024607));
#33544=CARTESIAN_POINT('Ctrl Pts',(-39.6436264406592,39.731909023587,42.4162602137638));
#33545=CARTESIAN_POINT('Ctrl Pts',(-39.6760213122352,39.8762333505486,42.4447354533078));
#33546=CARTESIAN_POINT('Ctrl Pts',(-39.7038642357611,40.0222012348209,42.4684371019829));
#33547=CARTESIAN_POINT('Ctrl Pts',(-39.731707159287,40.1681691190932,42.4921387506579));
#33548=CARTESIAN_POINT('Ctrl Pts',(-39.7549980731144,40.3157802374815,42.511066755985));
#33549=CARTESIAN_POINT('Ctrl Pts',(-39.7736421628699,40.4644336837353,42.5251440644412));
#33550=CARTESIAN_POINT('Ctrl Pts',(-39.7922862526254,40.6130871299891,42.5392213728974));
#33551=CARTESIAN_POINT('Ctrl Pts',(-39.8062834770282,40.7627825749675,42.5484479533134));
#33552=CARTESIAN_POINT('Ctrl Pts',(-39.8155768551427,40.9129106273891,42.5527862454437));
#33553=CARTESIAN_POINT('Ctrl Pts',(-39.8248702332572,41.0630386798108,42.557124537574));
#33554=CARTESIAN_POINT('Ctrl Pts',(-39.8294597445064,41.2135990072699,42.556574531813));
#33555=CARTESIAN_POINT('Ctrl Pts',(-39.8293267055689,41.3639786976575,42.5511384671649));
#33556=CARTESIAN_POINT('Ctrl Pts',(-39.8291936666312,41.5143583880452,42.5457024025167));
#33557=CARTESIAN_POINT('Ctrl Pts',(-39.8243380778014,41.6645571083984,42.5353802910175));
#33558=CARTESIAN_POINT('Ctrl Pts',(-39.8147797055691,41.8139634186653,42.5202141526818));
#33559=CARTESIAN_POINT('Ctrl Pts',(-39.8052213333368,41.9633697289321,42.5050480143461));
#33560=CARTESIAN_POINT('Ctrl Pts',(-39.7909601988658,42.1119832983048,42.4850378827539));
#33561=CARTESIAN_POINT('Ctrl Pts',(-39.7720543574363,42.2591991396813,42.4602652166278));
#33562=CARTESIAN_POINT('Ctrl Pts',(-39.7531485160068,42.4064149810577,42.4354925505018));
#33563=CARTESIAN_POINT('Ctrl Pts',(-39.7295980094791,42.5522327684799,42.4059574046923));
#33564=CARTESIAN_POINT('Ctrl Pts',(-39.7014987089959,42.6960588961218,42.3717800130538));
#33565=CARTESIAN_POINT('Ctrl Pts',(-39.6733994085126,42.8398850237637,42.3376026214152));
#33566=CARTESIAN_POINT('Ctrl Pts',(-39.6407513762898,42.9817191731726,42.2987830596216));
#33567=CARTESIAN_POINT('Ctrl Pts',(-39.6036875183501,43.1209839554103,42.2554793572141));
#33568=CARTESIAN_POINT('Ctrl Pts',(-39.5666236604103,43.2602487376481,42.2121756548065));
#33569=CARTESIAN_POINT('Ctrl Pts',(-39.5251440588185,43.3969438443617,42.1643879076659));
#33570=CARTESIAN_POINT('Ctrl Pts',(-39.4794175718025,43.5305128070077,42.1123106536853));
#33571=CARTESIAN_POINT('Ctrl Pts',(-39.4336504457071,43.6642004780878,42.0601871164279));
#33572=CARTESIAN_POINT('Ctrl Pts',(-39.383628983482,43.7947561496885,42.0037665599188));
#33573=CARTESIAN_POINT('Ctrl Pts',(-39.3295571628989,43.921647389681,41.9432790580052));
#33574=CARTESIAN_POINT('Ctrl Pts',(-38.3401070380879,37.396188156926,41.4895374854793));
#33575=CARTESIAN_POINT('Ctrl Pts',(-38.4248693212561,37.4955353174855,41.5735409108681));
#33576=CARTESIAN_POINT('Ctrl Pts',(-38.506514813727,37.6004370897919,41.65411973065));
#33577=CARTESIAN_POINT('Ctrl Pts',(-38.5846906414969,37.7104401067918,41.7309256030157));
#33578=CARTESIAN_POINT('Ctrl Pts',(-38.6628664692668,37.8204431237917,41.8077314753812));
#33579=CARTESIAN_POINT('Ctrl Pts',(-38.7375724378322,37.9355471118982,41.880764209148));
#33580=CARTESIAN_POINT('Ctrl Pts',(-38.8084856098052,38.0552546781698,41.9497080168992));
#33581=CARTESIAN_POINT('Ctrl Pts',(-38.8793987817783,38.1749622444414,42.0186518246504));
#33582=CARTESIAN_POINT('Ctrl Pts',(-38.9465189806562,38.2992730912161,42.0835065346916));
#33583=CARTESIAN_POINT('Ctrl Pts',(-39.0095559897528,38.427650086403,42.1439916370817));
#33584=CARTESIAN_POINT('Ctrl Pts',(-39.0725929988496,38.5560270815899,42.2044767394719));
#33585=CARTESIAN_POINT('Ctrl Pts',(-39.1315466611802,38.6884699060094,42.260592083481));
#33586=CARTESIAN_POINT('Ctrl Pts',(-39.1861619833017,38.8244063172954,42.3120948561651));
#33587=CARTESIAN_POINT('Ctrl Pts',(-39.2407773054231,38.9603427285815,42.3635976288492));
#33588=CARTESIAN_POINT('Ctrl Pts',(-39.2910541512182,39.099772388779,42.4104877017388));
#33589=CARTESIAN_POINT('Ctrl Pts',(-39.3367749499686,39.2420928764857,42.4525620540421));
#33590=CARTESIAN_POINT('Ctrl Pts',(-39.3824957487191,39.3844133641924,42.4946364063455));
#33591=CARTESIAN_POINT('Ctrl Pts',(-39.423660386346,39.5296243255813,42.5318949329592));
#33592=CARTESIAN_POINT('Ctrl Pts',(-39.4600905923665,39.6770983514491,42.5641761580101));
#33593=CARTESIAN_POINT('Ctrl Pts',(-39.496520798387,39.824572377317,42.5964573830611));
#33594=CARTESIAN_POINT('Ctrl Pts',(-39.5282164817421,39.974309101005,42.6237612257167));
#33595=CARTESIAN_POINT('Ctrl Pts',(-39.555040211571,40.1256615321412,42.645969150317));
#33596=CARTESIAN_POINT('Ctrl Pts',(-39.5818639414,40.2770139632773,42.6681770749175));
#33597=CARTESIAN_POINT('Ctrl Pts',(-39.6038156504478,40.4299817255212,42.6852890255972));
#33598=CARTESIAN_POINT('Ctrl Pts',(-39.6207999354897,40.5839038229087,42.6972304327144));
#33599=CARTESIAN_POINT('Ctrl Pts',(-39.6377842205318,40.7378259202961,42.7091718398316));
#33600=CARTESIAN_POINT('Ctrl Pts',(-39.6498010386968,40.8927019700386,42.7159426729704));
#33601=CARTESIAN_POINT('Ctrl Pts',(-39.6567978408013,41.0478626671964,42.717512975975));
#33602=CARTESIAN_POINT('Ctrl Pts',(-39.6637946429058,41.2030233643541,42.7190832789797));
#33603=CARTESIAN_POINT('Ctrl Pts',(-39.6657714108332,41.3584683229798,42.715453047148));
#33604=CARTESIAN_POINT('Ctrl Pts',(-39.6627189071036,41.5135256978668,42.7066372013421));
#33605=CARTESIAN_POINT('Ctrl Pts',(-39.659666403374,41.6685830727536,42.6978213555362));
#33606=CARTESIAN_POINT('Ctrl Pts',(-39.6515846347838,41.8232524781121,42.683819916811));
#33607=CARTESIAN_POINT('Ctrl Pts',(-39.6385077605088,41.9768653196993,42.6646925603359));
#33608=CARTESIAN_POINT('Ctrl Pts',(-39.6254308862338,42.1304781612864,42.6455652038608));
#33609=CARTESIAN_POINT('Ctrl Pts',(-39.6073589379277,42.2830340567859,42.6213119762699));
#33610=CARTESIAN_POINT('Ctrl Pts',(-39.5843691828914,42.4338734269017,42.5920367990964));
#33611=CARTESIAN_POINT('Ctrl Pts',(-39.5613794278551,42.5847127970175,42.562761621923));
#33612=CARTESIAN_POINT('Ctrl Pts',(-39.5334719223308,42.7338352661928,42.5284645669829));
#33613=CARTESIAN_POINT('Ctrl Pts',(-39.5007663821658,42.8805959572736,42.489292913312));
#33614=CARTESIAN_POINT('Ctrl Pts',(-39.4680608420009,43.0273566483544,42.4501212596411));
#33615=CARTESIAN_POINT('Ctrl Pts',(-39.4305573475459,43.1717551957721,42.4060751036235));
#33616=CARTESIAN_POINT('Ctrl Pts',(-39.3884170381864,43.3131669860338,42.3573438196041));
#33617=CARTESIAN_POINT('Ctrl Pts',(-39.346276728827,43.4545787762955,42.3086125355848));
#33618=CARTESIAN_POINT('Ctrl Pts',(-39.2994997083353,43.593003456964,42.2551962436915));
#33619=CARTESIAN_POINT('Ctrl Pts',(-39.2482871579526,43.7278420662347,42.1973247888432));
#33620=CARTESIAN_POINT('Ctrl Pts',(-39.197029092792,43.8628005123285,42.1394019011646));
#33621=CARTESIAN_POINT('Ctrl Pts',(-39.1413277366783,43.9941661731301,42.0770160711227));
#33622=CARTESIAN_POINT('Ctrl Pts',(-39.0814232252891,44.1213693905809,42.0104363569345));
#33623=CARTESIAN_POINT('Ctrl Pts',(-38.1698933472347,37.4023057767316,41.654374420382));
#33624=CARTESIAN_POINT('Ctrl Pts',(-38.2574371396393,37.5046775074782,41.740752380849));
#33625=CARTESIAN_POINT('Ctrl Pts',(-38.3416705748698,37.6129487843841,41.8234930542166));
#33626=CARTESIAN_POINT('Ctrl Pts',(-38.422207032264,37.7266226511676,41.9022165301249));
#33627=CARTESIAN_POINT('Ctrl Pts',(-38.5027434896582,37.8402965179512,41.9809400060332));
#33628=CARTESIAN_POINT('Ctrl Pts',(-38.5795827433154,37.959372655871,42.0556460634807));
#33629=CARTESIAN_POINT('Ctrl Pts',(-38.6523720426952,38.0833045948027,42.1259915980532));
#33630=CARTESIAN_POINT('Ctrl Pts',(-38.725161342075,38.2072365337344,42.1963371326256));
#33631=CARTESIAN_POINT('Ctrl Pts',(-38.7939004829064,38.3360239262585,42.2623219467166));
#33632=CARTESIAN_POINT('Ctrl Pts',(-38.8582738129496,38.4690757875448,42.3236428832583));
#33633=CARTESIAN_POINT('Ctrl Pts',(-38.9226471429928,38.602127648831,42.3849638198));
#33634=CARTESIAN_POINT('Ctrl Pts',(-38.9826544814682,38.7394436059457,42.441620706383));
#33635=CARTESIAN_POINT('Ctrl Pts',(-39.0380201640102,38.8803935651702,42.4933531100336));
#33636=CARTESIAN_POINT('Ctrl Pts',(-39.0933858465522,39.0213435243946,42.5450855136842));
#33637=CARTESIAN_POINT('Ctrl Pts',(-39.1441097175204,39.165927090677,42.5918932887627));
#33638=CARTESIAN_POINT('Ctrl Pts',(-39.1899586250542,39.3134808246791,42.6335611131595));
#33639=CARTESIAN_POINT('Ctrl Pts',(-39.235807532588,39.4610345586814,42.6752289375563));
#33640=CARTESIAN_POINT('Ctrl Pts',(-39.2767813476062,39.6115580468308,42.7117566937311));
#33641=CARTESIAN_POINT('Ctrl Pts',(-39.3126915674182,39.7643605724095,42.7429761454479));
#33642=CARTESIAN_POINT('Ctrl Pts',(-39.3486017872303,39.9171630979881,42.7741955971648));
#33643=CARTESIAN_POINT('Ctrl Pts',(-39.3794483104926,40.0722442326687,42.8001066560573));
#33644=CARTESIAN_POINT('Ctrl Pts',(-39.4050890128859,40.2288923003061,42.8205897169714));
#33645=CARTESIAN_POINT('Ctrl Pts',(-39.4307297152792,40.3855403679434,42.8410727778855));
#33646=CARTESIAN_POINT('Ctrl Pts',(-39.4511645241242,40.543754929356,42.8561277824382));
#33647=CARTESIAN_POINT('Ctrl Pts',(-39.4662989994119,40.7028098591025,42.8656848578283));
#33648=CARTESIAN_POINT('Ctrl Pts',(-39.4814334746995,40.8618647888489,42.8752419332184));
#33649=CARTESIAN_POINT('Ctrl Pts',(-39.491267573081,41.0217596408937,42.8793010515829));
#33650=CARTESIAN_POINT('Ctrl Pts',(-39.4957554095817,41.1817604835205,42.8778427197039));
#33651=CARTESIAN_POINT('Ctrl Pts',(-39.5002432460823,41.3417613261473,42.8763843878249));
#33652=CARTESIAN_POINT('Ctrl Pts',(-39.4993848070836,41.5018677105294,42.869408608619));
#33653=CARTESIAN_POINT('Ctrl Pts',(-39.493183190154,41.6613446140811,42.8569464556646));
#33654=CARTESIAN_POINT('Ctrl Pts',(-39.4869815732246,41.8208215176326,42.8444843027102));
#33655=CARTESIAN_POINT('Ctrl Pts',(-39.4754367946057,41.9796684928248,42.8265358096833));
#33656=CARTESIAN_POINT('Ctrl Pts',(-39.4586009147309,42.1371561528159,42.803182342358));
#33657=CARTESIAN_POINT('Ctrl Pts',(-39.4417650348561,42.2946438128069,42.7798288750327));
#33658=CARTESIAN_POINT('Ctrl Pts',(-39.419638099685,42.4507717154438,42.7510704975448));
#33659=CARTESIAN_POINT('Ctrl Pts',(-39.3923206657399,42.6048227861614,42.7170381338524));
#33660=CARTESIAN_POINT('Ctrl Pts',(-39.3650032317948,42.7588738568789,42.68300577016));
#33661=CARTESIAN_POINT('Ctrl Pts',(-39.3324953743416,42.9108476629302,42.6436995142815));
#33662=CARTESIAN_POINT('Ctrl Pts',(-39.2949452362731,43.0600460076279,42.599298661516));
#33663=CARTESIAN_POINT('Ctrl Pts',(-39.2573950982045,43.2092443523257,42.5548978087504));
#33664=CARTESIAN_POINT('Ctrl Pts',(-39.2148027834144,43.3556668162752,42.50540248215));
#33665=CARTESIAN_POINT('Ctrl Pts',(-39.1673626766853,43.4986404754819,42.4510387193772));
#33666=CARTESIAN_POINT('Ctrl Pts',(-39.1199225699561,43.6416141346887,42.3966749566045));
#33667=CARTESIAN_POINT('Ctrl Pts',(-39.0676348028709,43.7811385869357,42.3374429086328));
#33668=CARTESIAN_POINT('Ctrl Pts',(-39.010738234995,43.9165723466299,42.2736132990986));
#33669=CARTESIAN_POINT('Ctrl Pts',(-38.9537911007125,44.052126472083,42.2097269614679));
#33670=CARTESIAN_POINT('Ctrl Pts',(-38.892227128286,44.1835822485594,42.1412350643881));
#33671=CARTESIAN_POINT('Ctrl Pts',(-38.8263282286146,44.3103338969357,42.0684513874025));
#33672=CARTESIAN_POINT('Ctrl Pts',(-38.0000876683942,37.4088997145424,41.8196126328366));
#33673=CARTESIAN_POINT('Ctrl Pts',(-38.0904681512693,37.5142776343105,41.9082850918914));
#33674=CARTESIAN_POINT('Ctrl Pts',(-38.1773371111399,37.6259135682359,41.9930992333451));
#33675=CARTESIAN_POINT('Ctrl Pts',(-38.2602708604475,37.7432630321777,42.0736413913554));
#33676=CARTESIAN_POINT('Ctrl Pts',(-38.3432046097552,37.8606124961195,42.1541835493656));
#33677=CARTESIAN_POINT('Ctrl Pts',(-38.4222028848055,37.9836751169552,42.2304534678416));
#33678=CARTESIAN_POINT('Ctrl Pts',(-38.4968803858612,38.111850678957,42.3020791538276));
#33679=CARTESIAN_POINT('Ctrl Pts',(-38.5715578869169,38.2400262409588,42.3737048398136));
#33680=CARTESIAN_POINT('Ctrl Pts',(-38.6419143765348,38.3733143365819,42.4406860655693));
#33681=CARTESIAN_POINT('Ctrl Pts',(-38.7076067036954,38.5110648771956,42.5026961420409));
#33682=CARTESIAN_POINT('Ctrl Pts',(-38.7732990308561,38.6488154178094,42.5647062185125));
#33683=CARTESIAN_POINT('Ctrl Pts',(-38.8343269866852,38.7910279654247,42.6217449485334));
#33684=CARTESIAN_POINT('Ctrl Pts',(-38.8903929183668,38.937008903999,42.6735341357586));
#33685=CARTESIAN_POINT('Ctrl Pts',(-38.9464588500485,39.0829898425733,42.7253233229839));
#33686=CARTESIAN_POINT('Ctrl Pts',(-38.9975625793161,39.2327387079484,42.7718628027449));
#33687=CARTESIAN_POINT('Ctrl Pts',(-39.0434548569381,39.3855251270308,42.8129255868781));
#33688=CARTESIAN_POINT('Ctrl Pts',(-39.0893471345601,39.5383115461131,42.8539883710113));
#33689=CARTESIAN_POINT('Ctrl Pts',(-39.1300278146177,39.6941350331057,42.8895743289534));
#33690=CARTESIAN_POINT('Ctrl Pts',(-39.1652984843805,39.852235587009,42.9195098963547));
#33691=CARTESIAN_POINT('Ctrl Pts',(-39.2005691541434,40.0103361409123,42.9494454637562));
#33692=CARTESIAN_POINT('Ctrl Pts',(-39.2304297014648,40.1707132590325,42.9737305454333));
#33693=CARTESIAN_POINT('Ctrl Pts',(-39.2547344868207,40.3325847308073,42.9922466950162));
#33694=CARTESIAN_POINT('Ctrl Pts',(-39.2790392721765,40.494456202582,43.0107628445991));
#33695=CARTESIAN_POINT('Ctrl Pts',(-39.2977882182871,40.6578215133272,43.0235100032131));
#33696=CARTESIAN_POINT('Ctrl Pts',(-39.310889880424,40.821883878049,43.0304259986301));
#33697=CARTESIAN_POINT('Ctrl Pts',(-39.3239915425609,40.9859462427706,43.0373419940472));
#33698=CARTESIAN_POINT('Ctrl Pts',(-39.3314458790656,41.1507051398183,43.0384268042762));
#33699=CARTESIAN_POINT('Ctrl Pts',(-39.333216532603,41.31535698716,43.0336751381041));
#33700=CARTESIAN_POINT('Ctrl Pts',(-39.3349871861405,41.4800088345017,43.0289234719321));
#33701=CARTESIAN_POINT('Ctrl Pts',(-39.3310741510799,41.6445531086124,43.0183353444663));
#33702=CARTESIAN_POINT('Ctrl Pts',(-39.3214965123727,41.8081872741634,43.0019623971693));
#33703=CARTESIAN_POINT('Ctrl Pts',(-39.3119188736654,41.9718214397145,42.9855894498722));
#33704=CARTESIAN_POINT('Ctrl Pts',(-39.2966766617635,42.1345449764166,42.963431734802));
#33705=CARTESIAN_POINT('Ctrl Pts',(-39.2758442176283,42.2955642291726,42.9355973220397));
#33706=CARTESIAN_POINT('Ctrl Pts',(-39.2550117734931,42.4565834819286,42.9077629092774));
#33707=CARTESIAN_POINT('Ctrl Pts',(-39.2285891633622,42.6158979387632,42.8742518873238));
#33708=CARTESIAN_POINT('Ctrl Pts',(-39.19670525858,42.7727305716617,42.8352277000236));
#33709=CARTESIAN_POINT('Ctrl Pts',(-39.1648213537978,42.9295632045603,42.7962035127234));
#33710=CARTESIAN_POINT('Ctrl Pts',(-39.1274762557409,43.083913514859,42.7516662841563));
#33711=CARTESIAN_POINT('Ctrl Pts',(-39.084852108241,43.2350286861848,42.7018332365743));
#33712=CARTESIAN_POINT('Ctrl Pts',(-39.042227960741,43.3861438575105,42.6520001889924));
#33713=CARTESIAN_POINT('Ctrl Pts',(-38.9943248993241,43.5340234093782,42.596871480843));
#33714=CARTESIAN_POINT('Ctrl Pts',(-38.9413765624222,43.6779460852896,42.5367159924989));
#33715=CARTESIAN_POINT('Ctrl Pts',(-38.8884282255205,43.821868761201,42.4765605041547));
#33716=CARTESIAN_POINT('Ctrl Pts',(-38.8304347814866,43.9618341035397,42.4113784268845));
#33717=CARTESIAN_POINT('Ctrl Pts',(-38.7676790828296,44.097159455865,42.3414876746605));
#33718=CARTESIAN_POINT('Ctrl Pts',(-38.7048676105065,44.2326050776027,42.2715348075442));
#33719=CARTESIAN_POINT('Ctrl Pts',(-38.6372856148521,44.3634020271021,42.1968651147725));
#33720=CARTESIAN_POINT('Ctrl Pts',(-38.5652632803349,44.4889112104465,42.1178434117343));
#33721=CARTESIAN_POINT('Ctrl Pts',(-38.0398886763558,37.4073630839945,41.7808966890927));
#33722=CARTESIAN_POINT('Ctrl Pts',(-38.196487830305,37.401351958814,41.6286232707617));
#33723=CARTESIAN_POINT('Ctrl Pts',(-38.353424823516,37.395735231147,41.4766821154713));
#33724=CARTESIAN_POINT('Ctrl Pts',(-38.5105944106295,37.3903900363274,41.3249697149942));
#33725=CARTESIAN_POINT('Ctrl Pts',(-38.5891792041849,37.3877174389176,41.249113514757));
#33726=CARTESIAN_POINT('Ctrl Pts',(-38.6678226442078,37.3851133060814,41.1733149929954));
#33727=CARTESIAN_POINT('Ctrl Pts',(-38.7465138697966,37.3825649586746,41.0975634680728));
#33728=CARTESIAN_POINT('Ctrl Pts',(-38.825205095388,37.3800166112678,41.0218119431476));
#33729=CARTESIAN_POINT('Ctrl Pts',(-38.9039441351633,37.3775240826995,40.946107443207));
#33730=CARTESIAN_POINT('Ctrl Pts',(-38.9827210478919,37.3750757674608,40.8704401911061));
#33731=CARTESIAN_POINT('Ctrl Pts',(-39.0614979606169,37.3726274522222,40.7947729390086));
#33732=CARTESIAN_POINT('Ctrl Pts',(-39.1403127743051,37.3702233830122,40.7191429622981));
#33733=CARTESIAN_POINT('Ctrl Pts',(-39.2191560456546,37.3678525356093,40.6435409735397));
#33734=CARTESIAN_POINT('Ctrl Pts',(-39.2979993170057,37.3654816882064,40.5679389847796));
#33735=CARTESIAN_POINT('Ctrl Pts',(-39.3768710769017,37.3631440986645,40.4923650143452));
#33736=CARTESIAN_POINT('Ctrl Pts',(-39.4557619421374,37.3608288129201,40.4168098339066));
#33737=CARTESIAN_POINT('Ctrl Pts',(-39.5346528073732,37.3585135271757,40.341254653468));
#33738=CARTESIAN_POINT('Ctrl Pts',(-39.6135628167506,37.3562205905267,40.2657183011866));
#33739=CARTESIAN_POINT('Ctrl Pts',(-39.6924821306133,37.3539385160429,40.1901910998149));
#33740=CARTESIAN_POINT('Ctrl Pts',(-39.7714014444796,37.3516564415591,40.1146638984399));
#33741=CARTESIAN_POINT('Ctrl Pts',(-39.8503301182025,37.3493852938815,40.0391459024319));
#33742=CARTESIAN_POINT('Ctrl Pts',(-39.9292571604855,37.3471122416419,39.9636263019119));
#33743=CARTESIAN_POINT('Ctrl Pts',(-40.0081842027615,37.3448391894025,39.8881067013986));
#33744=CARTESIAN_POINT('Ctrl Pts',(-40.087109702463,37.3425643363435,39.8125855837718));
#33745=CARTESIAN_POINT('Ctrl Pts',(-40.166020457705,37.3402722704297,39.7370499650508));
#33746=CARTESIAN_POINT('Ctrl Pts',(-40.2449312129548,37.3379802045157,39.6615143463223));
#33747=CARTESIAN_POINT('Ctrl Pts',(-40.3238273833577,37.3356711120805,39.5859643834778));
#33748=CARTESIAN_POINT('Ctrl Pts',(-40.4026917455433,37.3333248863596,39.5103831374279));
#33749=CARTESIAN_POINT('Ctrl Pts',(-40.4421239266295,37.3321517734993,39.4725925144092));
#33750=CARTESIAN_POINT('Ctrl Pts',(-40.4815480803642,37.3309692894147,39.4347939965346));
#33751=CARTESIAN_POINT('Ctrl Pts',(-40.520961424251,37.329774185787,39.3969848472346));
#33752=CARTESIAN_POINT('Ctrl Pts',(-40.5603747681469,37.328579082159,39.3591756979259));
#33753=CARTESIAN_POINT('Ctrl Pts',(-40.5997773169133,37.3273713761704,39.3213559316673));
#33754=CARTESIAN_POINT('Ctrl Pts',(-40.6391656485399,37.3261470729261,39.2835221829305));
#33755=CARTESIAN_POINT('Ctrl Pts',(-40.678553980157,37.3249227696822,39.2456884342028));
#33756=CARTESIAN_POINT('Ctrl Pts',(-40.7179281175588,37.3236818959449,39.2078407255431));
#33757=CARTESIAN_POINT('Ctrl Pts',(-40.7572837211927,37.3224193856699,39.1699747890254));
#33758=CARTESIAN_POINT('Ctrl Pts',(-40.7966393248366,37.3211568753946,39.1321088524983));
#33759=CARTESIAN_POINT('Ctrl Pts',(-40.8359764322357,37.3198727723864,39.0942247250169));
#33760=CARTESIAN_POINT('Ctrl Pts',(-40.8752893413857,37.3185604200586,39.0563167986917));
#33761=CARTESIAN_POINT('Ctrl Pts',(-40.9146022505253,37.3172480677311,39.0184088723765));
#33762=CARTESIAN_POINT('Ctrl Pts',(-40.9538910266967,37.3159075422936,38.9804772114209));
#33763=CARTESIAN_POINT('Ctrl Pts',(-40.9931478523898,37.3145297174934,38.942514127347));
#33764=CARTESIAN_POINT('Ctrl Pts',(-41.0324046780937,37.3131518926928,38.9045510432627));
#33765=CARTESIAN_POINT('Ctrl Pts',(-41.0716296760241,37.3117369117765,38.8665566567397));
#33766=CARTESIAN_POINT('Ctrl Pts',(-41.110811545496,37.3102715821923,38.8285198536169));
#33767=CARTESIAN_POINT('Ctrl Pts',(-41.1304024802235,37.3095389174004,38.8095014520637));
#33768=CARTESIAN_POINT('Ctrl Pts',(-41.1499825689311,37.3087935908378,38.7904723835099));
#33769=CARTESIAN_POINT('Ctrl Pts',(-41.1695498758672,37.3080333426855,38.7714307441549));
#33770=CARTESIAN_POINT('Ctrl Pts',(-41.1891171828148,37.3072730945327,38.7523891047887));
#33771=CARTESIAN_POINT('Ctrl Pts',(-41.208671719699,37.3064979384582,38.733334906136));
#33772=CARTESIAN_POINT('Ctrl Pts',(-41.2282110281082,37.3057050044836,38.7142657303626));
#33773=CARTESIAN_POINT('Ctrl Pts',(-41.2477503365059,37.3049120705096,38.6951965546006));
#33774=CARTESIAN_POINT('Ctrl Pts',(-41.2672744347923,37.3041013800735,38.6761124197787));
#33775=CARTESIAN_POINT('Ctrl Pts',(-41.2867801198516,37.3032691938202,38.6570101756499));
#33776=CARTESIAN_POINT('Ctrl Pts',(-41.3062858049228,37.3024370075665,38.6379079315096));
#33777=CARTESIAN_POINT('Ctrl Pts',(-41.3257731069796,37.3015833607664,38.6187876077765));
#33778=CARTESIAN_POINT('Ctrl Pts',(-41.3452377207335,37.3007032273755,38.5996449702233));
#33779=CARTESIAN_POINT('Ctrl Pts',(-41.3647023344753,37.2998230939851,38.580502332682));
#33780=CARTESIAN_POINT('Ctrl Pts',(-41.3841443126135,37.298916535526,38.5613374331501));
#33781=CARTESIAN_POINT('Ctrl Pts',(-41.4035576403255,37.2979765302234,38.5421443560828));
#33782=CARTESIAN_POINT('Ctrl Pts',(-41.4229709680498,37.2970365249202,38.5229512790035));
#33783=CARTESIAN_POINT('Ctrl Pts',(-41.4423557441877,37.2960631881607,38.5037301215973));
#33784=CARTESIAN_POINT('Ctrl Pts',(-41.4617031412364,37.2950462146141,38.484472202064));
#33785=CARTESIAN_POINT('Ctrl Pts',(-41.4810505382725,37.2940292410683,38.4652142825432));
#33786=CARTESIAN_POINT('Ctrl Pts',(-41.5003607592692,37.2929688677782,38.4459198005936));
#33787=CARTESIAN_POINT('Ctrl Pts',(-41.5196199854035,37.2918489624883,38.4265751654797));
#33788=CARTESIAN_POINT('Ctrl Pts',(-41.5292495984738,37.2912890098432,38.4169028479197));
#33789=CARTESIAN_POINT('Ctrl Pts',(-41.5388663699674,37.2907140657909,38.4072179007401));
#33790=CARTESIAN_POINT('Ctrl Pts',(-41.5484677647746,37.2901211708148,38.3975178306749));
#33791=CARTESIAN_POINT('Ctrl Pts',(-41.5580691595883,37.2895282758384,38.3878177606031));
#33792=CARTESIAN_POINT('Ctrl Pts',(-41.5676552001071,37.2889174560781,38.3781025896675));
#33793=CARTESIAN_POINT('Ctrl Pts',(-41.5772224902082,37.2882847468604,38.3683689778));
#33794=CARTESIAN_POINT('Ctrl Pts',(-41.5867897802965,37.2876520376437,38.3586353659456));
#33795=CARTESIAN_POINT('Ctrl Pts',(-41.5963383565882,37.2869974817215,38.3488833491761));
#33796=CARTESIAN_POINT('Ctrl Pts',(-41.6058635266892,37.286315601138,38.3391083125477));
#33797=CARTESIAN_POINT('Ctrl Pts',(-41.6153886968031,37.2856337205536,38.3293332759061));
#33798=CARTESIAN_POINT('Ctrl Pts',(-41.6248905220874,37.2849245869414,38.3195352797541));
#33799=CARTESIAN_POINT('Ctrl Pts',(-41.6343622916865,37.2841803659703,38.3097077240023));
#33800=CARTESIAN_POINT('Ctrl Pts',(-41.6438340612728,37.2834361450001,38.299880168264));
#33801=CARTESIAN_POINT('Ctrl Pts',(-41.6532758769268,37.2826569554584,38.2900231529994));
#33802=CARTESIAN_POINT('Ctrl Pts',(-41.6626778025202,37.2818311977926,38.2801269060814));
#33803=CARTESIAN_POINT('Ctrl Pts',(-41.6720797281266,37.2810054401256,38.2702306591499));
#33804=CARTESIAN_POINT('Ctrl Pts',(-41.6814419126922,37.280133288302,38.2602953271252));
#33805=CARTESIAN_POINT('Ctrl Pts',(-41.6907493023114,37.2791971682157,38.2503061045745));
#33806=CARTESIAN_POINT('Ctrl Pts',(-41.6954029971114,37.2787291081736,38.2453114933095));
#33807=CARTESIAN_POINT('Ctrl Pts',(-41.7000428977186,37.2782449446291,38.2403033155323));
#33808=CARTESIAN_POINT('Ctrl Pts',(-41.7046664632498,37.2777417113255,38.2352790722985));
#33809=CARTESIAN_POINT('Ctrl Pts',(-41.7092900287873,37.2772384780212,38.2302548290579));
#33810=CARTESIAN_POINT('Ctrl Pts',(-41.7138972585809,37.276716174178,38.2252145197037));
#33811=CARTESIAN_POINT('Ctrl Pts',(-41.7184851250849,37.2761712654037,38.2201551666616));
#33812=CARTESIAN_POINT('Ctrl Pts',(-41.7230729915889,37.2756263566294,38.2150958136196));
#33813=CARTESIAN_POINT('Ctrl Pts',(-41.7276414848393,37.2750588312918,38.21001740709));
#33814=CARTESIAN_POINT('Ctrl Pts',(-41.7321871653729,37.2744646741212,38.20491656438));
#33815=CARTESIAN_POINT('Ctrl Pts',(-41.7367328459131,37.2738705169498,38.1998157216626));
#33816=CARTESIAN_POINT('Ctrl Pts',(-41.7412556909106,37.2732497012984,38.1946924203157));
#33817=CARTESIAN_POINT('Ctrl Pts',(-41.7457520939533,37.2725980169989,38.1895431134528));
#33818=CARTESIAN_POINT('Ctrl Pts',(-41.7502484969831,37.2719463327013,38.1843938066046));
#33819=CARTESIAN_POINT('Ctrl Pts',(-41.7547184267385,37.271263743193,38.1792184634379));
#33820=CARTESIAN_POINT('Ctrl Pts',(-41.7591585257862,37.2705463289669,38.1740137819355));
#33821=CARTESIAN_POINT('Ctrl Pts',(-41.7635986248468,37.2698289147387,38.1688091004181));
#33822=CARTESIAN_POINT('Ctrl Pts',(-41.7680088677799,37.2690766461175,38.163575055565));
#33823=CARTESIAN_POINT('Ctrl Pts',(-41.7723865878687,37.2682864099468,38.1583090246749));
#33824=CARTESIAN_POINT('Ctrl Pts',(-41.7767643079513,37.2674961737772,38.1530429937924));
#33825=CARTESIAN_POINT('Ctrl Pts',(-41.7811094995483,37.2666679632042,38.1477449708898));
#33826=CARTESIAN_POINT('Ctrl Pts',(-41.7854204349472,37.2657997620299,38.1424132579943));
#33827=CARTESIAN_POINT('Ctrl Pts',(-41.7864981687969,37.2655827117364,38.1410803297704));
#33828=CARTESIAN_POINT('Ctrl Pts',(-41.7875737620729,37.2653631624537,38.1397452962095));
#33829=CARTESIAN_POINT('Ctrl Pts',(-41.7886472050151,37.2651411028499,38.1384081478136));
#33830=CARTESIAN_POINT('Ctrl Pts',(-41.7889155657455,37.2650855879501,38.1380738607211));
#33831=CARTESIAN_POINT('Ctrl Pts',(-41.7891882242383,37.2650307276919,38.1377366532483));
#33832=CARTESIAN_POINT('Ctrl Pts',(-41.789451172242,37.2649739597976,38.137405330718));
#33833=CARTESIAN_POINT('Ctrl Pts',(-41.7897141202531,37.2649171919017,38.1370740081785));
#33834=CARTESIAN_POINT('Ctrl Pts',(-41.7899770299188,37.2648604923531,38.1367426435067));
#33835=CARTESIAN_POINT('Ctrl Pts',(-41.7902399729327,37.2648037333654,38.1364113154772));
#33836=CARTESIAN_POINT('Ctrl Pts',(-41.7907658589594,37.2646902153904,38.1357486594197));
#33837=CARTESIAN_POINT('Ctrl Pts',(-41.7912917036929,37.2645767709905,38.1350859579939));
#33838=CARTESIAN_POINT('Ctrl Pts',(-41.7918175742758,37.2644632804643,38.1344232849708));
#33839=CARTESIAN_POINT('Ctrl Pts',(-41.7939210565952,37.2640093183625,38.1317725928941));
#33840=CARTESIAN_POINT('Ctrl Pts',(-41.7960245110482,37.2635554059264,38.1291218701979));
#33841=CARTESIAN_POINT('Ctrl Pts',(-41.7981279794346,37.2631014686576,38.1264711628116));
#33842=CARTESIAN_POINT('Origin',(-36.3078527277528,58.7571818148754,39.9768461872608));
#33843=CARTESIAN_POINT('',(-33.5529552244032,70.2939023154161,29.521482977958));
#33844=CARTESIAN_POINT('',(-26.1333050833765,70.2640602812185,36.2258025733947));
#33845=CARTESIAN_POINT('Origin',(-29.8431301538898,70.2789812983173,32.8736427756763));
#33846=CARTESIAN_POINT('',(-40.0176777982662,58.7721028319742,36.6246863895425));
#33847=CARTESIAN_POINT('',(-40.0176777982662,58.7721028319742,36.6246863895425));
#33848=CARTESIAN_POINT('',(-32.5980276572394,58.7422607977766,43.3290059849791));
#33849=CARTESIAN_POINT('Origin',(-36.3078527277528,58.7571818148754,39.9768461872608));
#33850=CARTESIAN_POINT('',(-32.5980276572394,58.7422607977766,43.3290059849791));
#33851=CARTESIAN_POINT('Origin',(-32.5980276572394,58.7422607977766,43.3290059849791));
#33852=CARTESIAN_POINT('',(-24.4181484426939,68.1256242727979,34.3181253946216));
#33853=CARTESIAN_POINT('',(-26.1333050833765,70.2640602812185,36.2258025733947));
#33854=CARTESIAN_POINT('',(-30.8828710165569,56.603824789356,41.4213288062061));
#33855=CARTESIAN_POINT('',(-32.5980276572394,58.7422607977766,43.3290059849791));
#33856=CARTESIAN_POINT('',(-30.8828710165569,56.603824789356,41.4213288062061));
#33857=CARTESIAN_POINT('Origin',(-30.14514456676,51.0735937808341,33.1223948565145));
#33858=CARTESIAN_POINT('',(-23.7241967287056,67.8609953274847,34.5204571570535));
#33859=CARTESIAN_POINT('Origin',(-23.680421992897,62.595393264276,26.01919144493));
#33860=CARTESIAN_POINT('',(-30.1889193025686,56.3391958440429,41.623660568638));
#33861=CARTESIAN_POINT('Origin',(-30.14514456676,51.0735937808341,33.1223948565145));
#33862=CARTESIAN_POINT('',(-30.1889193025686,56.3391958440429,41.623660568638));
#33863=CARTESIAN_POINT('Origin',(-5.81522832743221,46.4801655823699,45.702859600428));
#33864=CARTESIAN_POINT('Origin',(-17.0047025368452,45.7553165663936,36.4551430811504));
#33865=CARTESIAN_POINT('',(-19.0137036843474,67.8420495966423,38.7768102493421));
#33866=CARTESIAN_POINT('',(-10.5399799629823,57.2771160498355,29.3519396695659));
#33867=CARTESIAN_POINT('',(-10.5399799629823,57.2771160498355,29.3519396695659));
#33868=CARTESIAN_POINT('',(-25.4784262582104,56.3202501132004,45.8800136609266));
#33869=CARTESIAN_POINT('',(-25.4784262582104,56.3202501132004,45.8800136609266));
#33870=CARTESIAN_POINT('',(-17.0047025368452,45.7553165663936,36.4551430811504));
#33871=CARTESIAN_POINT('',(-17.0047025368452,45.7553165663936,36.4551430811504));
#33872=CARTESIAN_POINT('',(-17.0047025368452,45.7553165663936,36.4551430811504));
#33873=CARTESIAN_POINT('Origin',(-25.4784262582104,56.3202501132004,45.8800136609266));
#33874=CARTESIAN_POINT('',(-19.0137036843474,67.8420495966423,38.7768102493421));
#33875=CARTESIAN_POINT('',(-25.4784262582104,56.3202501132004,45.8800136609266));
#33876=CARTESIAN_POINT('Origin',(-17.0047025368452,45.7553165663936,36.4551430811504));
#33877=CARTESIAN_POINT('',(-10.5399799629823,57.2771160498355,29.3519396695659));
#33878=CARTESIAN_POINT('',(-17.0047025368452,45.7553165663936,36.4551430811504));
#33879=CARTESIAN_POINT('Origin',(-37.9028116553955,37.2474344007039,41.6462389504159));
#33880=CARTESIAN_POINT('Origin',(-40.0176777982662,58.7721028319742,36.6246863895425));
#33881=CARTESIAN_POINT('',(-33.5529552244032,70.2939023154161,29.521482977958));
#33882=CARTESIAN_POINT('',(-40.0176777982662,58.7721028319742,36.6246863895425));
#33883=CARTESIAN_POINT('Origin',(-29.8431301538898,70.2789812983173,32.8736427756763));
#33884=CARTESIAN_POINT('Origin',(-44.6514843000067,41.123844669555,31.2333209653637));
#33885=CARTESIAN_POINT('Origin',(-18.0776624288824,72.5809528165923,19.8630818215568));
#33886=CARTESIAN_POINT('Origin',(-36.3078527277528,58.7571818148754,39.9768461872608));
#33887=CARTESIAN_POINT('Origin',(-53.2977525215594,44.2689648703008,19.9340598087839));
#33888=CARTESIAN_POINT('Origin',(-7.08622728734316,53.9840227357375,43.4139320205864));
#33889=CARTESIAN_POINT('',(-13.7639124142673,54.0108805665153,37.3800443846934));
#33890=CARTESIAN_POINT('',(-14.8937422437826,55.4195383727563,38.6366937953302));
#33891=CARTESIAN_POINT('',(-13.7639124142673,54.0108805665153,37.3800443846934));
#33892=CARTESIAN_POINT('',(-8.21605711685851,55.3926805419784,44.6705814312232));
#33893=CARTESIAN_POINT('',(-8.21605711685851,55.3926805419784,44.6705814312232));
#33894=CARTESIAN_POINT('',(-7.08622728734316,53.9840227357375,43.4139320205864));
#33895=CARTESIAN_POINT('',(-7.08622728734316,53.9840227357375,43.4139320205864));
#33896=CARTESIAN_POINT('',(-7.08622728734316,53.9840227357375,43.4139320205864));
#33897=CARTESIAN_POINT('Origin',(-7.34481619029768,53.5231507563998,43.6980601570498));
#33898=CARTESIAN_POINT('',(-14.0225013172218,53.5500085871777,37.6641725211568));
#33899=CARTESIAN_POINT('',(-14.0225013172218,53.5500085871777,37.6641725211568));
#33900=CARTESIAN_POINT('',(-7.34481619029768,53.5231507563998,43.6980601570498));
#33901=CARTESIAN_POINT('',(-7.34481619029768,53.5231507563998,43.6980601570498));
#33902=CARTESIAN_POINT('',(-7.34481619029768,53.5231507563998,43.6980601570498));
#33903=CARTESIAN_POINT('Origin',(-12.5509467813568,62.5506302129796,36.075670838085));
#33904=CARTESIAN_POINT('',(-15.1523311467371,54.9586663934186,38.9208219317936));
#33905=CARTESIAN_POINT('',(-15.1523311467371,54.9586663934186,38.9208219317936));
#33906=CARTESIAN_POINT('',(-14.8937422437826,55.4195383727563,38.6366937953302));
#33907=CARTESIAN_POINT('Origin',(-16.2626702143646,66.7932946931195,17.8286736257813));
#33908=CARTESIAN_POINT('Origin',(-8.21605711685851,55.3926805419784,44.6705814312232));
#33909=CARTESIAN_POINT('',(-8.47464601981303,54.9318085626407,44.9547095676866));
#33910=CARTESIAN_POINT('',(-8.47464601981303,54.9318085626407,44.9547095676866));
#33911=CARTESIAN_POINT('',(-8.21605711685851,55.3926805419784,44.6705814312232));
#33912=CARTESIAN_POINT('Origin',(-5.87326165443273,62.5237723822018,42.109558473978));
#33913=CARTESIAN_POINT('',(-8.47464601981303,54.9318085626407,44.9547095676866));
#33914=CARTESIAN_POINT('Origin',(-8.47464601981303,54.9318085626407,44.9547095676866));
#33915=CARTESIAN_POINT('Origin',(-9.55849548170321,62.9036549880343,48.8745226900051));
#33916=CARTESIAN_POINT('',(0.,0.,0.));
#33917=CARTESIAN_POINT('Origin',(-28.393108630048,72.7321117214098,30.9925849618393));
#33918=CARTESIAN_POINT('',(-38.9069263049545,56.3529534297169,37.0903559934943));
#33919=CARTESIAN_POINT('Origin',(-37.012738728532,57.369712410154,40.463522843952));
#33920=CARTESIAN_POINT('',(-39.7810443854308,54.7950500343233,38.0508053338062));
#33921=CARTESIAN_POINT('',(-30.2872962064705,71.7153527409726,27.6194181113816));
#33922=CARTESIAN_POINT('Origin',(-37.8868568090083,55.8118090147604,41.423972184264));
#33923=CARTESIAN_POINT('Origin',(-34.9009293544028,61.1335002414122,38.1431430628339));
#33924=CARTESIAN_POINT('',(-40.232869135087,56.4700997583121,41.8610879399662));
#33925=CARTESIAN_POINT('',(-39.6882902068655,56.7624179651878,42.8308734094728));
#33926=CARTESIAN_POINT('Origin',(-36.6676052751974,62.4851867637248,38.7277794765853));
#33927=CARTESIAN_POINT('',(-38.7873697728656,55.7663207511003,42.6252145919964));
#33928=CARTESIAN_POINT('Origin',(-34.6286398902921,61.2796593448501,38.6280357975872));
#33929=CARTESIAN_POINT('',(-38.7033067843916,56.8717526272238,43.7448778970514));
#33930=CARTESIAN_POINT('Origin',(-35.3279590748654,61.2947308388206,38.016022662737));
#33931=CARTESIAN_POINT('',(-38.296523342403,55.6344840136914,42.8580939635258));
#33932=CARTESIAN_POINT('Origin',(-34.5098422368239,61.0749923461824,38.4041736673213));
#33933=CARTESIAN_POINT('',(-37.5464148739375,56.1871303837669,43.8470743034192));
#33934=CARTESIAN_POINT('Origin',(-35.3425983346016,61.4714218719905,38.2893021662718));
#33935=CARTESIAN_POINT('',(-36.6630769135403,55.5112871226107,43.5547560965436));
#33936=CARTESIAN_POINT('Origin',(-33.8117714979599,61.7181366551636,40.0827140018471));
#33937=CARTESIAN_POINT('',(-37.4131853820058,54.9586407525351,42.5657757566501));
#33938=CARTESIAN_POINT('Origin',(-34.4592603742044,60.7955786108343,37.9969839593961));
#33939=CARTESIAN_POINT('',(-35.8766253111206,54.7090541915238,42.8094596350493));
#33940=CARTESIAN_POINT('Origin',(-34.92222282311,61.3905053805684,38.5406405225208));
#33941=CARTESIAN_POINT('',(-37.2967369646954,54.6258352478992,42.1319276178937));
#33942=CARTESIAN_POINT('Origin',(-34.7281327675399,60.8358027888048,37.8175254188111));
#33943=CARTESIAN_POINT('',(-36.1549383652767,54.0590449205628,41.6616005819702));
#33944=CARTESIAN_POINT('Origin',(-34.6286398902921,61.2796593448501,38.6280357975872));
#33945=CARTESIAN_POINT('',(-36.6995172934982,53.7667267136871,40.6918151124636));
#33946=CARTESIAN_POINT('Origin',(-33.1342534336086,59.7818137190999,37.5585066490826));
#33947=CARTESIAN_POINT('',(-37.8413158929169,54.3335170410235,41.1621421483871));
#33948=CARTESIAN_POINT('Origin',(-35.1732188185136,60.9873411379744,37.6582503280806));
#33949=CARTESIAN_POINT('',(-37.6192778814294,53.7736359295216,39.7061461326282));
#33950=CARTESIAN_POINT('Origin',(-34.4738996339406,60.972269644004,38.2702634629306));
#33951=CARTESIAN_POINT('',(-38.3321623233795,54.4653537784324,40.9292627768577));
#33952=CARTESIAN_POINT('Origin',(-35.292016471982,61.1920081366421,37.8821124583463));
#33953=CARTESIAN_POINT('',(-38.8413926264262,54.342014295108,39.6756142185172));
#33954=CARTESIAN_POINT('Origin',(-34.4592603742044,60.7955786108343,37.9969839593961));
#33955=CARTESIAN_POINT('',(-39.7247305868234,55.0178575562642,39.9679324253928));
#33956=CARTESIAN_POINT('Origin',(-35.9900872108458,60.5488638276609,36.2035721238207));
#33957=CARTESIAN_POINT('',(-39.2155002837767,55.1411970395887,41.2215809837334));
#33958=CARTESIAN_POINT('Origin',(-35.3425983346016,61.4714218719905,38.2893021662718));
#33959=CARTESIAN_POINT('',(-40.4459593547004,55.9363343652216,40.6415643946303));
#33960=CARTESIAN_POINT('Origin',(-34.8796358856957,60.8764951022562,37.7456456031473));
#33961=CARTESIAN_POINT('',(-39.3319487010871,55.4740025442247,41.6554291224898));
#33962=CARTESIAN_POINT('Origin',(-35.0737259412659,61.4311976940199,38.468760706857));
#33963=CARTESIAN_POINT('Origin',(-35.1732188185136,60.9873411379744,37.6582503280806));
#33964=CARTESIAN_POINT('Origin',(-36.8403461265623,57.6769603963792,40.2741040863097));
#33965=CARTESIAN_POINT('',(-38.0545418955644,56.8104949709136,38.6082810762002));
#33966=CARTESIAN_POINT('Origin',(-37.012738728532,57.369712410154,40.463522843952));
#33967=CARTESIAN_POINT('',(-37.696662681666,57.2124706447442,38.7603610476862));
#33968=CARTESIAN_POINT('Origin',(-37.8821492935947,57.1177429571387,38.418862318558));
#33969=CARTESIAN_POINT('Origin',(-36.8442301901646,57.6700379953797,40.2783717549553));
#33970=CARTESIAN_POINT('Origin',(-36.8442301901646,57.6700379953797,40.2783717549553));
#33971=CARTESIAN_POINT('',(-37.4056077410637,57.7224461315386,38.4608120751962));
#33972=CARTESIAN_POINT('',(-37.696662681666,57.2124706447442,38.7603610476862));
#33973=CARTESIAN_POINT('',(-35.7148085556595,58.6300306164513,41.471785135086));
#33974=CARTESIAN_POINT('Origin',(-36.5602081483616,58.1762383739949,39.9662986051411));
#33975=CARTESIAN_POINT('Origin',(-36.5602081483616,58.1762383739949,39.9662986051411));
#33976=CARTESIAN_POINT('Origin',(-36.5602081483616,58.1762383739949,39.9662986051411));
#33977=CARTESIAN_POINT('',(-37.0547713564024,58.4743848476173,37.7824909411013));
#33978=CARTESIAN_POINT('',(-35.1605837799799,59.4911438280544,41.155657791559));
#33979=CARTESIAN_POINT('Origin',(-36.1076775681912,58.9827643378359,39.4690743663302));
#33980=CARTESIAN_POINT('',(-35.7148085556595,58.6300306164513,41.471785135086));
#33981=CARTESIAN_POINT('Origin',(-36.1076775681912,58.9827643378359,39.4690743663302));
#33982=CARTESIAN_POINT('Origin',(-28.393108630048,72.7321117214098,30.9925849618393));
#33983=CARTESIAN_POINT('',(-29.3402024182593,72.2237322311912,29.3060015366105));
#33984=CARTESIAN_POINT('Origin',(-28.393108630048,72.7321117214098,30.9925849618393));
#33985=CARTESIAN_POINT('',(-29.3402024182593,72.2237322311912,29.3060015366105));
#33986=CARTESIAN_POINT('Origin',(-29.9293485611736,73.9074913060293,31.5009644520579));
#33987=CARTESIAN_POINT('Origin',(-40.0852185907832,59.7204715793931,41.4802818243891));
#33988=CARTESIAN_POINT('Origin',(-39.1543717028682,54.3387298731897,43.2616154689789));
#33989=CARTESIAN_POINT('',(-37.6311300310271,56.8203861500479,42.1269838523944));
#33990=CARTESIAN_POINT('',(-38.9671726962921,54.4392142568033,43.5949792241218));
#33991=CARTESIAN_POINT('',(-37.001460645271,57.1583790767479,43.2482983015114));
#33992=CARTESIAN_POINT('',(-37.8183290376032,56.7199017664344,41.7936200972515));
#33993=CARTESIAN_POINT('',(-38.337503310536,54.7772071835033,44.7162936732388));
#33994=CARTESIAN_POINT('Origin',(-40.4793786434641,55.3524947649241,43.7000927792924));
#33995=CARTESIAN_POINT('',(-39.143335978199,57.7336666581687,42.232097407565));
#33996=CARTESIAN_POINT('',(-38.1219764614898,56.9522228874568,41.894104480865));
#33997=CARTESIAN_POINT('',(-39.143335978199,57.7336666581687,42.232097407565));
#33998=CARTESIAN_POINT('',(-39.4580191267548,54.5710509942122,43.3620998525924));
#33999=CARTESIAN_POINT('',(-40.4793786434641,55.3524947649241,43.7000927792924));
#34000=CARTESIAN_POINT('Origin',(-41.0239575716855,55.0601765580484,42.7303073097858));
#34001=CARTESIAN_POINT('',(-39.6879149064205,57.4413484512931,41.2623119380584));
#34002=CARTESIAN_POINT('',(-41.0239575716855,55.0601765580484,42.7303073097858));
#34003=CARTESIAN_POINT('',(-39.6879149064205,57.4413484512931,41.2623119380584));
#34004=CARTESIAN_POINT('Origin',(-39.6989506310897,54.0464116663141,42.2918299994723));
#34005=CARTESIAN_POINT('',(-38.6665553897112,56.6599046805812,40.9243190113584));
#34006=CARTESIAN_POINT('',(-40.0025980549763,54.2787327873365,42.3923143830858));
#34007=CARTESIAN_POINT('',(-38.3629079658247,56.4275835595587,40.8238346277449));
#34008=CARTESIAN_POINT('Origin',(-41.2696592085703,54.4682892260227,41.5466160105783));
#34009=CARTESIAN_POINT('',(-39.9336165433053,56.8494611192673,40.0786206388509));
#34010=CARTESIAN_POINT('',(-41.2696592085703,54.4682892260227,41.5466160105783));
#34011=CARTESIAN_POINT('',(-39.9336165433053,56.8494611192673,40.0786206388509));
#34012=CARTESIAN_POINT('Origin',(-39.2572816508911,53.708490035736,42.1456708960345));
#34013=CARTESIAN_POINT('',(-38.5501069724008,56.3270991759452,40.490470872602));
#34014=CARTESIAN_POINT('',(-39.8861496376659,53.9459272827006,41.9584662443294));
#34015=CARTESIAN_POINT('',(-37.9212389856261,56.0896619289806,40.677675524307));
#34016=CARTESIAN_POINT('Origin',(-40.5158190234219,53.6079343560005,40.8371517952124));
#34017=CARTESIAN_POINT('',(-39.1797763581569,55.9891062492452,39.369156423485));
#34018=CARTESIAN_POINT('',(-39.1797763581569,55.9891062492452,39.369156423485));
#34019=CARTESIAN_POINT('',(-40.5158190234219,53.6079343560005,40.8371517952124));
#34020=CARTESIAN_POINT('Origin',(-39.6324810630247,52.9320910948443,40.5448335883368));
#34021=CARTESIAN_POINT('',(-38.2964383977597,55.313262988089,39.0768382166093));
#34022=CARTESIAN_POINT('',(-39.6324810630247,52.9320910948443,40.5448335883368));
#34023=CARTESIAN_POINT('',(-38.2964383977597,55.313262988089,39.0768382166093));
#34024=CARTESIAN_POINT('Origin',(-38.8156126706925,53.3705684051578,41.9995117925966));
#34025=CARTESIAN_POINT('',(-37.6667690120036,55.651255914789,40.1981526657263));
#34026=CARTESIAN_POINT('',(-39.0028116772686,53.2700840215443,41.6661480374538));
#34027=CARTESIAN_POINT('',(-37.4795700054275,55.7517402984025,40.5315164208692));
#34028=CARTESIAN_POINT('Origin',(-38.4429777352992,52.3055907903227,40.6111977485762));
#34029=CARTESIAN_POINT('',(-37.1069350700342,54.6867626835674,39.1432023768487));
#34030=CARTESIAN_POINT('',(-38.4429777352992,52.3055907903227,40.6111977485762));
#34031=CARTESIAN_POINT('',(-37.1069350700342,54.6867626835674,39.1432023768487));
#34032=CARTESIAN_POINT('Origin',(-38.5433232065818,53.5167275085957,42.48440452735));
#34033=CARTESIAN_POINT('',(-37.1759225815409,55.51941917738,40.4310320372557));
#34034=CARTESIAN_POINT('',(-38.511965246806,53.1382472841354,41.8990274089831));
#34035=CARTESIAN_POINT('',(-37.2072805413167,55.8978994018403,41.0164091556225));
#34036=CARTESIAN_POINT('Origin',(-37.4906057300967,52.3568035134235,41.5610344822831));
#34037=CARTESIAN_POINT('',(-36.1545630648317,54.7379754066681,40.0930391105557));
#34038=CARTESIAN_POINT('',(-36.1545630648317,54.7379754066681,40.0930391105557));
#34039=CARTESIAN_POINT('',(-37.4906057300967,52.3568035134235,41.5610344822831));
#34040=CARTESIAN_POINT('Origin',(-36.9460268018752,52.6491217202992,42.5308199517897));
#34041=CARTESIAN_POINT('',(-35.6099841366102,55.0302936135438,41.0628245800623));
#34042=CARTESIAN_POINT('',(-36.9460268018752,52.6491217202992,42.5308199517897));
#34043=CARTESIAN_POINT('',(-35.6099841366102,55.0302936135438,41.0628245800623));
#34044=CARTESIAN_POINT('Origin',(-38.271033742471,53.6628866120335,42.9692972621033));
#34045=CARTESIAN_POINT('',(-36.6313436533195,55.8117373842557,41.4008175067623));
#34046=CARTESIAN_POINT('',(-37.9673863185845,53.4305654910111,42.8688128784897));
#34047=CARTESIAN_POINT('',(-36.934991077206,56.0440585052782,41.5013018903758));
#34048=CARTESIAN_POINT('Origin',(-36.7003251649905,53.2410090523249,43.7145112509973));
#34049=CARTESIAN_POINT('',(-35.3642824997255,55.6221809455696,42.2465158792698));
#34050=CARTESIAN_POINT('',(-36.7003251649905,53.2410090523249,43.7145112509973));
#34051=CARTESIAN_POINT('',(-35.3642824997255,55.6221809455696,42.2465158792698));
#34052=CARTESIAN_POINT('Origin',(-38.7127027226696,54.0008082426116,43.1154563655411));
#34053=CARTESIAN_POINT('',(-36.7477920706299,56.1445428888917,41.8346656455187));
#34054=CARTESIAN_POINT('',(-38.0838347358949,53.763370995647,43.3026610172461));
#34055=CARTESIAN_POINT('',(-37.3766600574046,56.3819801358563,41.6474609938136));
#34056=CARTESIAN_POINT('Origin',(-37.4541653501388,54.101363922347,44.4239754663631));
#34057=CARTESIAN_POINT('',(-36.1181226848738,56.4825358155917,42.9559800946357));
#34058=CARTESIAN_POINT('',(-36.1181226848738,56.4825358155917,42.9559800946357));
#34059=CARTESIAN_POINT('',(-37.4541653501388,54.101363922347,44.4239754663631));
#34060=CARTESIAN_POINT('Origin',(-38.337503310536,54.7772071835033,44.7162936732388));
#34061=CARTESIAN_POINT('',(-37.001460645271,57.1583790767479,43.2482983015114));
#34062=CARTESIAN_POINT('Origin',(-36.1181226848738,56.4825358155917,42.9559800946357));
#34063=CARTESIAN_POINT('',(-38.1909639729965,57.7848793812695,43.181934141272));
#34064=CARTESIAN_POINT('',(-38.090618501714,56.5737426629966,41.3087273624982));
#34065=CARTESIAN_POINT('',(-38.1909639729965,57.7848793812695,43.181934141272));
#34066=CARTESIAN_POINT('Origin',(-39.5270066382616,55.4037074880248,44.6499295129994));
#34067=CARTESIAN_POINT('',(-39.5270066382616,55.4037074880248,44.6499295129994));
#34068=CARTESIAN_POINT('Origin',(-39.426661166979,54.1925707697519,42.7767227342256));
#34069=CARTESIAN_POINT('',(0.,0.,0.));
#34070=CARTESIAN_POINT('Ctrl Pts',(-1.77573785876366E-15,38.6077491572282,
14.5682581662533));
#34071=CARTESIAN_POINT('Ctrl Pts',(-1.77573785876366E-15,37.4339720363476,
14.8177521952346));
#34072=CARTESIAN_POINT('Ctrl Pts',(29.,38.6077491572282,14.5682581662533));
#34073=CARTESIAN_POINT('Ctrl Pts',(29.,37.4339720363476,14.8177521952346));
#34074=CARTESIAN_POINT('Ctrl Pts',(29.,32.3703984326954,-14.7761698557608));
#34075=CARTESIAN_POINT('Ctrl Pts',(29.,31.1966213118148,-14.5266758267795));
#34076=CARTESIAN_POINT('Ctrl Pts',(0.,32.3703984326954,-14.7761698557608));
#34077=CARTESIAN_POINT('Ctrl Pts',(0.,31.1966213118148,-14.5266758267795));
#34078=CARTESIAN_POINT('',(-1.77573785876366E-15,38.6077491572282,14.5682581662533));
#34079=CARTESIAN_POINT('',(13.9832936034398,36.3141977378119,3.77794710083046));
#34080=CARTESIAN_POINT('Origin',(6.26496290550477E-13,35.489073794962,-0.103955844753016));
#34081=CARTESIAN_POINT('',(-1.77573785876366E-15,37.6296015564944,14.7761698570711));
#34082=CARTESIAN_POINT('',(-1.77573785876366E-15,38.6077491572282,14.5682581662533));
#34083=CARTESIAN_POINT('',(13.9832936034398,35.3360501370781,3.98585879164823));
#34084=CARTESIAN_POINT('Origin',(-4.06952304038461E-13,34.5109261942279,
0.103955846063604));
#34085=CARTESIAN_POINT('',(13.9832936034398,33.6858022513779,-3.77794709952022));
#34086=CARTESIAN_POINT('Origin',(1.71995750974929E-11,34.510926194228,0.103955846063976));
#34087=CARTESIAN_POINT('',(0.,31.3922508319616,-14.5682581649431));
#34088=CARTESIAN_POINT('Origin',(-7.105427357601E-14,34.510926194228,0.10395584606411));
#34089=CARTESIAN_POINT('',(0.,32.3703984326954,-14.7761698557608));
#34090=CARTESIAN_POINT('',(0.,32.3703984326954,-14.7761698557608));
#34091=CARTESIAN_POINT('',(13.9832936034398,34.6639498521117,-3.98585879033799));
#34092=CARTESIAN_POINT('Origin',(-2.22044604925031E-14,35.4890737949618,
-0.103955844753743));
#34093=CARTESIAN_POINT('Origin',(2.6754154447417E-11,35.4890737949615,-0.103955844754103));
#34094=CARTESIAN_POINT('Origin',(7.49999972068901,37.9344427967963,-0.62373507179816));
#34095=CARTESIAN_POINT('',(8.91421328306212,32.6156398209602,3.21167037016454));
#34096=CARTESIAN_POINT('',(6.08578615831592,32.6156398209602,3.21167037016456));
#34097=CARTESIAN_POINT('Origin',(7.499999720689,32.0655571923935,0.6237350731084));
#34098=CARTESIAN_POINT('',(6.08578615831588,31.5154745638267,-1.96420022394774));
#34099=CARTESIAN_POINT('Origin',(7.499999720689,32.0655571923935,0.6237350731084));
#34100=CARTESIAN_POINT('',(7.499999720689,31.4418221199402,-2.31070772909302));
#34101=CARTESIAN_POINT('Origin',(7.499999720689,32.0655571923935,0.6237350731084));
#34102=CARTESIAN_POINT('',(7.499999720689,29.8805494572643,-1.97884898008522));
#34103=CARTESIAN_POINT('',(7.49999972068901,37.310707724343,-3.55817787399958));
#34104=CARTESIAN_POINT('Origin',(7.499999720689,30.5042845297176,0.955593822116194));
#34105=CARTESIAN_POINT('',(8.91421328306212,31.5154745638267,-1.96420022394774));
#34106=CARTESIAN_POINT('Origin',(7.499999720689,32.0655571923935,0.6237350731084));
#34107=CARTESIAN_POINT('Origin',(7.499999720689,32.0655571923935,0.6237350731084));
#34108=CARTESIAN_POINT('Origin',(7.49999972068907,35.5868885550352,-0.124747013835536));
#34109=CARTESIAN_POINT('',(5.949999720689,29.8493353829967,0.698650580301697));
#34110=CARTESIAN_POINT('',(5.949999720689,30.0104669433805,1.4567149708704));
#34111=CARTESIAN_POINT('Origin',(5.949999720689,35.5868885550352,-0.124747013835536));
#34112=CARTESIAN_POINT('',(6.846093470689,29.8458529108876,1.49170476361971));
#34113=CARTESIAN_POINT('Origin',(7.49999972068907,35.6674543352271,0.254285181448814));
#34114=CARTESIAN_POINT('',(6.259999720689,30.2320748221203,2.28115611924892));
#34115=CARTESIAN_POINT('Origin',(7.23686974721422,35.5492769441233,-0.301695730997491));
#34116=CARTESIAN_POINT('',(7.112499720689,29.9012418847696,1.7522893978777));
#34117=CARTESIAN_POINT('Origin',(7.68090157745298,35.6415963527252,0.13263293839996));
#34118=CARTESIAN_POINT('',(7.112499720689,30.2521642839561,2.59381155672345));
#34119=CARTESIAN_POINT('Origin',(7.112499720689,35.5868885550352,-0.124747013835536));
#34120=CARTESIAN_POINT('',(7.887499720689,30.2521642839561,2.59381155672345));
#34121=CARTESIAN_POINT('Origin',(7.49999972068907,35.9091516758027,1.39138176730186));
#34122=CARTESIAN_POINT('',(7.887499720689,29.9012418847695,1.7522893978777));
#34123=CARTESIAN_POINT('Origin',(7.88749972068901,35.5868885550352,-0.124747013835536));
#34124=CARTESIAN_POINT('',(8.739999720689,30.2320748221202,2.28115611924892));
#34125=CARTESIAN_POINT('Origin',(7.31909786392512,35.6415963527252,0.132632938400021));
#34126=CARTESIAN_POINT('',(8.153905970689,29.8458529108876,1.49170476361971));
#34127=CARTESIAN_POINT('Origin',(7.76312969416383,35.5492769441233,-0.30169573099743));
#34128=CARTESIAN_POINT('',(9.049999720689,30.0104669433804,1.45671497087041));
#34129=CARTESIAN_POINT('Origin',(7.49999972068907,35.6674543352271,0.254285181448814));
#34130=CARTESIAN_POINT('',(9.049999720689,29.8493353829967,0.698650580301706));
#34131=CARTESIAN_POINT('Origin',(9.04999972068901,35.5868885550352,-0.124747013835536));
#34132=CARTESIAN_POINT('',(8.153905970689,29.6847213505039,0.733640373051015));
#34133=CARTESIAN_POINT('Origin',(7.49999972068907,35.5063227748433,-0.503779209119886));
#34134=CARTESIAN_POINT('',(8.739999720689,29.7164538288922,-0.144649930570914));
#34135=CARTESIAN_POINT('Origin',(7.76312969416383,35.624500165947,0.0522017033263585));
#34136=CARTESIAN_POINT('',(7.887499720689,29.6293323766219,0.473055738793025));
#34137=CARTESIAN_POINT('Origin',(7.31909786392512,35.5321807573452,-0.382126966071094));
#34138=CARTESIAN_POINT('',(7.887499720689,29.607638042421,-0.438446005551347));
#34139=CARTESIAN_POINT('Origin',(7.88749972068901,35.5868885550352,-0.124747013835536));
#34140=CARTESIAN_POINT('',(7.112499720689,29.6076380424211,-0.438446005551349));
#34141=CARTESIAN_POINT('Origin',(7.49999972068907,35.2646254342677,-1.64087579497293));
#34142=CARTESIAN_POINT('',(7.112499720689,29.629332376622,0.473055738793022));
#34143=CARTESIAN_POINT('Origin',(7.112499720689,35.5868885550352,-0.124747013835536));
#34144=CARTESIAN_POINT('',(6.259999720689,29.7164538288922,-0.144649930570921));
#34145=CARTESIAN_POINT('Origin',(7.68090157745298,35.5321807573452,-0.382126966071032));
#34146=CARTESIAN_POINT('',(6.846093470689,29.6847213505039,0.733640373051013));
#34147=CARTESIAN_POINT('Origin',(7.23686974721422,35.6245001659471,0.0522017033264189));
#34148=CARTESIAN_POINT('Origin',(7.49999972068907,35.5063227748433,-0.503779209119886));
#34149=CARTESIAN_POINT('Origin',(22.5,34.9999999945949,6.55125051005245E-10));
#34150=CARTESIAN_POINT('',(22.5,34.1683532313239,-3.9125904022801));
#34151=CARTESIAN_POINT('Origin',(22.5,34.9999999945949,6.55125051005245E-10));
#34152=CARTESIAN_POINT('',(14.55,34.1683532313239,-3.9125904022801));
#34153=CARTESIAN_POINT('',(22.5,34.1683532313239,-3.9125904022801));
#34154=CARTESIAN_POINT('',(14.55,34.6639498521117,-3.98585879033799));
#34155=CARTESIAN_POINT('Origin',(14.55,34.9999999945949,6.55125051005245E-10));
#34156=CARTESIAN_POINT('',(14.55,34.6639498521117,-3.98585879033799));
#34157=CARTESIAN_POINT('',(-13.9832936034398,34.6639498521117,-3.98585879033799));
#34158=CARTESIAN_POINT('',(14.55,34.6639498521117,-3.98585879033799));
#34159=CARTESIAN_POINT('',(-14.55,34.6639498521117,-3.98585879033799));
#34160=CARTESIAN_POINT('',(14.55,34.6639498521117,-3.98585879033799));
#34161=CARTESIAN_POINT('',(-14.55,34.1683532313239,-3.9125904022801));
#34162=CARTESIAN_POINT('Origin',(-14.55,34.9999999945949,6.55125051005245E-10));
#34163=CARTESIAN_POINT('',(-22.5,34.1683532313239,-3.9125904022801));
#34164=CARTESIAN_POINT('',(22.5,34.1683532313239,-3.9125904022801));
#34165=CARTESIAN_POINT('Origin',(-22.5,34.9999999945949,6.55125051005245E-10));
#34166=CARTESIAN_POINT('',(-14.55,33.6858022513779,-3.77794709952022));
#34167=CARTESIAN_POINT('Origin',(-14.55,34.9999999945949,6.55125051005245E-10));
#34168=CARTESIAN_POINT('',(-13.9832936034398,33.6858022513779,-3.77794709952022));
#34169=CARTESIAN_POINT('',(14.55,33.6858022513779,-3.77794709952022));
#34170=CARTESIAN_POINT('',(14.55,33.6858022513779,-3.77794709952022));
#34171=CARTESIAN_POINT('',(14.55,33.6858022513779,-3.77794709952022));
#34172=CARTESIAN_POINT('',(14.55,33.6858022513779,-3.77794709952022));
#34173=CARTESIAN_POINT('Origin',(14.55,34.9999999945949,6.55125051005245E-10));
#34174=CARTESIAN_POINT('',(-14.55,35.3360501370781,3.98585879164823));
#34175=CARTESIAN_POINT('',(-14.55,36.3141977378119,3.77794710083046));
#34176=CARTESIAN_POINT('Origin',(-14.55,34.9999999945949,6.55125051005245E-10));
#34177=CARTESIAN_POINT('',(-13.9832936034398,36.3141977378119,3.77794710083047));
#34178=CARTESIAN_POINT('',(14.55,36.3141977378119,3.77794710083046));
#34179=CARTESIAN_POINT('',(14.55,36.3141977378119,3.77794710083046));
#34180=CARTESIAN_POINT('',(14.55,36.3141977378119,3.77794710083046));
#34181=CARTESIAN_POINT('',(14.55,36.3141977378119,3.77794710083046));
#34182=CARTESIAN_POINT('',(14.55,35.3360501370781,3.98585879164823));
#34183=CARTESIAN_POINT('Origin',(14.55,34.9999999945949,6.55125051005245E-10));
#34184=CARTESIAN_POINT('',(14.55,35.3360501370781,3.98585879164823));
#34185=CARTESIAN_POINT('',(-13.9832936034398,35.3360501370781,3.98585879164823));
#34186=CARTESIAN_POINT('',(14.55,35.3360501370781,3.98585879164823));
#34187=CARTESIAN_POINT('',(14.55,35.3360501370781,3.98585879164823));
#34188=CARTESIAN_POINT('',(14.55,38.4845254253631,1.96420022525798));
#34189=CARTESIAN_POINT('',(14.55,37.3843601682296,-3.21167036885432));
#34190=CARTESIAN_POINT('Origin',(14.55,34.9999999945949,6.55114870111609E-10));
#34191=CARTESIAN_POINT('',(-14.55,38.4845254253631,1.96420022525798));
#34192=CARTESIAN_POINT('',(14.55,38.4845254253631,1.96420022525798));
#34193=CARTESIAN_POINT('',(-14.55,37.3843601682296,-3.21167036885432));
#34194=CARTESIAN_POINT('Origin',(-14.55,34.9999999945949,6.55114870111609E-10));
#34195=CARTESIAN_POINT('',(14.55,37.3843601682296,-3.21167036885432));
#34196=CARTESIAN_POINT('',(14.55,31.5154745638267,-1.96420022394774));
#34197=CARTESIAN_POINT('',(14.55,32.6156398209602,3.21167037016456));
#34198=CARTESIAN_POINT('Origin',(14.55,34.9999999945949,6.55125051005245E-10));
#34199=CARTESIAN_POINT('',(14.55,31.5154745638267,-1.96420022394774));
#34200=CARTESIAN_POINT('',(14.55,31.5154745638267,-1.96420022394774));
#34201=CARTESIAN_POINT('',(-6.08578624028789,31.5154745638267,-1.96420022394774));
#34202=CARTESIAN_POINT('',(14.55,31.5154745638267,-1.96420022394774));
#34203=CARTESIAN_POINT('',(-8.91421336503412,31.5154745638267,-1.96420022394774));
#34204=CARTESIAN_POINT('',(14.55,31.5154745638267,-1.96420022394774));
#34205=CARTESIAN_POINT('',(-14.55,31.5154745638267,-1.96420022394774));
#34206=CARTESIAN_POINT('',(14.55,31.5154745638267,-1.96420022394774));
#34207=CARTESIAN_POINT('',(-14.55,32.6156398209602,3.21167037016456));
#34208=CARTESIAN_POINT('Origin',(-14.55,34.9999999945949,6.55125051005245E-10));
#34209=CARTESIAN_POINT('',(-8.91421336503407,32.6156398209602,3.21167037016456));
#34210=CARTESIAN_POINT('',(14.55,32.6156398209602,3.21167037016456));
#34211=CARTESIAN_POINT('',(-6.08578624028785,32.6156398209602,3.21167037016452));
#34212=CARTESIAN_POINT('',(14.55,32.6156398209602,3.21167037016456));
#34213=CARTESIAN_POINT('',(14.55,32.6156398209602,3.21167037016456));
#34214=CARTESIAN_POINT('',(14.55,32.6156398209602,3.21167037016456));
#34215=CARTESIAN_POINT('',(14.55,32.6156398209602,3.21167037016456));
#34216=CARTESIAN_POINT('Origin',(-7.49999980266093,35.5868885550352,-0.124747013835536));
#34217=CARTESIAN_POINT('',(-7.499999802661,29.8805494572643,-1.97884898008522));
#34218=CARTESIAN_POINT('Origin',(-7.499999802661,30.5042845297176,0.955593822116194));
#34219=CARTESIAN_POINT('',(-9.049999802661,29.8493353829967,0.698650580301697));
#34220=CARTESIAN_POINT('',(-9.049999802661,30.0104669433805,1.4567149708704));
#34221=CARTESIAN_POINT('Origin',(-9.049999802661,35.5868885550352,-0.124747013835536));
#34222=CARTESIAN_POINT('',(-8.153906052661,29.8458529108876,1.49170476361971));
#34223=CARTESIAN_POINT('Origin',(-7.49999980266093,35.6674543352271,0.254285181448814));
#34224=CARTESIAN_POINT('',(-8.739999802661,30.2320748221203,2.28115611924892));
#34225=CARTESIAN_POINT('Origin',(-7.76312977613578,35.5492769441233,-0.301695730997491));
#34226=CARTESIAN_POINT('',(-7.887499802661,29.9012418847696,1.7522893978777));
#34227=CARTESIAN_POINT('Origin',(-7.31909794589703,35.6415963527252,0.13263293839996));
#34228=CARTESIAN_POINT('',(-7.887499802661,30.2521642839561,2.59381155672345));
#34229=CARTESIAN_POINT('Origin',(-7.887499802661,35.5868885550352,-0.124747013835536));
#34230=CARTESIAN_POINT('',(-7.112499802661,30.2521642839561,2.59381155672345));
#34231=CARTESIAN_POINT('Origin',(-7.49999980266093,35.9091516758027,1.39138176730186));
#34232=CARTESIAN_POINT('',(-7.112499802661,29.9012418847695,1.7522893978777));
#34233=CARTESIAN_POINT('Origin',(-7.112499802661,35.5868885550352,-0.124747013835536));
#34234=CARTESIAN_POINT('',(-6.259999802661,30.2320748221202,2.28115611924892));
#34235=CARTESIAN_POINT('Origin',(-7.68090165942488,35.6415963527252,0.132632938400021));
#34236=CARTESIAN_POINT('',(-6.846093552661,29.8458529108876,1.49170476361971));
#34237=CARTESIAN_POINT('Origin',(-7.23686982918617,35.5492769441233,-0.30169573099743));
#34238=CARTESIAN_POINT('',(-5.949999802661,30.0104669433804,1.45671497087041));
#34239=CARTESIAN_POINT('Origin',(-7.49999980266093,35.6674543352271,0.254285181448814));
#34240=CARTESIAN_POINT('',(-5.949999802661,29.8493353829967,0.698650580301706));
#34241=CARTESIAN_POINT('Origin',(-5.949999802661,35.5868885550352,-0.124747013835536));
#34242=CARTESIAN_POINT('',(-6.846093552661,29.6847213505039,0.733640373051015));
#34243=CARTESIAN_POINT('Origin',(-7.49999980266093,35.5063227748433,-0.503779209119886));
#34244=CARTESIAN_POINT('',(-6.259999802661,29.7164538288922,-0.144649930570914));
#34245=CARTESIAN_POINT('Origin',(-7.23686982918617,35.624500165947,0.0522017033263585));
#34246=CARTESIAN_POINT('',(-7.112499802661,29.6293323766219,0.473055738793025));
#34247=CARTESIAN_POINT('Origin',(-7.68090165942488,35.5321807573452,-0.382126966071094));
#34248=CARTESIAN_POINT('',(-7.112499802661,29.607638042421,-0.438446005551347));
#34249=CARTESIAN_POINT('Origin',(-7.112499802661,35.5868885550352,-0.124747013835536));
#34250=CARTESIAN_POINT('',(-7.887499802661,29.6076380424211,-0.438446005551349));
#34251=CARTESIAN_POINT('Origin',(-7.49999980266093,35.2646254342677,-1.64087579497293));
#34252=CARTESIAN_POINT('',(-7.887499802661,29.629332376622,0.473055738793022));
#34253=CARTESIAN_POINT('Origin',(-7.887499802661,35.5868885550352,-0.124747013835536));
#34254=CARTESIAN_POINT('',(-8.739999802661,29.7164538288922,-0.144649930570921));
#34255=CARTESIAN_POINT('Origin',(-7.31909794589703,35.5321807573452,-0.382126966071032));
#34256=CARTESIAN_POINT('',(-8.153906052661,29.6847213505039,0.733640373051013));
#34257=CARTESIAN_POINT('Origin',(-7.76312977613578,35.6245001659471,0.0522017033264189));
#34258=CARTESIAN_POINT('Origin',(-7.49999980266093,35.5063227748433,-0.503779209119886));
#34259=CARTESIAN_POINT('Origin',(-7.49999980266099,37.9344427967963,-0.62373507179816));
#34260=CARTESIAN_POINT('Origin',(-7.499999802661,32.0655571923935,0.6237350731084));
#34261=CARTESIAN_POINT('Origin',(-7.499999802661,32.0655571923935,0.6237350731084));
#34262=CARTESIAN_POINT('',(-7.499999802661,31.4418221199402,-2.31070772909302));
#34263=CARTESIAN_POINT('Origin',(-7.499999802661,32.0655571923935,0.6237350731084));
#34264=CARTESIAN_POINT('',(-7.49999980266099,37.310707724343,-3.55817787399958));
#34265=CARTESIAN_POINT('Origin',(-7.499999802661,32.0655571923935,0.6237350731084));
#34266=CARTESIAN_POINT('Origin',(-7.499999802661,32.0655571923935,0.6237350731084));
#34267=CARTESIAN_POINT('Origin',(14.55,35.3360501370781,3.98585879164823));
#34268=CARTESIAN_POINT('Origin',(-1.25033317033285E-11,34.5109261942281,
0.103955846063943));
#34269=CARTESIAN_POINT('',(-14.55,35.3360501370781,3.98585879164823));
#34270=CARTESIAN_POINT('Origin',(14.55,35.3360501370781,3.98585879164823));
#34271=CARTESIAN_POINT('',(14.55,35.3360501370781,3.98585879164823));
#34272=CARTESIAN_POINT('Origin',(14.55,34.6639498521117,-3.98585879033799));
#34273=CARTESIAN_POINT('Origin',(1.28297372725683E-11,35.4890737949616,
-0.103955844753872));
#34274=CARTESIAN_POINT('',(-14.55,34.6639498521117,-3.98585879033799));
#34275=CARTESIAN_POINT('Origin',(-10.499999802661,32.0655571923935,0.6237350731084));
#34276=CARTESIAN_POINT('Origin',(-7.887499802661,28.6001199783652,1.3603364920056));
#34277=CARTESIAN_POINT('',(-8.153906052661,31.0282400003182,1.24038062932732));
#34278=CARTESIAN_POINT('',(-8.15390605266101,28.6806857585571,1.73936868728995));
#34279=CARTESIAN_POINT('',(-8.739999802661,31.2054847167403,2.07425145895289));
#34280=CARTESIAN_POINT('',(-7.887499802661,30.9476742201263,0.861348434042974));
#34281=CARTESIAN_POINT('',(-8.739999802661,28.8579304749792,2.57323951691552));
#34282=CARTESIAN_POINT('Origin',(-8.739999802661,28.8579304749792,2.57323951691552));
#34283=CARTESIAN_POINT('',(-7.887499802661,31.0836289742001,1.50096526358531));
#34284=CARTESIAN_POINT('',(-8.739999802661,31.2054847167403,2.07425145895289));
#34285=CARTESIAN_POINT('',(-7.887499802661,28.736074732439,1.99995332154794));
#34286=CARTESIAN_POINT('Origin',(-7.112499802661,31.2699373408939,2.37747721518037));
#34287=CARTESIAN_POINT('',(-9.049999802661,31.0282400003182,1.24038062932732));
#34288=CARTESIAN_POINT('',(-9.049999802661,31.0282400003182,1.24038062932732));
#34289=CARTESIAN_POINT('',(-9.049999802661,30.8671084399344,0.482316238758624));
#34290=CARTESIAN_POINT('',(-9.049999802661,30.8671084399344,0.482316238758624));
#34291=CARTESIAN_POINT('',(-8.153906052661,30.8671084399344,0.482316238758625));
#34292=CARTESIAN_POINT('',(-7.887499802661,30.8671084399344,0.482316238758625));
#34293=CARTESIAN_POINT('',(-8.739999802661,30.6898637235123,-0.351554590866945));
#34294=CARTESIAN_POINT('',(-8.739999802661,30.6898637235123,-0.351554590866945));
#34295=CARTESIAN_POINT('',(-7.887499802661,30.8117194660525,0.221731604500634));
#34296=CARTESIAN_POINT('',(-7.499999802661,30.8671084399344,0.482316238758625));
#34297=CARTESIAN_POINT('',(-7.887499802661,30.6254110993588,-0.654780347094424));
#34298=CARTESIAN_POINT('',(-7.887499802661,30.6254110993588,-0.654780347094424));
#34299=CARTESIAN_POINT('',(-7.112499802661,30.6254110993588,-0.654780347094424));
#34300=CARTESIAN_POINT('',(-7.112499802661,30.6254110993588,-0.654780347094424));
#34301=CARTESIAN_POINT('',(-7.112499802661,30.8117194660525,0.221731604500634));
#34302=CARTESIAN_POINT('',(-7.112499802661,30.8671084399344,0.482316238758625));
#34303=CARTESIAN_POINT('',(-6.259999802661,30.6898637235123,-0.351554590866944));
#34304=CARTESIAN_POINT('',(-6.259999802661,30.6898637235123,-0.351554590866944));
#34305=CARTESIAN_POINT('',(-6.846093552661,30.8671084399344,0.482316238758625));
#34306=CARTESIAN_POINT('',(-7.112499802661,30.9476742201263,0.861348434042974));
#34307=CARTESIAN_POINT('',(-5.949999802661,30.8671084399344,0.482316238758625));
#34308=CARTESIAN_POINT('',(-5.949999802661,30.8671084399344,0.482316238758625));
#34309=CARTESIAN_POINT('',(-5.949999802661,31.0282400003182,1.24038062932732));
#34310=CARTESIAN_POINT('',(-5.949999802661,31.0282400003182,1.24038062932732));
#34311=CARTESIAN_POINT('',(-6.846093552661,31.0282400003182,1.24038062932732));
#34312=CARTESIAN_POINT('',(-7.112499802661,31.0282400003182,1.24038062932732));
#34313=CARTESIAN_POINT('',(-6.259999802661,31.2054847167403,2.07425145895289));
#34314=CARTESIAN_POINT('',(-6.259999802661,31.2054847167403,2.07425145895289));
#34315=CARTESIAN_POINT('',(-7.112499802661,31.0836289742001,1.50096526358531));
#34316=CARTESIAN_POINT('',(-7.499999802661,31.0282400003182,1.24038062932732));
#34317=CARTESIAN_POINT('',(-7.112499802661,31.2699373408939,2.37747721518037));
#34318=CARTESIAN_POINT('',(-7.112499802661,31.2699373408939,2.37747721518037));
#34319=CARTESIAN_POINT('',(-7.887499802661,31.2699373408939,2.37747721518037));
#34320=CARTESIAN_POINT('',(-7.887499802661,31.2699373408939,2.37747721518037));
#34321=CARTESIAN_POINT('',(-7.887499802661,31.0282400003182,1.24038062932732));
#34322=CARTESIAN_POINT('Origin',(-7.887499802661,28.9223830991327,2.876465273143));
#34323=CARTESIAN_POINT('',(-7.887499802661,28.9223830991327,2.876465273143));
#34324=CARTESIAN_POINT('',(-7.112499802661,28.9223830991327,2.876465273143));
#34325=CARTESIAN_POINT('Origin',(-7.112499802661,28.9223830991327,2.876465273143));
#34326=CARTESIAN_POINT('',(-7.112499802661,28.736074732439,1.99995332154794));
#34327=CARTESIAN_POINT('Origin',(-7.49999980266101,28.6806857585571,1.73936868728995));
#34328=CARTESIAN_POINT('',(-6.259999802661,28.8579304749792,2.57323951691552));
#34329=CARTESIAN_POINT('Origin',(-6.259999802661,28.8579304749792,2.57323951691552));
#34330=CARTESIAN_POINT('',(-6.846093552661,28.6806857585571,1.73936868728995));
#34331=CARTESIAN_POINT('Origin',(-7.112499802661,28.6806857585571,1.73936868728995));
#34332=CARTESIAN_POINT('',(-5.949999802661,28.6806857585571,1.73936868728995));
#34333=CARTESIAN_POINT('Origin',(-5.949999802661,28.6806857585571,1.73936868728995));
#34334=CARTESIAN_POINT('',(-5.949999802661,28.5195541981733,0.981304296721249));
#34335=CARTESIAN_POINT('Origin',(-5.949999802661,28.5195541981733,0.981304296721249));
#34336=CARTESIAN_POINT('',(-6.846093552661,28.5195541981733,0.981304296721249));
#34337=CARTESIAN_POINT('Origin',(-7.112499802661,28.6001199783652,1.3603364920056));
#34338=CARTESIAN_POINT('',(-6.259999802661,28.3423094817512,0.14743346709568));
#34339=CARTESIAN_POINT('Origin',(-6.259999802661,28.3423094817512,0.14743346709568));
#34340=CARTESIAN_POINT('',(-7.112499802661,28.4641652242914,0.720719662463259));
#34341=CARTESIAN_POINT('Origin',(-7.112499802661,28.5195541981733,0.981304296721249));
#34342=CARTESIAN_POINT('',(-7.112499802661,28.2778568575977,-0.1557922891318));
#34343=CARTESIAN_POINT('Origin',(-7.112499802661,28.2778568575977,-0.1557922891318));
#34344=CARTESIAN_POINT('',(-7.887499802661,28.2778568575977,-0.1557922891318));
#34345=CARTESIAN_POINT('Origin',(-7.887499802661,28.2778568575977,-0.1557922891318));
#34346=CARTESIAN_POINT('',(-7.887499802661,28.4641652242914,0.720719662463258));
#34347=CARTESIAN_POINT('Origin',(-7.49999980266101,28.5195541981733,0.981304296721249));
#34348=CARTESIAN_POINT('',(-8.739999802661,28.3423094817512,0.14743346709568));
#34349=CARTESIAN_POINT('Origin',(-8.739999802661,28.3423094817512,0.14743346709568));
#34350=CARTESIAN_POINT('',(-8.15390605266101,28.5195541981733,0.981304296721249));
#34351=CARTESIAN_POINT('Origin',(-7.887499802661,28.5195541981733,0.981304296721249));
#34352=CARTESIAN_POINT('',(-9.049999802661,28.5195541981733,0.981304296721248));
#34353=CARTESIAN_POINT('Origin',(-9.049999802661,28.5195541981733,0.981304296721248));
#34354=CARTESIAN_POINT('',(-9.049999802661,28.6806857585571,1.73936868728995));
#34355=CARTESIAN_POINT('Origin',(-9.049999802661,28.6806857585571,1.73936868728995));
#34356=CARTESIAN_POINT('Origin',(-7.887499802661,28.6806857585571,1.73936868728995));
#34357=CARTESIAN_POINT('Origin',(-10.499999802661,32.0655571923935,0.6237350731084));
#34358=CARTESIAN_POINT('Origin',(14.55,32.6156398209602,3.21167037016456));
#34359=CARTESIAN_POINT('',(-14.55,32.6156398209602,3.21167037016456));
#34360=CARTESIAN_POINT('Origin',(14.55,32.6156398209602,3.21167037016456));
#34361=CARTESIAN_POINT('Origin',(22.5,34.9999999945949,6.55125051005245E-10));
#34362=CARTESIAN_POINT('Origin',(14.55,32.6768994428521,0.493790266347305));
#34363=CARTESIAN_POINT('',(14.55,34.6639498521117,-3.98585879033799));
#34364=CARTESIAN_POINT('Origin',(-14.55,32.6768994428521,0.493790266347305));
#34365=CARTESIAN_POINT('Origin',(-22.5,34.9999999945949,6.55125051005245E-10));
#34366=CARTESIAN_POINT('Origin',(14.55,32.6156398209602,3.21167037016456));
#34367=CARTESIAN_POINT('',(14.55,32.6156398209602,3.21167037016456));
#34368=CARTESIAN_POINT('Origin',(14.55,32.6768994428521,0.493790266347305));
#34369=CARTESIAN_POINT('Origin',(-14.55,32.6768994428521,0.493790266347305));
#34370=CARTESIAN_POINT('Origin',(-14.55,37.3231005463377,-0.493790265037065));
#34371=CARTESIAN_POINT('',(-14.55,37.3843601682296,-3.21167036885432));
#34372=CARTESIAN_POINT('Origin',(14.55,37.3843601682296,-3.21167036885432));
#34373=CARTESIAN_POINT('',(14.55,37.3843601682296,-3.21167036885432));
#34374=CARTESIAN_POINT('Origin',(14.55,37.3231005463377,-0.493790265037065));
#34375=CARTESIAN_POINT('Origin',(14.55,34.6639498521117,-3.98585879033799));
#34376=CARTESIAN_POINT('Origin',(7.887499720689,31.2699373408939,2.37747721518037));
#34377=CARTESIAN_POINT('',(6.846093470689,31.0282400003182,1.24038062932732));
#34378=CARTESIAN_POINT('',(6.259999720689,31.2054847167403,2.07425145895289));
#34379=CARTESIAN_POINT('',(7.112499720689,30.9476742201263,0.861348434042974));
#34380=CARTESIAN_POINT('',(5.949999720689,31.0282400003182,1.24038062932732));
#34381=CARTESIAN_POINT('',(5.949999720689,31.0282400003182,1.24038062932732));
#34382=CARTESIAN_POINT('',(5.949999720689,30.8671084399344,0.482316238758624));
#34383=CARTESIAN_POINT('',(5.949999720689,30.8671084399344,0.482316238758624));
#34384=CARTESIAN_POINT('',(6.846093470689,30.8671084399344,0.482316238758625));
#34385=CARTESIAN_POINT('',(7.112499720689,30.8671084399344,0.482316238758625));
#34386=CARTESIAN_POINT('',(6.259999720689,30.6898637235123,-0.351554590866945));
#34387=CARTESIAN_POINT('',(6.259999720689,30.6898637235123,-0.351554590866945));
#34388=CARTESIAN_POINT('',(7.112499720689,30.8117194660525,0.221731604500634));
#34389=CARTESIAN_POINT('',(7.499999720689,30.8671084399344,0.482316238758625));
#34390=CARTESIAN_POINT('',(7.112499720689,30.6254110993588,-0.654780347094424));
#34391=CARTESIAN_POINT('',(7.112499720689,30.6254110993588,-0.654780347094424));
#34392=CARTESIAN_POINT('',(7.887499720689,30.6254110993588,-0.654780347094424));
#34393=CARTESIAN_POINT('',(7.887499720689,30.6254110993588,-0.654780347094424));
#34394=CARTESIAN_POINT('',(7.887499720689,30.8117194660525,0.221731604500634));
#34395=CARTESIAN_POINT('',(7.887499720689,30.8671084399344,0.482316238758625));
#34396=CARTESIAN_POINT('',(8.739999720689,30.6898637235123,-0.351554590866944));
#34397=CARTESIAN_POINT('',(8.739999720689,30.6898637235123,-0.351554590866944));
#34398=CARTESIAN_POINT('',(8.153905970689,30.8671084399344,0.482316238758625));
#34399=CARTESIAN_POINT('',(7.887499720689,30.9476742201263,0.861348434042974));
#34400=CARTESIAN_POINT('',(9.049999720689,30.8671084399344,0.482316238758625));
#34401=CARTESIAN_POINT('',(9.049999720689,30.8671084399344,0.482316238758625));
#34402=CARTESIAN_POINT('',(9.049999720689,31.0282400003182,1.24038062932732));
#34403=CARTESIAN_POINT('',(9.049999720689,31.0282400003182,1.24038062932732));
#34404=CARTESIAN_POINT('',(8.153905970689,31.0282400003182,1.24038062932732));
#34405=CARTESIAN_POINT('',(7.887499720689,31.0282400003182,1.24038062932732));
#34406=CARTESIAN_POINT('',(8.739999720689,31.2054847167403,2.07425145895289));
#34407=CARTESIAN_POINT('',(8.739999720689,31.2054847167403,2.07425145895289));
#34408=CARTESIAN_POINT('',(7.887499720689,31.0836289742001,1.50096526358531));
#34409=CARTESIAN_POINT('',(7.499999720689,31.0282400003182,1.24038062932732));
#34410=CARTESIAN_POINT('',(7.887499720689,31.2699373408939,2.37747721518037));
#34411=CARTESIAN_POINT('',(7.887499720689,31.2699373408939,2.37747721518037));
#34412=CARTESIAN_POINT('',(7.112499720689,31.2699373408939,2.37747721518037));
#34413=CARTESIAN_POINT('',(7.112499720689,31.2699373408939,2.37747721518037));
#34414=CARTESIAN_POINT('',(7.112499720689,31.0836289742001,1.50096526358531));
#34415=CARTESIAN_POINT('',(7.112499720689,31.0282400003182,1.24038062932732));
#34416=CARTESIAN_POINT('',(6.259999720689,31.2054847167403,2.07425145895289));
#34417=CARTESIAN_POINT('Origin',(5.949999720689,28.5195541981733,0.981304296721248));
#34418=CARTESIAN_POINT('',(5.949999720689,28.5195541981733,0.981304296721248));
#34419=CARTESIAN_POINT('',(5.949999720689,28.6806857585571,1.73936868728995));
#34420=CARTESIAN_POINT('Origin',(7.112499720689,28.5195541981733,0.981304296721249));
#34421=CARTESIAN_POINT('',(6.846093470689,28.5195541981733,0.981304296721249));
#34422=CARTESIAN_POINT('Origin',(6.259999720689,28.3423094817512,0.14743346709568));
#34423=CARTESIAN_POINT('',(6.259999720689,28.3423094817512,0.14743346709568));
#34424=CARTESIAN_POINT('Origin',(7.499999720689,28.5195541981733,0.981304296721249));
#34425=CARTESIAN_POINT('',(7.112499720689,28.4641652242914,0.720719662463258));
#34426=CARTESIAN_POINT('Origin',(7.112499720689,28.2778568575977,-0.1557922891318));
#34427=CARTESIAN_POINT('',(7.112499720689,28.2778568575977,-0.1557922891318));
#34428=CARTESIAN_POINT('Origin',(7.887499720689,28.2778568575977,-0.1557922891318));
#34429=CARTESIAN_POINT('',(7.887499720689,28.2778568575977,-0.1557922891318));
#34430=CARTESIAN_POINT('Origin',(7.887499720689,28.5195541981733,0.981304296721249));
#34431=CARTESIAN_POINT('',(7.887499720689,28.4641652242914,0.720719662463259));
#34432=CARTESIAN_POINT('Origin',(8.739999720689,28.3423094817512,0.14743346709568));
#34433=CARTESIAN_POINT('',(8.739999720689,28.3423094817512,0.14743346709568));
#34434=CARTESIAN_POINT('Origin',(7.887499720689,28.6001199783652,1.3603364920056));
#34435=CARTESIAN_POINT('',(8.153905970689,28.5195541981733,0.981304296721249));
#34436=CARTESIAN_POINT('Origin',(9.049999720689,28.5195541981733,0.981304296721249));
#34437=CARTESIAN_POINT('',(9.049999720689,28.5195541981733,0.981304296721249));
#34438=CARTESIAN_POINT('Origin',(9.049999720689,28.6806857585571,1.73936868728995));
#34439=CARTESIAN_POINT('',(9.049999720689,28.6806857585571,1.73936868728995));
#34440=CARTESIAN_POINT('Origin',(7.887499720689,28.6806857585571,1.73936868728995));
#34441=CARTESIAN_POINT('',(8.153905970689,28.6806857585571,1.73936868728995));
#34442=CARTESIAN_POINT('Origin',(8.739999720689,28.8579304749792,2.57323951691552));
#34443=CARTESIAN_POINT('',(8.739999720689,28.8579304749792,2.57323951691552));
#34444=CARTESIAN_POINT('Origin',(7.499999720689,28.6806857585571,1.73936868728995));
#34445=CARTESIAN_POINT('',(7.887499720689,28.736074732439,1.99995332154794));
#34446=CARTESIAN_POINT('Origin',(7.887499720689,28.9223830991327,2.876465273143));
#34447=CARTESIAN_POINT('',(7.887499720689,28.9223830991327,2.876465273143));
#34448=CARTESIAN_POINT('Origin',(7.112499720689,28.9223830991327,2.876465273143));
#34449=CARTESIAN_POINT('',(7.112499720689,28.9223830991327,2.876465273143));
#34450=CARTESIAN_POINT('Origin',(7.112499720689,28.6806857585571,1.73936868728995));
#34451=CARTESIAN_POINT('',(7.112499720689,28.736074732439,1.99995332154794));
#34452=CARTESIAN_POINT('Origin',(6.259999720689,28.8579304749792,2.57323951691552));
#34453=CARTESIAN_POINT('',(6.259999720689,28.8579304749792,2.57323951691552));
#34454=CARTESIAN_POINT('Origin',(7.112499720689,28.6001199783652,1.3603364920056));
#34455=CARTESIAN_POINT('',(6.846093470689,28.6806857585571,1.73936868728995));
#34456=CARTESIAN_POINT('Origin',(5.949999720689,28.6806857585571,1.73936868728995));
#34457=CARTESIAN_POINT('Origin',(4.499999720689,32.0655571923935,0.6237350731084));
#34458=CARTESIAN_POINT('Origin',(4.499999720689,32.0655571923935,0.6237350731084));
#34459=CARTESIAN_POINT('Origin',(0.,34.510926194228,0.103955846064));
#34460=CARTESIAN_POINT('Origin',(5.19584375524573E-13,34.5109261942278,
0.103955846063327));
#34461=CARTESIAN_POINT('Origin',(0.,35.4890737949618,-0.10395584475376));
#34462=CARTESIAN_POINT('Origin',(2.55351295663786E-13,35.4890737949617,
-0.103955844754159));
#34463=CARTESIAN_POINT('Origin',(0.,34.510926194228,0.103955846064));
#34464=CARTESIAN_POINT('Origin',(1.32155929348462E-13,34.5109261942281,
0.103955846064179));
#34465=CARTESIAN_POINT('Ctrl Pts',(0.,32.3703984326954,-14.7761698557608));
#34466=CARTESIAN_POINT('Ctrl Pts',(0.,31.1966213118148,-14.5266758267795));
#34467=CARTESIAN_POINT('Ctrl Pts',(-29.,32.3703984326954,-14.7761698557608));
#34468=CARTESIAN_POINT('Ctrl Pts',(-29.,31.1966213118148,-14.5266758267795));
#34469=CARTESIAN_POINT('Ctrl Pts',(-29.,38.6077491572282,14.5682581662533));
#34470=CARTESIAN_POINT('Ctrl Pts',(-29.,37.4339720363476,14.8177521952346));
#34471=CARTESIAN_POINT('Ctrl Pts',(-1.77573785876366E-15,38.6077491572282,
14.5682581662533));
#34472=CARTESIAN_POINT('Ctrl Pts',(-1.77573785876366E-15,37.4339720363476,
14.8177521952346));
#34473=CARTESIAN_POINT('Origin',(1.88970922978163E-13,35.4890737949618,
-0.103955844753516));
#34474=CARTESIAN_POINT('Origin',(0.,35.4890737949618,-0.10395584475376));
#34475=CARTESIAN_POINT('',(0.,0.,0.));
#34476=CARTESIAN_POINT('Origin',(46.,34.999999994595,6.55002914876687E-10));
#34477=CARTESIAN_POINT('',(35.,38.8160931995804,8.90421747895505));
#34478=CARTESIAN_POINT('',(35.,42.2216398951714,6.45721096177453));
#34479=CARTESIAN_POINT('Origin',(35.,34.999999994595,6.55002914876687E-10));
#34480=CARTESIAN_POINT('',(35.,38.2526765117554,9.12511653277189));
#34481=CARTESIAN_POINT('Origin',(35.,34.999999994595,6.55002914876687E-10));
#34482=CARTESIAN_POINT('',(35.,27.7783600940186,-6.45721096046452));
#34483=CARTESIAN_POINT('Origin',(35.,34.999999994595,6.55002914876687E-10));
#34484=CARTESIAN_POINT('',(46.,27.7783600940186,-6.45721096046452));
#34485=CARTESIAN_POINT('',(46.,27.7783600940186,-6.45721096046452));
#34486=CARTESIAN_POINT('',(46.,42.2216398951714,6.45721096177453));
#34487=CARTESIAN_POINT('Origin',(46.,34.999999994595,6.55002914876687E-10));
#34488=CARTESIAN_POINT('',(46.,42.2216398951714,6.45721096177453));
#34489=CARTESIAN_POINT('Origin',(49.1839401118236,21.0000000000002,6.00000000000001));
#34490=CARTESIAN_POINT('',(33.,20.1857688098371,4.10012722295268));
#34491=CARTESIAN_POINT('Origin',(33.,21.0000000000002,6.00000000000001));
#34492=CARTESIAN_POINT('',(35.,20.1857688098371,4.10012722295268));
#34493=CARTESIAN_POINT('',(49.1839401118236,20.1857688098371,4.10012722295268));
#34494=CARTESIAN_POINT('Origin',(35.,21.0000000000002,6.00000000000001));
#34495=CARTESIAN_POINT('Origin',(33.,21.0000000000003,5.99999999999997));
#34496=CARTESIAN_POINT('',(28.,25.9586702584788,5.3584477669892));
#34497=CARTESIAN_POINT('',(28.,24.8843448987174,2.85168859421269));
#34498=CARTESIAN_POINT('Origin',(28.,21.0000000000003,5.99999999999997));
#34499=CARTESIAN_POINT('',(33.,25.9586702584788,5.3584477669892));
#34500=CARTESIAN_POINT('',(33.,25.9586702584788,5.3584477669892));
#34501=CARTESIAN_POINT('',(33.,24.8843448987174,2.85168859421269));
#34502=CARTESIAN_POINT('Origin',(33.,21.0000000000003,5.99999999999997));
#34503=CARTESIAN_POINT('',(33.,24.8843448987174,2.85168859421269));
#34504=CARTESIAN_POINT('Origin',(33.,35.0000000000003,1.87377939199425E-14));
#34505=CARTESIAN_POINT('',(28.,26.2716828895476,2.19464813110885));
#34506=CARTESIAN_POINT('',(28.,27.3912430012989,4.80695505852859));
#34507=CARTESIAN_POINT('Origin',(28.,35.0000000000003,1.87377939199425E-14));
#34508=CARTESIAN_POINT('',(33.,26.2716828895476,2.19464813110885));
#34509=CARTESIAN_POINT('',(33.,26.2716828895476,2.19464813110885));
#34510=CARTESIAN_POINT('',(33.,27.3912430012989,4.80695505852859));
#34511=CARTESIAN_POINT('Origin',(33.,35.0000000000003,1.87377939199425E-14));
#34512=CARTESIAN_POINT('',(33.,27.3912430012989,4.80695505852859));
#34513=CARTESIAN_POINT('Origin',(35.,36.2005438522226,0.262677966498032));
#34514=CARTESIAN_POINT('',(28.,39.4857043089188,8.64168272683559));
#34515=CARTESIAN_POINT('',(28.,44.4728491223851,-3.28259572071447));
#34516=CARTESIAN_POINT('Origin',(28.,36.2005438522226,0.262677966498032));
#34517=CARTESIAN_POINT('',(35.,39.4857043089188,8.64168272683559));
#34518=CARTESIAN_POINT('',(35.,39.4857043089188,8.64168272683559));
#34519=CARTESIAN_POINT('',(35.,44.3549070848781,4.07139957222298));
#34520=CARTESIAN_POINT('Origin',(35.,36.2005438522226,0.262677966498032));
#34521=CARTESIAN_POINT('',(35.,44.4728491223851,-3.28259572071447));
#34522=CARTESIAN_POINT('Origin',(35.,36.2005438522226,0.262677966498032));
#34523=CARTESIAN_POINT('',(35.,44.4728491223851,-3.28259572071447));
#34524=CARTESIAN_POINT('Origin',(36.5,49.8743530018414,-19.3357042103691));
#34525=CARTESIAN_POINT('',(36.5,44.5419465307234,-13.3720273892479));
#34526=CARTESIAN_POINT('',(36.,44.5419465307234,-13.3720273892479));
#34527=CARTESIAN_POINT('',(36.5,44.5419465307234,-13.3720273892479));
#34528=CARTESIAN_POINT('',(36.,49.8743530018414,-19.3357042103691));
#34529=CARTESIAN_POINT('',(36.,49.8743530018414,-19.3357042103691));
#34530=CARTESIAN_POINT('',(36.5,49.8743530018414,-19.3357042103691));
#34531=CARTESIAN_POINT('',(36.5,49.8743530018414,-19.3357042103691));
#34532=CARTESIAN_POINT('',(36.5,49.8743530018414,-19.3357042103691));
#34533=CARTESIAN_POINT('Origin',(36.5,50.0979908826335,-19.1357389677022));
#34534=CARTESIAN_POINT('',(36.5,44.7655844115154,-13.172062146581));
#34535=CARTESIAN_POINT('',(36.5,44.7655844115154,-13.172062146581));
#34536=CARTESIAN_POINT('',(36.5,50.0979908826335,-19.1357389677022));
#34537=CARTESIAN_POINT('',(36.5,50.0979908826335,-19.1357389677022));
#34538=CARTESIAN_POINT('',(36.5,50.0979908826335,-19.1357389677022));
#34539=CARTESIAN_POINT('Origin',(36.,50.0979908826335,-19.1357389677022));
#34540=CARTESIAN_POINT('',(36.,44.7655844115154,-13.172062146581));
#34541=CARTESIAN_POINT('',(36.,44.7655844115154,-13.172062146581));
#34542=CARTESIAN_POINT('',(36.,50.0979908826335,-19.1357389677022));
#34543=CARTESIAN_POINT('',(36.,50.0979908826335,-19.1357389677022));
#34544=CARTESIAN_POINT('',(36.,50.0979908826335,-19.1357389677022));
#34545=CARTESIAN_POINT('Origin',(28.,51.2161802865937,-18.1359127543675));
#34546=CARTESIAN_POINT('',(36.5,52.3343696905538,-17.1360865410329));
#34547=CARTESIAN_POINT('',(36.5,52.558007571346,-16.936121298366));
#34548=CARTESIAN_POINT('',(36.5,52.3343696905538,-17.1360865410329));
#34549=CARTESIAN_POINT('',(36.,52.3343696905538,-17.1360865410329));
#34550=CARTESIAN_POINT('',(36.,52.3343696905538,-17.1360865410329));
#34551=CARTESIAN_POINT('',(36.,52.558007571346,-16.936121298366));
#34552=CARTESIAN_POINT('',(36.,52.558007571346,-16.936121298366));
#34553=CARTESIAN_POINT('',(36.5,52.558007571346,-16.936121298366));
#34554=CARTESIAN_POINT('Origin',(36.,52.3343696905538,-17.1360865410329));
#34555=CARTESIAN_POINT('',(36.,47.0019632194358,-11.1724097199117));
#34556=CARTESIAN_POINT('',(36.5,47.0019632194358,-11.1724097199117));
#34557=CARTESIAN_POINT('',(36.,47.0019632194358,-11.1724097199117));
#34558=CARTESIAN_POINT('',(36.,52.3343696905538,-17.1360865410329));
#34559=CARTESIAN_POINT('',(36.5,52.3343696905538,-17.1360865410329));
#34560=CARTESIAN_POINT('Origin',(36.5,52.558007571346,-16.936121298366));
#34561=CARTESIAN_POINT('',(36.5,47.2256011002279,-10.9724444772448));
#34562=CARTESIAN_POINT('',(36.,47.2256011002279,-10.9724444772448));
#34563=CARTESIAN_POINT('',(36.5,47.2256011002279,-10.9724444772448));
#34564=CARTESIAN_POINT('',(36.5,52.558007571346,-16.936121298366));
#34565=CARTESIAN_POINT('',(36.,52.558007571346,-16.936121298366));
#34566=CARTESIAN_POINT('Origin',(28.,33.1363509879946,-1.66637702156941));
#34567=CARTESIAN_POINT('',(48.8,48.0194296622137,-18.3113705713116));
#34568=CARTESIAN_POINT('',(48.5,48.0194296622137,-18.3113705713116));
#34569=CARTESIAN_POINT('',(48.8,48.0194296622137,-18.3113705713116));
#34570=CARTESIAN_POINT('',(48.5,49.3656354031611,-19.8169452151862));
#34571=CARTESIAN_POINT('',(48.5,33.1363509879946,-1.66637702156941));
#34572=CARTESIAN_POINT('',(48.8,49.6858066844382,-20.175019577912));
#34573=CARTESIAN_POINT('',(48.,48.8320166010328,-19.2201546106433));
#34574=CARTESIAN_POINT('',(48.8,49.6858066844382,-20.175019577912));
#34575=CARTESIAN_POINT('Origin',(48.,48.0194296622137,-18.3113705713116));
#34576=CARTESIAN_POINT('',(48.,49.2047464023529,-18.8868792061983));
#34577=CARTESIAN_POINT('',(48.,52.1865848129134,-16.2206759706393));
#34578=CARTESIAN_POINT('',(48.,48.8320166010328,-19.2201546106433));
#34579=CARTESIAN_POINT('',(48.,48.3921594635339,-17.9780951668667));
#34580=CARTESIAN_POINT('',(48.,48.3921594635339,-17.9780951668667));
#34581=CARTESIAN_POINT('',(48.,51.3739978740944,-15.3118919313077));
#34582=CARTESIAN_POINT('',(48.,48.0194296622137,-18.3113705713116));
#34583=CARTESIAN_POINT('',(48.,52.1865848129134,-16.2206759706393));
#34584=CARTESIAN_POINT('Origin',(48.,48.8320166010328,-19.2201546106433));
#34585=CARTESIAN_POINT('',(39.9575325128956,46.6168572862855,-3.92682792990623));
#34586=CARTESIAN_POINT('',(48.5,53.0929334163619,-16.4841911707374));
#34587=CARTESIAN_POINT('',(47.57228567029,51.4112682420982,-15.9952575162825));
#34588=CARTESIAN_POINT('',(48.8,53.4131046976389,-16.8422655334632));
#34589=CARTESIAN_POINT('',(48.,52.5593146142335,-15.8874005661944));
#34590=CARTESIAN_POINT('',(48.8,49.6858066844382,-20.175019577912));
#34591=CARTESIAN_POINT('Origin',(28.,49.8830786688142,-16.6449935490872));
#34592=CARTESIAN_POINT('',(48.5,48.0194296622137,-18.3113705713116));
#34593=CARTESIAN_POINT('',(49.8,48.0194296622137,-18.3113705713116));
#34594=CARTESIAN_POINT('',(49.8,48.0194296622137,-18.3113705713116));
#34595=CARTESIAN_POINT('',(49.8,51.7467276754146,-14.9786165268629));
#34596=CARTESIAN_POINT('',(49.8,51.7467276754146,-14.9786165268629));
#34597=CARTESIAN_POINT('',(48.8,51.7467276754146,-14.9786165268629));
#34598=CARTESIAN_POINT('',(48.8,51.7467276754146,-14.9786165268629));
#34599=CARTESIAN_POINT('',(48.5,51.7467276754146,-14.9786165268629));
#34600=CARTESIAN_POINT('',(48.8,51.7467276754146,-14.9786165268629));
#34601=CARTESIAN_POINT('',(48.,51.3739978740944,-15.3118919313077));
#34602=CARTESIAN_POINT('Origin',(48.8,51.7467276754146,-14.9786165268629));
#34603=CARTESIAN_POINT('',(48.8,47.747422822076,-10.505858911022));
#34604=CARTESIAN_POINT('',(49.8,47.747422822076,-10.505858911022));
#34605=CARTESIAN_POINT('',(48.8,47.747422822076,-10.505858911022));
#34606=CARTESIAN_POINT('',(48.8,51.7467276754146,-14.9786165268629));
#34607=CARTESIAN_POINT('',(49.8,51.7467276754146,-14.9786165268629));
#34608=CARTESIAN_POINT('Origin',(49.8,48.0194296622137,-18.3113705713116));
#34609=CARTESIAN_POINT('',(49.8,44.0201248088753,-13.8386129554708));
#34610=CARTESIAN_POINT('',(48.8,44.0201248088753,-13.8386129554708));
#34611=CARTESIAN_POINT('',(49.8,44.0201248088753,-13.8386129554708));
#34612=CARTESIAN_POINT('',(49.8,48.0194296622137,-18.3113705713116));
#34613=CARTESIAN_POINT('',(48.8,48.0194296622137,-18.3113705713116));
#34614=CARTESIAN_POINT('Origin',(48.8,61.4283911851505,-9.67541749392847));
#34615=CARTESIAN_POINT('',(49.8,48.1486287370291,-21.5494833323853));
#34616=CARTESIAN_POINT('',(48.8,46.8574548302663,-22.7039831992086));
#34617=CARTESIAN_POINT('Origin',(47.8,48.1486287370291,-21.5494833323853));
#34618=CARTESIAN_POINT('',(48.8,48.5676172804779,-21.1748457912466));
#34619=CARTESIAN_POINT('',(48.8,61.4283911851505,-9.67541749392847));
#34620=CARTESIAN_POINT('',(48.8,61.4283911851505,-9.67541749392847));
#34621=CARTESIAN_POINT('',(48.8,54.5312941015992,-15.8424393201286));
#34622=CARTESIAN_POINT('',(48.8,61.4283911851505,-9.67541749392847));
#34623=CARTESIAN_POINT('',(48.8,56.2414565518108,-14.3133019121667));
#34624=CARTESIAN_POINT('',(48.8,61.4283911851505,-9.67541749392847));
#34625=CARTESIAN_POINT('',(49.8,54.950282645048,-15.4678017789899));
#34626=CARTESIAN_POINT('Origin',(47.8,54.950282645048,-15.4678017789899));
#34627=CARTESIAN_POINT('',(49.8,61.4283911851505,-9.67541749392847));
#34628=CARTESIAN_POINT('Origin',(46.,65.7609714429338,-14.5209049110894));
#34629=CARTESIAN_POINT('',(48.2499021086877,47.5471157171578,-23.8003792172667));
#34630=CARTESIAN_POINT('',(46.,50.6412872520117,-28.0401320991545));
#34631=CARTESIAN_POINT('',(45.1007678884438,51.8779536794353,-29.7346600173847));
#34632=CARTESIAN_POINT('',(46.,52.3038298561492,-26.5535738555194));
#34633=CARTESIAN_POINT('',(46.,65.7609714429338,-14.5209049110894));
#34634=CARTESIAN_POINT('',(48.,49.2091296720183,-23.0925114146902));
#34635=CARTESIAN_POINT('',(51.3562786983429,44.0157915191397,-17.2843663427951));
#34636=CARTESIAN_POINT('Origin',(47.9999999999999,49.8054973541307,-22.5592707675784));
#34637=CARTESIAN_POINT('Origin',(47.800000000136,49.6959788286485,-23.2800145527791));
#34638=CARTESIAN_POINT('Origin',(46.,53.1054137160521,-5.71502497212683));
#34639=CARTESIAN_POINT('',(42.,39.2212286168793,-18.1295337876985));
#34640=CARTESIAN_POINT('',(40.5,39.2212286168793,-18.1295337876985));
#34641=CARTESIAN_POINT('',(42.,39.2212286168793,-18.1295337876985));
#34642=CARTESIAN_POINT('',(40.5,39.6964591135624,-17.7046076470313));
#34643=CARTESIAN_POINT('',(40.5,38.9509995109222,-18.3711584559211));
#34644=CARTESIAN_POINT('',(46.,40.6430251186653,-16.8582380595522));
#34645=CARTESIAN_POINT('',(40.5,39.6964591135624,-17.7046076470313));
#34646=CARTESIAN_POINT('',(46.,38.6621339148992,-18.6294468943659));
#34647=CARTESIAN_POINT('',(46.,53.1054137160521,-5.71502497212683));
#34648=CARTESIAN_POINT('',(42.,38.6621339148992,-18.6294468943659));
#34649=CARTESIAN_POINT('',(46.,38.6621339148992,-18.6294468943659));
#34650=CARTESIAN_POINT('',(42.,39.2212286168793,-18.1295337876985));
#34651=CARTESIAN_POINT('Origin',(40.35,49.3810785931525,-22.4596728974293));
#34652=CARTESIAN_POINT('',(40.35,49.5609187050531,-20.8604902883506));
#34653=CARTESIAN_POINT('',(40.35,43.6101220274232,-14.2052159003601));
#34654=CARTESIAN_POINT('',(40.35,50.2756301163208,-21.6598119267616));
#34655=CARTESIAN_POINT('',(40.35,49.9029003150007,-21.9930873312064));
#34656=CARTESIAN_POINT('',(40.35,49.9029003150006,-21.9930873312065));
#34657=CARTESIAN_POINT('',(40.35,49.7538083944726,-22.1263974929844));
#34658=CARTESIAN_POINT('',(40.35,49.3810785931525,-22.4596728974293));
#34659=CARTESIAN_POINT('',(40.35,48.6663671818848,-21.6603512590183));
#34660=CARTESIAN_POINT('',(40.35,49.7538083944726,-22.1263974929844));
#34661=CARTESIAN_POINT('',(40.35,42.7155705042549,-15.0050768710278));
#34662=CARTESIAN_POINT('',(40.35,49.3810785931525,-22.4596728974293));
#34663=CARTESIAN_POINT('',(40.35,42.7155705042549,-15.0050768710278));
#34664=CARTESIAN_POINT('Origin',(40.65,49.3810785931525,-22.4596728974293));
#34665=CARTESIAN_POINT('',(40.65,48.6663671818848,-21.6603512590183));
#34666=CARTESIAN_POINT('',(40.65,48.6663671818848,-21.6603512590183));
#34667=CARTESIAN_POINT('',(40.65,42.7155705042549,-15.0050768710278));
#34668=CARTESIAN_POINT('',(40.65,49.3810785931525,-22.4596728974293));
#34669=CARTESIAN_POINT('',(40.65,42.7155705042549,-15.0050768710278));
#34670=CARTESIAN_POINT('Origin',(40.65,54.8229336924257,-17.5938519925341));
#34671=CARTESIAN_POINT('',(40.35,54.1082222811579,-16.794530354123));
#34672=CARTESIAN_POINT('',(40.35,48.1574256035281,-10.1392559661326));
#34673=CARTESIAN_POINT('',(40.35,54.8229336924257,-17.5938519925341));
#34674=CARTESIAN_POINT('',(40.65,54.1082222811579,-16.794530354123));
#34675=CARTESIAN_POINT('',(40.65,54.1082222811579,-16.794530354123));
#34676=CARTESIAN_POINT('',(40.65,48.1574256035281,-10.1392559661326));
#34677=CARTESIAN_POINT('',(40.65,54.8229336924257,-17.5938519925341));
#34678=CARTESIAN_POINT('',(40.65,48.1574256035281,-10.1392559661326));
#34679=CARTESIAN_POINT('Origin',(40.65,55.7174852155938,-16.7939910218664));
#34680=CARTESIAN_POINT('',(40.65,55.3447554142738,-17.1272664263113));
#34681=CARTESIAN_POINT('',(40.65,55.1956634937457,-17.2605765880892));
#34682=CARTESIAN_POINT('',(40.65,55.7174852155938,-16.7939910218664));
#34683=CARTESIAN_POINT('',(40.65,55.0027738043262,-15.9946693834553));
#34684=CARTESIAN_POINT('',(40.65,55.3447554142738,-17.1272664263113));
#34685=CARTESIAN_POINT('',(40.65,49.0519771266963,-9.33939499546487));
#34686=CARTESIAN_POINT('',(40.65,55.7174852155938,-16.7939910218664));
#34687=CARTESIAN_POINT('',(40.65,49.0519771266963,-9.33939499546487));
#34688=CARTESIAN_POINT('',(40.65,55.1956634937457,-17.2605765880892));
#34689=CARTESIAN_POINT('Origin',(28.,49.7538083944727,-22.1263974929844));
#34690=CARTESIAN_POINT('',(40.65,49.7538083944726,-22.1263974929844));
#34691=CARTESIAN_POINT('',(40.65,49.7538083944726,-22.1263974929844));
#34692=CARTESIAN_POINT('',(40.35,49.7538083944726,-22.1263974929844));
#34693=CARTESIAN_POINT('Origin',(28.,49.9029003150007,-21.9930873312064));
#34694=CARTESIAN_POINT('',(40.65,49.5609187050531,-20.8604902883506));
#34695=CARTESIAN_POINT('',(40.35,49.5609187050531,-20.8604902883506));
#34696=CARTESIAN_POINT('',(40.65,49.9029003150007,-21.9930873312064));
#34697=CARTESIAN_POINT('',(40.65,49.9029003150006,-21.9930873312065));
#34698=CARTESIAN_POINT('',(40.65,49.9029003150007,-21.9930873312064));
#34699=CARTESIAN_POINT('Origin',(28.,52.5492819043732,-19.6268319596478));
#34700=CARTESIAN_POINT('',(40.65,50.2756301163208,-21.6598119267616));
#34701=CARTESIAN_POINT('Origin',(28.,55.1956634937457,-17.2605765880892));
#34702=CARTESIAN_POINT('',(40.35,55.1956634937457,-17.2605765880892));
#34703=CARTESIAN_POINT('',(40.35,55.1956634937457,-17.2605765880892));
#34704=CARTESIAN_POINT('',(40.35,55.1956634937457,-17.2605765880892));
#34705=CARTESIAN_POINT('Origin',(28.,55.3447554142738,-17.1272664263113));
#34706=CARTESIAN_POINT('',(40.35,55.0027738043262,-15.9946693834553));
#34707=CARTESIAN_POINT('',(40.35,55.3447554142738,-17.1272664263113));
#34708=CARTESIAN_POINT('',(40.35,55.3447554142738,-17.1272664263113));
#34709=CARTESIAN_POINT('',(40.35,55.0027738043262,-15.9946693834553));
#34710=CARTESIAN_POINT('',(40.65,55.3447554142738,-17.1272664263113));
#34711=CARTESIAN_POINT('Origin',(28.,51.2161802865937,-18.1359127543675));
#34712=CARTESIAN_POINT('',(36.,49.8743530018414,-19.3357042103691));
#34713=CARTESIAN_POINT('Origin',(38.5,58.3261827962024,-18.886372642664));
#34714=CARTESIAN_POINT('',(35.7,59.4602420414948,-20.1546860901778));
#34715=CARTESIAN_POINT('',(36.,58.3261827962024,-18.886372642664));
#34716=CARTESIAN_POINT('',(35.7,59.4602420414948,-20.1546860901778));
#34717=CARTESIAN_POINT('',(38.5,61.5475289288871,-18.2883438252864));
#34718=CARTESIAN_POINT('Origin',(38.5,59.4602420414948,-20.1546860901778));
#34719=CARTESIAN_POINT('',(38.5,60.1898318028027,-17.2199956204396));
#34720=CARTESIAN_POINT('',(38.5,60.1898318028027,-17.2199956204396));
#34721=CARTESIAN_POINT('Origin',(38.5,58.3261827962024,-18.886372642664));
#34722=CARTESIAN_POINT('Origin',(42.5,60.1898318028026,-17.2199956204395));
#34723=CARTESIAN_POINT('',(42.5,61.5475289288871,-18.2883438252864));
#34724=CARTESIAN_POINT('',(38.5,61.5475289288871,-18.2883438252864));
#34725=CARTESIAN_POINT('',(42.5,60.1898318028026,-17.2199956204395));
#34726=CARTESIAN_POINT('',(42.5,60.1898318028026,-17.2199956204395));
#34727=CARTESIAN_POINT('',(42.5,60.1898318028026,-17.2199956204395));
#34728=CARTESIAN_POINT('Origin',(36.,58.3261827962024,-18.886372642664));
#34729=CARTESIAN_POINT('',(36.,51.1697706108569,-25.2852604080056));
#34730=CARTESIAN_POINT('',(36.,58.3261827962024,-18.886372642664));
#34731=CARTESIAN_POINT('',(35.7,52.3038298561492,-26.5535738555194));
#34732=CARTESIAN_POINT('',(35.7,52.3038298561492,-26.5535738555194));
#34733=CARTESIAN_POINT('',(35.7,59.4602420414948,-20.1546860901778));
#34734=CARTESIAN_POINT('Origin',(42.5,58.3261827962024,-18.886372642664));
#34735=CARTESIAN_POINT('',(45.3,59.4602420414948,-20.1546860901778));
#34736=CARTESIAN_POINT('Origin',(42.5,59.4602420414948,-20.1546860901778));
#34737=CARTESIAN_POINT('',(45.,58.3261827962023,-18.886372642664));
#34738=CARTESIAN_POINT('',(45.,58.3261827962023,-18.886372642664));
#34739=CARTESIAN_POINT('Origin',(42.5,58.3261827962024,-18.886372642664));
#34740=CARTESIAN_POINT('Origin',(38.5,51.1697706108569,-25.2852604080056));
#34741=CARTESIAN_POINT('',(38.5,49.3061216042565,-26.95163743023));
#34742=CARTESIAN_POINT('Origin',(38.5,51.1697706108569,-25.2852604080056));
#34743=CARTESIAN_POINT('',(38.5,50.2165429687568,-28.4199161204107));
#34744=CARTESIAN_POINT('',(38.5,50.2165429687568,-28.4199161204107));
#34745=CARTESIAN_POINT('Origin',(38.5,52.3038298561492,-26.5535738555194));
#34746=CARTESIAN_POINT('Origin',(45.,58.3261827962023,-18.886372642664));
#34747=CARTESIAN_POINT('',(45.3,52.3038298561492,-26.5535738555194));
#34748=CARTESIAN_POINT('',(45.3,59.4602420414947,-20.1546860901777));
#34749=CARTESIAN_POINT('',(45.,51.1697706108569,-25.2852604080056));
#34750=CARTESIAN_POINT('',(45.,51.1697706108569,-25.2852604080056));
#34751=CARTESIAN_POINT('',(45.,58.3261827962023,-18.886372642664));
#34752=CARTESIAN_POINT('Origin',(42.5,49.3061216042565,-26.9516374302301));
#34753=CARTESIAN_POINT('',(42.5,49.3061216042565,-26.9516374302301));
#34754=CARTESIAN_POINT('',(42.5,49.3061216042565,-26.9516374302301));
#34755=CARTESIAN_POINT('',(42.5,50.2165429687568,-28.4199161204107));
#34756=CARTESIAN_POINT('',(42.5,50.2165429687568,-28.4199161204107));
#34757=CARTESIAN_POINT('',(38.5,50.2165429687568,-28.4199161204107));
#34758=CARTESIAN_POINT('Origin',(40.35,55.7174852155938,-16.7939910218664));
#34759=CARTESIAN_POINT('',(40.35,49.0519771266963,-9.33939499546487));
#34760=CARTESIAN_POINT('',(40.35,55.7174852155938,-16.7939910218664));
#34761=CARTESIAN_POINT('',(40.35,49.0519771266963,-9.33939499546487));
#34762=CARTESIAN_POINT('Origin',(42.5,51.1697706108569,-25.2852604080056));
#34763=CARTESIAN_POINT('Origin',(42.5,52.3038298561492,-26.5535738555194));
#34764=CARTESIAN_POINT('Origin',(42.5,51.1697706108569,-25.2852604080056));
#34765=CARTESIAN_POINT('Origin',(36.5,52.3343696905538,-17.1360865410329));
#34766=CARTESIAN_POINT('',(36.5,47.0019632194358,-11.1724097199117));
#34767=CARTESIAN_POINT('Origin',(28.,36.8636490011954,1.66637702287939));
#34768=CARTESIAN_POINT('',(48.5,51.7467276754146,-14.9786165268629));
#34769=CARTESIAN_POINT('',(48.8,53.4131046976389,-16.8422655334632));
#34770=CARTESIAN_POINT('Origin',(48.,51.3739978740944,-15.3118919313077));
#34771=CARTESIAN_POINT('Origin',(48.5,33.1363509879946,-1.66637702156941));
#34772=CARTESIAN_POINT('Origin',(35.,26.4453341955376,13.754426956311));
#34773=CARTESIAN_POINT('',(28.,26.4453341955376,13.754426956311));
#34774=CARTESIAN_POINT('',(28.,26.4453341955376,13.754426956311));
#34775=CARTESIAN_POINT('',(35.,26.4453341955376,13.754426956311));
#34776=CARTESIAN_POINT('',(35.,26.4453341955376,13.754426956311));
#34777=CARTESIAN_POINT('',(35.,26.4453341955376,13.754426956311));
#34778=CARTESIAN_POINT('',(35.,26.4453341955376,13.754426956311));
#34779=CARTESIAN_POINT('',(35.,26.4453341955376,13.754426956311));
#34780=CARTESIAN_POINT('Origin',(35.,43.9100514671661,-4.59579024955887));
#34781=CARTESIAN_POINT('',(28.,43.9100514671661,-4.59579024955887));
#34782=CARTESIAN_POINT('',(28.,43.9100514671661,-4.59579024955887));
#34783=CARTESIAN_POINT('',(35.,43.9100514671661,-4.59579024955887));
#34784=CARTESIAN_POINT('',(35.,43.9100514671661,-4.59579024955887));
#34785=CARTESIAN_POINT('',(35.,43.9100514671661,-4.59579024955887));
#34786=CARTESIAN_POINT('Origin',(35.,35.6377461970035,-1.05051656234637));
#34787=CARTESIAN_POINT('',(28.,31.8358189268944,-9.20804983122126));
#34788=CARTESIAN_POINT('Origin',(28.,35.6377461970035,-1.05051656234637));
#34789=CARTESIAN_POINT('',(35.,31.8358189268944,-9.20804983122126));
#34790=CARTESIAN_POINT('Origin',(35.,35.6377461970035,-1.05051656234637));
#34791=CARTESIAN_POINT('',(35.,31.8358189268944,-9.20804983122126));
#34792=CARTESIAN_POINT('Origin',(35.,19.14012819977,-3.29105370048002));
#34793=CARTESIAN_POINT('',(28.,19.14012819977,-3.29105370048002));
#34794=CARTESIAN_POINT('',(28.,19.14012819977,-3.29105370048002));
#34795=CARTESIAN_POINT('',(35.,29.0964332376969,-7.93132256431019));
#34796=CARTESIAN_POINT('',(35.,19.14012819977,-3.29105370048002));
#34797=CARTESIAN_POINT('',(35.,19.14012819977,-3.29105370048002));
#34798=CARTESIAN_POINT('',(35.,19.14012819977,-3.29105370048002));
#34799=CARTESIAN_POINT('',(35.,19.14012819977,-3.29105370048002));
#34800=CARTESIAN_POINT('Origin',(35.,22.9420554698791,4.86647956839487));
#34801=CARTESIAN_POINT('',(28.,14.6697501997166,8.41175325560737));
#34802=CARTESIAN_POINT('Origin',(28.,22.9420554698791,4.86647956839487));
#34803=CARTESIAN_POINT('',(35.,14.6697501997166,8.41175325560737));
#34804=CARTESIAN_POINT('Origin',(35.,22.9420554698791,4.86647956839487));
#34805=CARTESIAN_POINT('',(35.,14.6697501997166,8.41175325560737));
#34806=CARTESIAN_POINT('Origin',(35.,23.1601737388414,5.37542219597347));
#34807=CARTESIAN_POINT('',(28.,14.8878684686789,8.92069588318597));
#34808=CARTESIAN_POINT('Origin',(28.,23.1601737388414,5.37542219597347));
#34809=CARTESIAN_POINT('',(35.,14.8878684686789,8.92069588318597));
#34810=CARTESIAN_POINT('',(35.,14.8878684686789,8.92069588318597));
#34811=CARTESIAN_POINT('Origin',(35.,23.1601737388414,5.37542219597347));
#34812=CARTESIAN_POINT('Origin',(35.,14.8878684686789,8.92069588318597));
#34813=CARTESIAN_POINT('',(28.,14.8878684686789,8.92069588318597));
#34814=CARTESIAN_POINT('',(35.,14.8878684686789,8.92069588318597));
#34815=CARTESIAN_POINT('Origin',(33.,25.7867763834114,2.31657302728156));
#34816=CARTESIAN_POINT('',(28.,25.9837360327009,2.77614554229058));
#34817=CARTESIAN_POINT('Origin',(28.,25.7867763834114,2.31657302728156));
#34818=CARTESIAN_POINT('',(33.,25.9837360327009,2.77614554229058));
#34819=CARTESIAN_POINT('',(33.,25.9837360327009,2.77614554229058));
#34820=CARTESIAN_POINT('Origin',(33.,25.7867763834114,2.31657302728156));
#34821=CARTESIAN_POINT('Origin',(33.,26.9685342791489,5.07400811733573));
#34822=CARTESIAN_POINT('',(28.,26.7715746298593,4.6144356023267));
#34823=CARTESIAN_POINT('Origin',(28.,26.9685342791489,5.07400811733573));
#34824=CARTESIAN_POINT('',(33.,26.7715746298593,4.6144356023267));
#34825=CARTESIAN_POINT('Origin',(33.,26.9685342791489,5.07400811733573));
#34826=CARTESIAN_POINT('',(33.,26.7715746298593,4.6144356023267));
#34827=CARTESIAN_POINT('Origin',(33.,26.257577635037,4.83472002867911));
#34828=CARTESIAN_POINT('',(28.,26.257577635037,4.83472002867911));
#34829=CARTESIAN_POINT('',(28.,26.257577635037,4.83472002867911));
#34830=CARTESIAN_POINT('',(33.,26.257577635037,4.83472002867911));
#34831=CARTESIAN_POINT('',(33.,26.257577635037,4.83472002867911));
#34832=CARTESIAN_POINT('',(33.,26.257577635037,4.83472002867911));
#34833=CARTESIAN_POINT('Origin',(33.,26.4545372843266,5.29429254368814));
#34834=CARTESIAN_POINT('Origin',(28.,26.4545372843266,5.29429254368814));
#34835=CARTESIAN_POINT('Origin',(33.,26.4545372843266,5.29429254368814));
#34836=CARTESIAN_POINT('Origin',(33.,25.2727793885891,2.53685745363396));
#34837=CARTESIAN_POINT('',(28.,25.4697390378787,2.99642996864299));
#34838=CARTESIAN_POINT('Origin',(28.,25.2727793885891,2.53685745363396));
#34839=CARTESIAN_POINT('',(33.,25.4697390378787,2.99642996864299));
#34840=CARTESIAN_POINT('Origin',(33.,25.2727793885891,2.53685745363396));
#34841=CARTESIAN_POINT('',(33.,25.4697390378787,2.99642996864299));
#34842=CARTESIAN_POINT('Origin',(35.,23.1601737388414,5.37542219597347));
#34843=CARTESIAN_POINT('',(35.,42.2216398951714,6.45721096177453));
#34844=CARTESIAN_POINT('Origin',(28.,23.1601737388414,5.37542219597347));
#34845=CARTESIAN_POINT('',(28.,25.4697390378787,2.99642996864299));
#34846=CARTESIAN_POINT('Origin',(33.,25.7867763834114,2.31657302728156));
#34847=CARTESIAN_POINT('',(33.,25.4697390378787,2.99642996864299));
#34848=CARTESIAN_POINT('Origin',(33.,25.4697390378787,2.99642996864299));
#34849=CARTESIAN_POINT('Origin',(46.,53.1054137160521,-5.71502497212683));
#34850=CARTESIAN_POINT('',(35.,42.3055677228029,-15.3716798159172));
#34851=CARTESIAN_POINT('',(35.,39.2212286168793,-18.1295337876985));
#34852=CARTESIAN_POINT('',(35.,53.1054137160521,-5.71502497212683));
#34853=CARTESIAN_POINT('',(38.5,39.6964591135624,-17.7046076470313));
#34854=CARTESIAN_POINT('Origin',(38.5,42.3055677228029,-15.3716798159172));
#34855=CARTESIAN_POINT('',(39.7,39.6964591135624,-17.7046076470313));
#34856=CARTESIAN_POINT('',(39.7,39.6964591135624,-17.7046076470313));
#34857=CARTESIAN_POINT('',(39.7,39.2212286168793,-18.1295337876985));
#34858=CARTESIAN_POINT('',(39.7,38.9509995109222,-18.3711584559211));
#34859=CARTESIAN_POINT('',(42.,39.2212286168793,-18.1295337876985));
#34860=CARTESIAN_POINT('Origin',(35.,23.1601737388414,5.37542219597347));
#34861=CARTESIAN_POINT('',(35.,27.7783600940186,-6.45721096046452));
#34862=CARTESIAN_POINT('Origin',(46.,42.2216398951714,6.45721096177453));
#34863=CARTESIAN_POINT('',(42.,49.7726596716033,-1.98772695892608));
#34864=CARTESIAN_POINT('',(42.,53.1054137160521,-5.71502497212683));
#34865=CARTESIAN_POINT('',(42.,49.7726596716033,-1.98772695892608));
#34866=CARTESIAN_POINT('',(41.,49.1061088627135,-1.24226735628591));
#34867=CARTESIAN_POINT('',(41.,49.1061088627135,-1.24226735628591));
#34868=CARTESIAN_POINT('',(35.,49.1061088627135,-1.24226735628591));
#34869=CARTESIAN_POINT('',(35.,49.1061088627135,-1.24226735628591));
#34870=CARTESIAN_POINT('',(35.,42.2216398951714,6.45721096177453));
#34871=CARTESIAN_POINT('',(46.,53.1054137160521,-5.71502497212683));
#34872=CARTESIAN_POINT('',(46.,42.2216398951714,6.45721096177453));
#34873=CARTESIAN_POINT('',(46.,53.1054137160521,-5.71502497212683));
#34874=CARTESIAN_POINT('Origin',(35.,34.999999994595,6.55002914876687E-10));
#34875=CARTESIAN_POINT('Origin',(46.,53.1054137160521,-5.71502497212683));
#34876=CARTESIAN_POINT('',(46.,51.124522512286,-7.4862338069405));
#34877=CARTESIAN_POINT('',(40.5,52.0710885173889,-6.63986421946138));
#34878=CARTESIAN_POINT('',(40.5,52.0710885173889,-6.63986421946138));
#34879=CARTESIAN_POINT('',(40.5,52.5463190140719,-6.21493807879413));
#34880=CARTESIAN_POINT('',(40.5,52.0710885173889,-6.63986421946138));
#34881=CARTESIAN_POINT('',(42.,52.5463190140719,-6.21493807879413));
#34882=CARTESIAN_POINT('',(42.,52.5463190140719,-6.21493807879413));
#34883=CARTESIAN_POINT('',(42.,52.5463190140719,-6.21493807879413));
#34884=CARTESIAN_POINT('',(46.,53.1054137160521,-5.71502497212683));
#34885=CARTESIAN_POINT('Origin',(46.,27.7783600940186,-6.45721096046452));
#34886=CARTESIAN_POINT('',(41.,34.6628290615606,-14.156689278525));
#34887=CARTESIAN_POINT('',(42.,35.3293798704504,-14.9021488811651));
#34888=CARTESIAN_POINT('',(41.,34.6628290615606,-14.156689278525));
#34889=CARTESIAN_POINT('',(42.,35.3293798704504,-14.9021488811651));
#34890=CARTESIAN_POINT('',(46.,27.7783600940186,-6.45721096046452));
#34891=CARTESIAN_POINT('',(35.,34.6628290615606,-14.156689278525));
#34892=CARTESIAN_POINT('',(35.,27.7783600940186,-6.45721096046452));
#34893=CARTESIAN_POINT('',(35.,34.6628290615606,-14.156689278525));
#34894=CARTESIAN_POINT('Origin',(35.,34.999999994595,6.55002914876687E-10));
#34895=CARTESIAN_POINT('',(35.,48.5470141607334,-1.74218046295324));
#34896=CARTESIAN_POINT('',(35.,48.5470141607334,-1.74218046295324));
#34897=CARTESIAN_POINT('',(35.,52.5463190140719,-6.21493807879413));
#34898=CARTESIAN_POINT('',(35.,52.5463190140719,-6.21493807879413));
#34899=CARTESIAN_POINT('',(35.,49.4619799081484,-8.97279205057551));
#34900=CARTESIAN_POINT('',(35.,53.1054137160521,-5.71502497212683));
#34901=CARTESIAN_POINT('',(35.,59.4602420414948,-20.1546860901778));
#34902=CARTESIAN_POINT('',(35.,59.4602420414948,-20.1546860901778));
#34903=CARTESIAN_POINT('',(35.,52.3038298561492,-26.5535738555194));
#34904=CARTESIAN_POINT('',(35.,52.3038298561492,-26.5535738555194));
#34905=CARTESIAN_POINT('',(35.,52.3038298561492,-26.5535738555194));
#34906=CARTESIAN_POINT('',(35.,35.2219237635407,-13.6567761718577));
#34907=CARTESIAN_POINT('',(35.,39.2212286168793,-18.1295337876985));
#34908=CARTESIAN_POINT('',(35.,35.2219237635407,-13.6567761718577));
#34909=CARTESIAN_POINT('Origin',(46.,34.999999994595,6.55002914876687E-10));
#34910=CARTESIAN_POINT('',(46.,42.3055677228029,-15.3716798159172));
#34911=CARTESIAN_POINT('',(46.,53.1054137160521,-5.71502497212683));
#34912=CARTESIAN_POINT('',(46.,49.4619799081483,-8.97279205057553));
#34913=CARTESIAN_POINT('',(46.,53.1054137160521,-5.71502497212683));
#34914=CARTESIAN_POINT('',(46.,53.1054137160521,-5.71502497212683));
#34915=CARTESIAN_POINT('Origin',(41.,35.2219237635407,-13.6567761718577));
#34916=CARTESIAN_POINT('',(41.,35.2219237635407,-13.6567761718577));
#34917=CARTESIAN_POINT('',(41.,35.2219237635407,-13.6567761718577));
#34918=CARTESIAN_POINT('',(42.,35.8884745724305,-14.4022357744978));
#34919=CARTESIAN_POINT('',(41.,35.2219237635407,-13.6567761718577));
#34920=CARTESIAN_POINT('',(42.,35.8884745724305,-14.4022357744978));
#34921=CARTESIAN_POINT('Origin',(42.,35.8884745724305,-14.4022357744978));
#34922=CARTESIAN_POINT('',(42.,35.8884745724305,-14.4022357744978));
#34923=CARTESIAN_POINT('Origin',(35.,35.2219237635407,-13.6567761718577));
#34924=CARTESIAN_POINT('',(35.,35.2219237635407,-13.6567761718577));
#34925=CARTESIAN_POINT('Origin',(28.,28.3374547959987,-5.9572978537972));
#34926=CARTESIAN_POINT('',(42.,39.2212286168793,-18.1295337876985));
#34927=CARTESIAN_POINT('Origin',(41.,48.5470141607334,-1.74218046295324));
#34928=CARTESIAN_POINT('',(42.,49.2135649696232,-2.48764006559341));
#34929=CARTESIAN_POINT('',(42.,49.2135649696232,-2.48764006559341));
#34930=CARTESIAN_POINT('',(41.,48.5470141607334,-1.74218046295324));
#34931=CARTESIAN_POINT('',(41.,48.5470141607334,-1.74218046295324));
#34932=CARTESIAN_POINT('',(41.,48.5470141607334,-1.74218046295324));
#34933=CARTESIAN_POINT('Origin',(42.,49.2135649696232,-2.48764006559341));
#34934=CARTESIAN_POINT('',(42.,49.2135649696232,-2.48764006559341));
#34935=CARTESIAN_POINT('Origin',(35.,48.5470141607334,-1.74218046295324));
#34936=CARTESIAN_POINT('',(35.,48.5470141607334,-1.74218046295324));
#34937=CARTESIAN_POINT('Origin',(28.,41.6625451931913,5.95729785510721));
#34938=CARTESIAN_POINT('',(39.7,52.5463190140719,-6.21493807879413));
#34939=CARTESIAN_POINT('',(42.,52.5463190140719,-6.21493807879413));
#34940=CARTESIAN_POINT('',(42.,52.5463190140719,-6.21493807879413));
#34941=CARTESIAN_POINT('Origin',(40.5,62.0693506507352,-17.8217582590636));
#34942=CARTESIAN_POINT('',(40.5,62.0693506507352,-17.8217582590636));
#34943=CARTESIAN_POINT('',(40.5,62.0693506507352,-17.8217582590636));
#34944=CARTESIAN_POINT('',(40.5,62.8148102533754,-17.1552074501738));
#34945=CARTESIAN_POINT('',(40.5,62.0693506507352,-17.8217582590636));
#34946=CARTESIAN_POINT('',(40.5,52.8165481200291,-5.97331341057162));
#34947=CARTESIAN_POINT('',(40.5,62.8148102533754,-17.1552074501738));
#34948=CARTESIAN_POINT('',(40.5,52.0710885173889,-6.63986421946138));
#34949=CARTESIAN_POINT('Origin',(40.5,62.8148102533754,-17.1552074501738));
#34950=CARTESIAN_POINT('',(39.7,52.8165481200291,-5.97331341057162));
#34951=CARTESIAN_POINT('',(40.5,52.8165481200291,-5.97331341057162));
#34952=CARTESIAN_POINT('',(39.7,62.8148102533754,-17.1552074501738));
#34953=CARTESIAN_POINT('',(40.5,62.8148102533754,-17.1552074501738));
#34954=CARTESIAN_POINT('',(39.7,62.8148102533754,-17.1552074501738));
#34955=CARTESIAN_POINT('Origin',(39.7,62.8148102533754,-17.1552074501738));
#34956=CARTESIAN_POINT('',(39.7,52.8165481200291,-5.97331341057162));
#34957=CARTESIAN_POINT('',(39.7,62.0693506507352,-17.8217582590636));
#34958=CARTESIAN_POINT('',(39.7,62.8148102533754,-17.1552074501738));
#34959=CARTESIAN_POINT('',(39.7,52.0710885173889,-6.63986421946138));
#34960=CARTESIAN_POINT('',(39.7,62.0693506507352,-17.8217582590636));
#34961=CARTESIAN_POINT('',(39.7,52.8165481200291,-5.97331341057162));
#34962=CARTESIAN_POINT('Origin',(38.5,62.0693506507352,-17.8217582590636));
#34963=CARTESIAN_POINT('',(38.5,52.0710885173889,-6.63986421946138));
#34964=CARTESIAN_POINT('',(38.5,52.0710885173889,-6.63986421946138));
#34965=CARTESIAN_POINT('',(38.5,62.0693506507352,-17.8217582590636));
#34966=CARTESIAN_POINT('',(38.5,62.0693506507352,-17.8217582590636));
#34967=CARTESIAN_POINT('',(38.5,62.0693506507352,-17.8217582590636));
#34968=CARTESIAN_POINT('Origin',(38.5,59.4602420414948,-20.1546860901778));
#34969=CARTESIAN_POINT('Origin',(38.5,49.4619799081484,-8.97279205057551));
#34970=CARTESIAN_POINT('Origin',(38.5,59.4602420414948,-20.1546860901778));
#34971=CARTESIAN_POINT('Origin',(38.5,52.3038298561492,-26.5535738555194));
#34972=CARTESIAN_POINT('',(38.5,49.6947212469087,-28.8865016866336));
#34973=CARTESIAN_POINT('Origin',(38.5,52.3038298561492,-26.5535738555194));
#34974=CARTESIAN_POINT('',(38.5,49.6947212469087,-28.8865016866336));
#34975=CARTESIAN_POINT('Origin',(39.7,49.6947212469087,-28.8865016866336));
#34976=CARTESIAN_POINT('',(39.7,49.6947212469087,-28.8865016866336));
#34977=CARTESIAN_POINT('',(39.7,49.6947212469087,-28.8865016866336));
#34978=CARTESIAN_POINT('',(39.7,49.6947212469087,-28.8865016866336));
#34979=CARTESIAN_POINT('Origin',(39.7,48.9492616442685,-29.5530524955233));
#34980=CARTESIAN_POINT('',(39.7,48.9492616442685,-29.5530524955233));
#34981=CARTESIAN_POINT('',(39.7,48.9492616442685,-29.5530524955233));
#34982=CARTESIAN_POINT('',(39.7,38.9509995109222,-18.3711584559211));
#34983=CARTESIAN_POINT('',(39.7,48.9492616442685,-29.5530524955233));
#34984=CARTESIAN_POINT('',(39.7,38.9509995109222,-18.3711584559211));
#34985=CARTESIAN_POINT('Origin',(40.5,48.9492616442685,-29.5530524955233));
#34986=CARTESIAN_POINT('',(40.5,38.9509995109222,-18.3711584559211));
#34987=CARTESIAN_POINT('',(40.5,38.9509995109222,-18.3711584559211));
#34988=CARTESIAN_POINT('',(40.5,48.9492616442685,-29.5530524955233));
#34989=CARTESIAN_POINT('',(40.5,48.9492616442685,-29.5530524955233));
#34990=CARTESIAN_POINT('',(40.5,48.9492616442685,-29.5530524955233));
#34991=CARTESIAN_POINT('Origin',(40.5,48.9492616442685,-29.5530524955233));
#34992=CARTESIAN_POINT('',(40.5,38.9509995109222,-18.3711584559211));
#34993=CARTESIAN_POINT('',(40.5,49.6947212469087,-28.8865016866336));
#34994=CARTESIAN_POINT('',(40.5,48.9492616442685,-29.5530524955233));
#34995=CARTESIAN_POINT('',(40.5,49.6947212469087,-28.8865016866336));
#34996=CARTESIAN_POINT('Origin',(40.5,49.6947212469087,-28.8865016866336));
#34997=CARTESIAN_POINT('',(48.2499021086877,41.0302398188277,-16.5120110196252));
#34998=CARTESIAN_POINT('',(48.2499021086877,51.028501952174,-27.6939050592275));
#34999=CARTESIAN_POINT('',(40.5,39.6964591135624,-17.7046076470313));
#35000=CARTESIAN_POINT('',(40.5,49.6947212469087,-28.8865016866336));
#35001=CARTESIAN_POINT('Origin',(38.5,49.4619799081484,-8.97279205057551));
#35002=CARTESIAN_POINT('',(48.8,48.8656122260362,-9.50603269768731));
#35003=CARTESIAN_POINT('',(48.8,42.901935404915,-14.8384391688054));
#35004=CARTESIAN_POINT('',(49.8,49.284600769485,-9.13139515654859));
#35005=CARTESIAN_POINT('',(49.8,42.4829468614662,-15.213076709944));
#35006=CARTESIAN_POINT('',(48.2499021086877,50.7373078121236,-7.83246084686749));
#35007=CARTESIAN_POINT('Origin',(47.8,49.284600769485,-9.13139515654859));
#35008=CARTESIAN_POINT('',(40.5,52.0710885173889,-6.63986421946138));
#35009=CARTESIAN_POINT('',(48.,49.4619799081484,-8.97279205057552));
#35010=CARTESIAN_POINT('',(45.4,49.4619799081483,-8.97279205057553));
#35011=CARTESIAN_POINT('Origin',(48.,48.8656122260362,-9.50603269768731));
#35012=CARTESIAN_POINT('Origin',(47.8,52.4812089948126,-26.3949707495463));
#35013=CARTESIAN_POINT('',(49.8,42.4829468614662,-15.213076709944));
#35014=CARTESIAN_POINT('',(49.8,52.4812089948126,-26.3949707495463));
#35015=CARTESIAN_POINT('Origin',(47.8,42.4829468614662,-15.213076709944));
#35016=CARTESIAN_POINT('Origin',(47.8,59.2828629028313,-20.3132891961508));
#35017=CARTESIAN_POINT('',(48.2499021086877,57.2541837104536,-15.1208290445089));
#35018=CARTESIAN_POINT('Origin',(47.7999999998822,56.4976327370815,-17.198332999803));
#35019=CARTESIAN_POINT('',(48.2499021086877,60.7355699454699,-19.0143548864697));
#35020=CARTESIAN_POINT('',(49.8,59.2828629028313,-20.3132891961508));
#35021=CARTESIAN_POINT('Origin',(38.5,49.4619799081484,-8.97279205057551));
#35022=CARTESIAN_POINT('Origin',(38.5,49.4619799081484,-8.97279205057551));
#35023=CARTESIAN_POINT('',(49.8,42.4829468614662,-15.213076709944));
#35024=CARTESIAN_POINT('',(48.8,42.901935404915,-14.8384391688054));
#35025=CARTESIAN_POINT('',(48.8,42.901935404915,-14.8384391688054));
#35026=CARTESIAN_POINT('',(48.,42.3055677228029,-15.3716798159172));
#35027=CARTESIAN_POINT('Origin',(48.,42.901935404915,-14.8384391688054));
#35028=CARTESIAN_POINT('',(45.4,42.3055677228029,-15.3716798159172));
#35029=CARTESIAN_POINT('Origin',(40.5,62.0693506507352,-17.8217582590636));
#35030=CARTESIAN_POINT('',(46.,61.1227846456323,-18.6681278465427));
#35031=CARTESIAN_POINT('',(45.1007678884438,62.6689719994181,-20.0858984152072));
#35032=CARTESIAN_POINT('',(40.5,62.0693506507352,-17.8217582590636));
#35033=CARTESIAN_POINT('Origin',(38.5,59.4602420414948,-20.1546860901778));
#35034=CARTESIAN_POINT('',(46.,59.4602420414948,-20.1546860901778));
#35035=CARTESIAN_POINT('',(46.,65.7609714429338,-14.5209049110894));
#35036=CARTESIAN_POINT('',(45.4,59.4602420414948,-20.1546860901778));
#35037=CARTESIAN_POINT('',(45.4,59.4602420414948,-20.1546860901778));
#35038=CARTESIAN_POINT('',(45.4,52.3038298561492,-26.5535738555194));
#35039=CARTESIAN_POINT('',(45.4,59.4602420414948,-20.1546860901778));
#35040=CARTESIAN_POINT('',(45.4,52.3038298561492,-26.5535738555194));
#35041=CARTESIAN_POINT('Origin',(49.8,52.4812089948126,-26.3949707495463));
#35042=CARTESIAN_POINT('Origin',(46.,53.1054137160521,-5.71502497212683));
#35043=CARTESIAN_POINT('Origin',(48.8,42.901935404915,-14.8384391688054));
#35044=CARTESIAN_POINT('',(48.8,48.8656122260362,-9.50603269768731));
#35045=CARTESIAN_POINT('Origin',(48.,48.8656122260362,-9.50603269768731));
#35046=CARTESIAN_POINT('',(48.,56.3655418573637,-16.6936236493485));
#35047=CARTESIAN_POINT('',(48.,49.4619799081484,-8.97279205057552));
#35048=CARTESIAN_POINT('Origin',(48.0000000000003,55.7691741752514,-17.2268642964596));
#35049=CARTESIAN_POINT('Origin',(48.,42.901935404915,-14.8384391688054));
#35050=CARTESIAN_POINT('',(48.8,42.901935404915,-14.8384391688054));
#35051=CARTESIAN_POINT('',(48.,42.3055677228029,-15.3716798159172));
#35052=CARTESIAN_POINT('Origin',(45.4,42.3055677228029,-15.3716798159172));
#35053=CARTESIAN_POINT('',(45.4,42.3055677228029,-15.3716798159172));
#35054=CARTESIAN_POINT('',(45.4,42.3055677228029,-15.3716798159172));
#35055=CARTESIAN_POINT('',(45.4,42.3055677228029,-15.3716798159172));
#35056=CARTESIAN_POINT('Origin',(38.5,49.4619799081484,-8.97279205057551));
#35057=CARTESIAN_POINT('Origin',(45.4,49.4619799081483,-8.97279205057553));
#35058=CARTESIAN_POINT('',(51.3562786983429,51.1722037044851,-10.8854785774534));
#35059=CARTESIAN_POINT('',(45.4,49.4619799081483,-8.97279205057553));
#35060=CARTESIAN_POINT('',(45.4,49.4619799081483,-8.97279205057553));
#35061=CARTESIAN_POINT('',(45.4,49.4619799081483,-8.97279205057553));
#35062=CARTESIAN_POINT('Origin',(48.,48.8656122260362,-9.50603269768731));
#35063=CARTESIAN_POINT('',(45.4,49.4619799081483,-8.97279205057553));
#35064=CARTESIAN_POINT('Origin',(45.4,49.4619799081483,-8.97279205057553));
#35065=CARTESIAN_POINT('Origin',(42.5,51.3256289147487,-7.3064150283511));
#35066=CARTESIAN_POINT('',(38.5,51.3256289147488,-7.30641502835113));
#35067=CARTESIAN_POINT('',(38.5,51.3256289147488,-7.30641502835113));
#35068=CARTESIAN_POINT('',(42.5,51.3256289147488,-7.30641502835114));
#35069=CARTESIAN_POINT('',(42.5,51.3256289147488,-7.30641502835114));
#35070=CARTESIAN_POINT('',(42.5,51.3256289147487,-7.3064150283511));
#35071=CARTESIAN_POINT('Origin',(42.5,49.4619799081484,-8.97279205057552));
#35072=CARTESIAN_POINT('',(45.,49.4619799081483,-8.97279205057549));
#35073=CARTESIAN_POINT('',(45.,49.4619799081483,-8.97279205057549));
#35074=CARTESIAN_POINT('Origin',(42.5,49.4619799081484,-8.97279205057552));
#35075=CARTESIAN_POINT('Origin',(45.,49.4619799081483,-8.97279205057549));
#35076=CARTESIAN_POINT('',(45.,42.3055677228029,-15.3716798159172));
#35077=CARTESIAN_POINT('',(45.,42.3055677228029,-15.3716798159172));
#35078=CARTESIAN_POINT('',(45.,49.4619799081483,-8.97279205057549));
#35079=CARTESIAN_POINT('Origin',(42.5,42.3055677228029,-15.3716798159172));
#35080=CARTESIAN_POINT('',(42.5,40.4419187162025,-17.0380568381416));
#35081=CARTESIAN_POINT('',(42.5,40.4419187162025,-17.0380568381416));
#35082=CARTESIAN_POINT('Origin',(42.5,42.3055677228029,-15.3716798159172));
#35083=CARTESIAN_POINT('Origin',(42.5,40.4419187162025,-17.0380568381416));
#35084=CARTESIAN_POINT('',(38.5,40.4419187162025,-17.0380568381416));
#35085=CARTESIAN_POINT('',(38.5,40.4419187162025,-17.0380568381416));
#35086=CARTESIAN_POINT('',(42.5,40.4419187162025,-17.0380568381416));
#35087=CARTESIAN_POINT('Origin',(38.5,42.3055677228029,-15.3716798159172));
#35088=CARTESIAN_POINT('',(36.,42.3055677228029,-15.3716798159172));
#35089=CARTESIAN_POINT('',(36.,42.3055677228029,-15.3716798159172));
#35090=CARTESIAN_POINT('Origin',(38.5,42.3055677228029,-15.3716798159172));
#35091=CARTESIAN_POINT('Origin',(38.5,49.4619799081484,-8.9727920505755));
#35092=CARTESIAN_POINT('',(36.,49.4619799081484,-8.97279205057551));
#35093=CARTESIAN_POINT('',(36.,49.4619799081484,-8.97279205057551));
#35094=CARTESIAN_POINT('Origin',(38.5,49.4619799081484,-8.9727920505755));
#35095=CARTESIAN_POINT('Origin',(46.,65.7609714429338,-14.5209049110894));
#35096=CARTESIAN_POINT('Origin',(48.8,42.901935404915,-14.8384391688054));
#35097=CARTESIAN_POINT('Origin',(36.,49.4619799081484,-8.97279205057551));
#35098=CARTESIAN_POINT('',(36.,49.4619799081484,-8.97279205057551));
#35099=CARTESIAN_POINT('',(36.,49.4619799081484,-8.97279205057551));
#35100=CARTESIAN_POINT('',(36.,49.4619799081484,-8.97279205057551));
#35101=CARTESIAN_POINT('Origin',(40.35,54.8229336924257,-17.5938519925341));
#35102=CARTESIAN_POINT('',(40.35,54.8229336924257,-17.5938519925341));
#35103=CARTESIAN_POINT('',(40.35,48.1574256035281,-10.1392559661326));
#35104=CARTESIAN_POINT('Origin',(28.,52.5492819043732,-19.6268319596478));
#35105=CARTESIAN_POINT('Origin',(40.65,52.1020061427891,-20.0267624449817));
#35106=CARTESIAN_POINT('',(40.35,51.3872947315215,-19.2274408065706));
#35107=CARTESIAN_POINT('',(40.35,45.4364980538915,-12.5721664185802));
#35108=CARTESIAN_POINT('',(40.35,52.1020061427891,-20.0267624449817));
#35109=CARTESIAN_POINT('',(40.65,51.3872947315215,-19.2274408065706));
#35110=CARTESIAN_POINT('',(40.65,51.3872947315215,-19.2274408065706));
#35111=CARTESIAN_POINT('',(40.65,45.4364980538915,-12.5721664185802));
#35112=CARTESIAN_POINT('',(40.65,52.1020061427891,-20.0267624449817));
#35113=CARTESIAN_POINT('',(40.65,45.4364980538915,-12.5721664185802));
#35114=CARTESIAN_POINT('Origin',(40.35,52.9965576659573,-19.2269014743139));
#35115=CARTESIAN_POINT('',(40.65,52.2818462546897,-18.4275798359029));
#35116=CARTESIAN_POINT('',(40.65,46.3310495770598,-11.7723054479125));
#35117=CARTESIAN_POINT('',(40.65,52.9965576659573,-19.2269014743139));
#35118=CARTESIAN_POINT('',(40.35,52.2818462546897,-18.4275798359029));
#35119=CARTESIAN_POINT('',(40.35,52.2818462546897,-18.4275798359029));
#35120=CARTESIAN_POINT('',(40.35,46.3310495770598,-11.7723054479125));
#35121=CARTESIAN_POINT('',(40.35,52.9965576659573,-19.2269014743139));
#35122=CARTESIAN_POINT('',(40.35,46.3310495770598,-11.7723054479125));
#35123=CARTESIAN_POINT('Origin',(40.65,52.9965576659573,-19.2269014743139));
#35124=CARTESIAN_POINT('',(40.65,52.6238278646372,-19.5601768787589));
#35125=CARTESIAN_POINT('',(40.65,52.4747359441092,-19.6934870405368));
#35126=CARTESIAN_POINT('',(40.65,52.9965576659573,-19.2269014743139));
#35127=CARTESIAN_POINT('',(40.65,52.6238278646372,-19.5601768787589));
#35128=CARTESIAN_POINT('',(40.65,46.3310495770598,-11.7723054479125));
#35129=CARTESIAN_POINT('',(40.65,52.4747359441092,-19.6934870405368));
#35130=CARTESIAN_POINT('Origin',(28.,52.6238278646372,-19.5601768787589));
#35131=CARTESIAN_POINT('',(40.35,52.6238278646372,-19.5601768787589));
#35132=CARTESIAN_POINT('',(40.35,52.6238278646372,-19.5601768787589));
#35133=CARTESIAN_POINT('',(40.65,52.6238278646372,-19.5601768787589));
#35134=CARTESIAN_POINT('Origin',(28.,52.5492819043732,-19.6268319596478));
#35135=CARTESIAN_POINT('',(40.35,52.4747359441092,-19.6934870405368));
#35136=CARTESIAN_POINT('',(40.35,52.1020061427891,-20.0267624449817));
#35137=CARTESIAN_POINT('',(40.35,52.4747359441092,-19.6934870405368));
#35138=CARTESIAN_POINT('Origin',(40.35,52.1020061427891,-20.0267624449817));
#35139=CARTESIAN_POINT('',(40.35,52.4747359441092,-19.6934870405368));
#35140=CARTESIAN_POINT('',(40.35,45.4364980538915,-12.5721664185802));
#35141=CARTESIAN_POINT('Origin',(40.35,50.2756301163208,-21.6598119267616));
#35142=CARTESIAN_POINT('',(40.65,43.6101220274232,-14.2052159003601));
#35143=CARTESIAN_POINT('',(40.65,50.2756301163208,-21.6598119267616));
#35144=CARTESIAN_POINT('',(40.35,43.6101220274232,-14.2052159003601));
#35145=CARTESIAN_POINT('Origin',(40.65,50.2756301163208,-21.6598119267616));
#35146=CARTESIAN_POINT('',(40.65,43.6101220274232,-14.2052159003601));
#35147=CARTESIAN_POINT('Origin',(28.,52.4747359441092,-19.6934870405368));
#35148=CARTESIAN_POINT('Origin',(42.5,49.4619799081484,-8.97279205057552));
#35149=CARTESIAN_POINT('',(0.,0.,0.));
#35150=CARTESIAN_POINT('Origin',(-37.718924746634,35.,3.67381906146713E-15));
#35151=CARTESIAN_POINT('',(-37.718924746634,26.8011470173929,-0.137148713427167));
#35152=CARTESIAN_POINT('',(-37.718924746634,25.2013708256647,-0.163909437998321));
#35153=CARTESIAN_POINT('Origin',(-37.718924746634,26.0012589215288,-0.150529075712744));
#35154=CARTESIAN_POINT('Origin',(-37.718924746634,26.0012589215288,-0.150529075712744));
#35155=CARTESIAN_POINT('',(-37.718924746634,26.8,0.));
#35156=CARTESIAN_POINT('Origin',(-37.718924746634,35.,3.67381906146713E-15));
#35157=CARTESIAN_POINT('',(-36.918924746634,26.,0.));
#35158=CARTESIAN_POINT('Origin',(-37.718924746634,26.,0.));
#35159=CARTESIAN_POINT('',(-37.718924746634,25.2,0.));
#35160=CARTESIAN_POINT('Origin',(-37.718924746634,26.,0.));
#35161=CARTESIAN_POINT('',(-38.518924746634,26.,0.));
#35162=CARTESIAN_POINT('Origin',(-37.718924746634,26.,0.));
#35163=CARTESIAN_POINT('Origin',(-37.718924746634,26.,0.));
#35164=CARTESIAN_POINT('Origin',(-17.718924746634,35.,-1.7347234759768E-15));
#35165=CARTESIAN_POINT('',(-18.518924746634,26.,-2.20436423846523E-14));
#35166=CARTESIAN_POINT('',(-17.718924746634,26.8,-2.00842075060165E-14));
#35167=CARTESIAN_POINT('Origin',(-17.718924746634,26.,-2.20436423846523E-14));
#35168=CARTESIAN_POINT('',(-17.718924746634,25.2,-2.40030772632881E-14));
#35169=CARTESIAN_POINT('Origin',(-17.718924746634,26.,-2.20436423846523E-14));
#35170=CARTESIAN_POINT('',(-16.918924746634,26.,-2.20436423846523E-14));
#35171=CARTESIAN_POINT('Origin',(-17.718924746634,26.,-2.20436423846523E-14));
#35172=CARTESIAN_POINT('Origin',(-17.718924746634,26.,-2.20436423846523E-14));
#35173=CARTESIAN_POINT('',(-17.718924746634,26.8044789537624,0.270988524991688));
#35174=CARTESIAN_POINT('Origin',(-17.718924746634,35.,-1.7347234759768E-15));
#35175=CARTESIAN_POINT('',(-17.718924746634,25.20535289596,0.323864334746163));
#35176=CARTESIAN_POINT('Origin',(-17.718924746634,26.0049159248612,0.297426429868925));
#35177=CARTESIAN_POINT('Origin',(-17.718924746634,26.0049159248612,0.297426429868925));
#35178=CARTESIAN_POINT('Origin',(-37.718924746634,21.,-2.5));
#35179=CARTESIAN_POINT('',(-37.3733225893608,18.2550018077979,-2.93018347082097));
#35180=CARTESIAN_POINT('',(-37.718924746634,19.3314643670594,-4.62273145772317));
#35181=CARTESIAN_POINT('Ctrl Pts',(-37.3733232272543,18.2550018791746,-2.93018346215923));
#35182=CARTESIAN_POINT('Ctrl Pts',(-37.3725399318501,18.2873279411122,-3.13887925979283));
#35183=CARTESIAN_POINT('Ctrl Pts',(-37.3771862418788,18.3459461927511,-3.34221139809461));
#35184=CARTESIAN_POINT('Ctrl Pts',(-37.4055310344249,18.5636687830632,-3.84861224630963));
#35185=CARTESIAN_POINT('Ctrl Pts',(-37.4367046322635,18.7448722293728,-4.09334967078263));
#35186=CARTESIAN_POINT('Ctrl Pts',(-37.513662764176,19.0344707879862,-4.3965117730213));
#35187=CARTESIAN_POINT('Ctrl Pts',(-37.5503726296912,19.1412839689907,-4.48376923795396));
#35188=CARTESIAN_POINT('Ctrl Pts',(-37.6047598935936,19.2409031720841,-4.55916514358062));
#35189=CARTESIAN_POINT('Ctrl Pts',(-37.6248502188041,19.2739476093295,-4.58313159510348));
#35190=CARTESIAN_POINT('Ctrl Pts',(-37.6598548373438,19.3077811937435,-4.60665604839667));
#35191=CARTESIAN_POINT('Ctrl Pts',(-37.6713097435794,19.3168085985258,-4.61282433924523));
#35192=CARTESIAN_POINT('Ctrl Pts',(-37.6923292478912,19.327010715773,-4.61973825681333));
#35193=CARTESIAN_POINT('Ctrl Pts',(-37.7011201878655,19.3298589042222,-4.62165247607873));
#35194=CARTESIAN_POINT('Ctrl Pts',(-37.7132641086043,19.3312981704222,-4.62261984197903));
#35195=CARTESIAN_POINT('Ctrl Pts',(-37.7161029581537,19.3314643670594,-4.62273145772315));
#35196=CARTESIAN_POINT('Ctrl Pts',(-37.718924746634,19.3314643670594,-4.62273145772315));
#35197=CARTESIAN_POINT('',(-36.9189423546079,17.5305480470118,-3.0004786401109));
#35198=CARTESIAN_POINT('Ctrl Pts',(-37.3733226583846,18.2550016652924,-2.93018349180643));
#35199=CARTESIAN_POINT('Ctrl Pts',(-37.3516251004149,18.2446527637436,-2.9312734297924));
#35200=CARTESIAN_POINT('Ctrl Pts',(-37.3303369685924,18.2333021834777,-2.93246489517018));
#35201=CARTESIAN_POINT('Ctrl Pts',(-37.3038079847852,18.2175624224805,-2.93410932586751));
#35202=CARTESIAN_POINT('Ctrl Pts',(-37.2981695486083,18.2141223505386,-2.93446831448551));
#35203=CARTESIAN_POINT('Ctrl Pts',(-37.2869979825889,18.2071152324757,-2.93519862167771));
#35204=CARTESIAN_POINT('Ctrl Pts',(-37.2704052709352,18.1964200031032,-2.93631197089007));
#35205=CARTESIAN_POINT('Ctrl Pts',(-37.2328335594255,18.1701812873708,-2.93903307929234));
#35206=CARTESIAN_POINT('Ctrl Pts',(-37.1823616251368,18.1291072193081,-2.94325912074197));
#35207=CARTESIAN_POINT('Ctrl Pts',(-37.1453575126505,18.0924641596172,-2.94698385382838));
#35208=CARTESIAN_POINT('Ctrl Pts',(-37.1188904285929,18.063538924587,-2.94990359739459));
#35209=CARTESIAN_POINT('Ctrl Pts',(-37.1102827811923,18.053656262645,-2.95089791608696));
#35210=CARTESIAN_POINT('Ctrl Pts',(-37.097699635775,18.0384638148773,-2.95242101316685));
#35211=CARTESIAN_POINT('Ctrl Pts',(-37.0935544678788,18.0333310247829,-2.95293470286882));
#35212=CARTESIAN_POINT('Ctrl Pts',(-37.0854130228059,18.0229903050876,-2.95396774156509));
#35213=CARTESIAN_POINT('Ctrl Pts',(-37.0654228154996,17.996938824735,-2.95656569797625));
#35214=CARTESIAN_POINT('Ctrl Pts',(-37.032653758298,17.9482802891913,-2.96137533348098));
#35215=CARTESIAN_POINT('Ctrl Pts',(-36.9956436062314,17.8797286255216,-2.96804918531509));
#35216=CARTESIAN_POINT('Ctrl Pts',(-36.9754354386431,17.8315716900848,-2.97266366864207));
#35217=CARTESIAN_POINT('Ctrl Pts',(-36.9642457335021,17.8006811814676,-2.97559869592517));
#35218=CARTESIAN_POINT('Ctrl Pts',(-36.9620775415684,17.7944555471112,-2.97618899559907));
#35219=CARTESIAN_POINT('Ctrl Pts',(-36.9579096024883,17.7819924669561,-2.97736824178165));
#35220=CARTESIAN_POINT('Ctrl Pts',(-36.9519025588888,17.763262156184,-2.97913679820747));
#35221=CARTESIAN_POINT('Ctrl Pts',(-36.9395867914297,17.7193101856959,-2.98326093492252));
#35222=CARTESIAN_POINT('Ctrl Pts',(-36.9267397851585,17.655829738656,-2.98914315755744));
#35223=CARTESIAN_POINT('Ctrl Pts',(-36.9198258320865,17.5885563906065,-2.99527260942571));
#35224=CARTESIAN_POINT('Ctrl Pts',(-36.918834284911,17.5465615159496,-2.99904690933985));
#35225=CARTESIAN_POINT('Ctrl Pts',(-36.9189421675989,17.5305480457708,-3.00047864028992));
#35226=CARTESIAN_POINT('',(-37.718924746634,16.7373849369936,-3.06578952415236));
#35227=CARTESIAN_POINT('Ctrl Pts',(-36.9189421675989,17.5305480457708,-3.00047864028992));
#35228=CARTESIAN_POINT('Ctrl Pts',(-36.919010575733,17.5203939456227,-3.0013864971935));
#35229=CARTESIAN_POINT('Ctrl Pts',(-36.9192737151562,17.5102114283485,-3.00229389904805));
#35230=CARTESIAN_POINT('Ctrl Pts',(-36.9209227121865,17.4736847569009,-3.00553816871275));
#35231=CARTESIAN_POINT('Ctrl Pts',(-36.9258858078666,17.4215585073783,-3.01012817483868));
#35232=CARTESIAN_POINT('Ctrl Pts',(-36.9408692628969,17.3448391155681,-3.01677274079049));
#35233=CARTESIAN_POINT('Ctrl Pts',(-36.9558799055065,17.2946725283372,-3.02104811851266));
#35234=CARTESIAN_POINT('Ctrl Pts',(-36.96687627967,17.2636336341393,-3.02367300382162));
#35235=CARTESIAN_POINT('Ctrl Pts',(-36.9691537112077,17.257450076958,-3.02419490147982));
#35236=CARTESIAN_POINT('Ctrl Pts',(-36.9738469995823,17.2451764290858,-3.02522882019687));
#35237=CARTESIAN_POINT('Ctrl Pts',(-36.9811011279822,17.2268856044673,-3.02676662512534));
#35238=CARTESIAN_POINT('Ctrl Pts',(-36.9995186272136,17.1850400421649,-3.03026458098281));
#35239=CARTESIAN_POINT('Ctrl Pts',(-37.0300126016223,17.1275979053621,-3.0350126340462));
#35240=CARTESIAN_POINT('Ctrl Pts',(-37.0588378628576,17.084120115963,-3.03855681973285));
#35241=CARTESIAN_POINT('Ctrl Pts',(-37.0782685093995,17.0577375107066,-3.04069395282585));
#35242=CARTESIAN_POINT('Ctrl Pts',(-37.082225544559,17.0525006314761,-3.04111747216896));
#35243=CARTESIAN_POINT('Ctrl Pts',(-37.0902828595418,17.0421069646206,-3.04195670011983));
#35244=CARTESIAN_POINT('Ctrl Pts',(-37.0943866683441,17.0369458657907,-3.04237275563911));
#35245=CARTESIAN_POINT('Ctrl Pts',(-37.1068915748229,17.0216125534472,-3.04360691231197));
#35246=CARTESIAN_POINT('Ctrl Pts',(-37.1325618428275,16.9916896358098,-3.04600756947841));
#35247=CARTESIAN_POINT('Ctrl Pts',(-37.1785652046567,16.9454439267093,-3.04968393967054));
#35248=CARTESIAN_POINT('Ctrl Pts',(-37.2187381548525,16.9122436653894,-3.05229515823886));
#35249=CARTESIAN_POINT('Ctrl Pts',(-37.2501443023646,16.8887815514432,-3.05413229054577));
#35250=CARTESIAN_POINT('Ctrl Pts',(-37.2661669984714,16.8774105933781,-3.05502048390176));
#35251=CARTESIAN_POINT('Ctrl Pts',(-37.2826770037829,16.8665887086542,-3.05586302629121));
#35252=CARTESIAN_POINT('Ctrl Pts',(-37.293793158217,16.8594974852881,-3.05641453576931));
#35253=CARTESIAN_POINT('Ctrl Pts',(-37.2994118352766,16.8560102252891,-3.05668545575409));
#35254=CARTESIAN_POINT('Ctrl Pts',(-37.3276328534854,16.8389747544918,-3.05800757335247));
#35255=CARTESIAN_POINT('Ctrl Pts',(-37.3737884152845,16.8141488770453,-3.0599257099477));
#35256=CARTESIAN_POINT('Ctrl Pts',(-37.4459381546772,16.7839866864414,-3.06224049280731));
#35257=CARTESIAN_POINT('Ctrl Pts',(-37.4959782855394,16.7685872041763,-3.06341603722978));
#35258=CARTESIAN_POINT('Ctrl Pts',(-37.5342560467992,16.7588521398196,-3.06415800376904));
#35259=CARTESIAN_POINT('Ctrl Pts',(-37.5471721285017,16.7559047648012,-3.06438240114302));
#35260=CARTESIAN_POINT('Ctrl Pts',(-37.5729991097878,16.7506789220564,-3.06478000194362));
#35261=CARTESIAN_POINT('Ctrl Pts',(-37.6117937694978,16.7438261426791,-3.06530089754843));
#35262=CARTESIAN_POINT('Ctrl Pts',(-37.6647357792095,16.7384443509895,-3.06570916417531));
#35263=CARTESIAN_POINT('Ctrl Pts',(-37.704858235669,16.737384873758,-3.06578952970039));
#35264=CARTESIAN_POINT('Ctrl Pts',(-37.718924746634,16.7373849369936,-3.06578952415236));
#35265=CARTESIAN_POINT('',(-38.5188998330781,17.5422403127815,-2.99943193326247));
#35266=CARTESIAN_POINT('Ctrl Pts',(-37.718924746634,16.7373849369936,-3.06578952415236));
#35267=CARTESIAN_POINT('Ctrl Pts',(-37.7309724146918,16.7373849911536,-3.06578951940059));
#35268=CARTESIAN_POINT('Ctrl Pts',(-37.7430350373672,16.7376571699563,-3.06576887237064));
#35269=CARTESIAN_POINT('Ctrl Pts',(-37.7682023355023,16.7387953147954,-3.06568253939694));
#35270=CARTESIAN_POINT('Ctrl Pts',(-37.7813096714479,16.7397096923924,-3.0656131746316));
#35271=CARTESIAN_POINT('Ctrl Pts',(-37.8009977508883,16.741573938698,-3.06547168652142));
#35272=CARTESIAN_POINT('Ctrl Pts',(-37.8075737093973,16.7422786005527,-3.06541819715752));
#35273=CARTESIAN_POINT('Ctrl Pts',(-37.8206887979692,16.7438483559608,-3.06529901151748));
#35274=CARTESIAN_POINT('Ctrl Pts',(-37.8533606292976,16.7481717229133,-3.06497067396001));
#35275=CARTESIAN_POINT('Ctrl Pts',(-37.9111453064512,16.7594812532432,-3.06411088374695));
#35276=CARTESIAN_POINT('Ctrl Pts',(-37.9860613887302,16.7818937437651,-3.06240058626652));
#35277=CARTESIAN_POINT('Ctrl Pts',(-38.0345821581833,16.8017347263525,-3.06087864877346));
#35278=CARTESIAN_POINT('Ctrl Pts',(-38.0644485553534,16.8157154672045,-3.05980221395205));
#35279=CARTESIAN_POINT('Ctrl Pts',(-38.0704043083084,16.8185937583215,-3.05958042082917));
#35280=CARTESIAN_POINT('Ctrl Pts',(-38.0822056520277,16.8244781459628,-3.05912657441623));
#35281=CARTESIAN_POINT('Ctrl Pts',(-38.099763863601,16.8335052848071,-3.05842974112173));
#35282=CARTESIAN_POINT('Ctrl Pts',(-38.1397327587973,16.8559635822866,-3.05669137072979));
#35283=CARTESIAN_POINT('Ctrl Pts',(-38.1940302112681,16.8919528132613,-3.05388941931908));
#35284=CARTESIAN_POINT('Ctrl Pts',(-38.2345117085067,16.9248663030074,-3.05130289362264));
#35285=CARTESIAN_POINT('Ctrl Pts',(-38.2637436106773,16.9511255701933,-3.04922757687767));
#35286=CARTESIAN_POINT('Ctrl Pts',(-38.2732990393399,16.9601414846898,-3.0485131908628));
#35287=CARTESIAN_POINT('Ctrl Pts',(-38.2873435899538,16.9740676197577,-3.04740650943474));
#35288=CARTESIAN_POINT('Ctrl Pts',(-38.2919756404014,16.9787758243361,-3.04703183290515));
#35289=CARTESIAN_POINT('Ctrl Pts',(-38.3010915965788,16.9882731695345,-3.04627492659788));
#35290=CARTESIAN_POINT('Ctrl Pts',(-38.3235426877027,17.012252520247,-3.04436110678424));
#35291=CARTESIAN_POINT('Ctrl Pts',(-38.3609567050234,17.0575033826528,-3.04072350743365));
#35292=CARTESIAN_POINT('Ctrl Pts',(-38.4045936810271,17.1221885322085,-3.03545633743746));
#35293=CARTESIAN_POINT('Ctrl Pts',(-38.429500116155,17.1682250232725,-3.03165548589758));
#35294=CARTESIAN_POINT('Ctrl Pts',(-38.4437134661759,17.1979395070246,-3.02918325758975));
#35295=CARTESIAN_POINT('Ctrl Pts',(-38.4464837427162,17.2039205266858,-3.02868471815221));
#35296=CARTESIAN_POINT('Ctrl Pts',(-38.4518595478943,17.2159127295726,-3.02768323259862));
#35297=CARTESIAN_POINT('Ctrl Pts',(-38.4596864613027,17.2339662976765,-3.02617273205817));
#35298=CARTESIAN_POINT('Ctrl Pts',(-38.4763011808142,17.2765454650671,-3.02258998023486));
#35299=CARTESIAN_POINT('Ctrl Pts',(-38.4954157055941,17.3386458788027,-3.01730425152133));
#35300=CARTESIAN_POINT('Ctrl Pts',(-38.5058190053368,17.3896723095994,-3.0128910139563));
#35301=CARTESIAN_POINT('Ctrl Pts',(-38.5117501031248,17.4284572602049,-3.00950811920092));
#35302=CARTESIAN_POINT('Ctrl Pts',(-38.5134146825683,17.4414715854915,-3.00836831081549));
#35303=CARTESIAN_POINT('Ctrl Pts',(-38.5161053987673,17.4676759533342,-3.00606351257013));
#35304=CARTESIAN_POINT('Ctrl Pts',(-38.5171225993645,17.4807801627204,-3.00490606944401));
#35305=CARTESIAN_POINT('Ctrl Pts',(-38.5186672398078,17.5100035515609,-3.0023138950648));
#35306=CARTESIAN_POINT('Ctrl Pts',(-38.5190286374484,17.5261237028805,-3.00087654313128));
#35307=CARTESIAN_POINT('Ctrl Pts',(-38.5189000091045,17.5422403141662,-2.99943193309589));
#35308=CARTESIAN_POINT('',(-38.0645261134423,18.255001868818,-2.93018339529753));
#35309=CARTESIAN_POINT('Ctrl Pts',(-38.5189000091045,17.5422403141662,-2.99943193309589));
#35310=CARTESIAN_POINT('Ctrl Pts',(-38.518819629035,17.5523116117943,-2.99852919384351));
#35311=CARTESIAN_POINT('Ctrl Pts',(-38.5185478927787,17.5623815270316,-2.99762362028695));
#35312=CARTESIAN_POINT('Ctrl Pts',(-38.5174831792733,17.5855404169291,-2.9955341060631));
#35313=CARTESIAN_POINT('Ctrl Pts',(-38.5165576565204,17.5986284329933,-2.99434819030326));
#35314=CARTESIAN_POINT('Ctrl Pts',(-38.5146791299617,17.6182569082276,-2.99256197428916));
#35315=CARTESIAN_POINT('Ctrl Pts',(-38.5139702987777,17.624806343346,-2.99196468640024));
#35316=CARTESIAN_POINT('Ctrl Pts',(-38.5123929064259,17.6378655121742,-2.99077117076634));
#35317=CARTESIAN_POINT('Ctrl Pts',(-38.5080511096546,17.6703979780115,-2.98779152237676));
#35318=CARTESIAN_POINT('Ctrl Pts',(-38.4967136126686,17.727935441958,-2.98246468554883));
#35319=CARTESIAN_POINT('Ctrl Pts',(-38.4742706912444,17.8025288092669,-2.97544207174657));
#35320=CARTESIAN_POINT('Ctrl Pts',(-38.454411593118,17.8508389101167,-2.97081849908883));
#35321=CARTESIAN_POINT('Ctrl Pts',(-38.4404194899548,17.8805751295757,-2.96794982485069));
#35322=CARTESIAN_POINT('Ctrl Pts',(-38.4375384803318,17.8865058429242,-2.967376526089));
#35323=CARTESIAN_POINT('Ctrl Pts',(-38.4316473483778,17.8982598993618,-2.96623805154997));
#35324=CARTESIAN_POINT('Ctrl Pts',(-38.4226095803834,17.9157483563618,-2.96454075450265));
#35325=CARTESIAN_POINT('Ctrl Pts',(-38.40012241695,17.9555624401979,-2.96065368940274));
#35326=CARTESIAN_POINT('Ctrl Pts',(-38.3640776936724,18.0096595981727,-2.95531050337563));
#35327=CARTESIAN_POINT('Ctrl Pts',(-38.3310991261845,18.0500004283726,-2.95126832284971));
#35328=CARTESIAN_POINT('Ctrl Pts',(-38.3047809236703,18.0791333861947,-2.94833016157896));
#35329=CARTESIAN_POINT('Ctrl Pts',(-38.2957436722637,18.0886569280017,-2.94736638630857));
#35330=CARTESIAN_POINT('Ctrl Pts',(-38.2817826469739,18.1026552032221,-2.94594525661301));
#35331=CARTESIAN_POINT('Ctrl Pts',(-38.2770696331703,18.1072649271286,-2.94547649987763));
#35332=CARTESIAN_POINT('Ctrl Pts',(-38.2675578378121,18.1163414658276,-2.94455208056439));
#35333=CARTESIAN_POINT('Ctrl Pts',(-38.2435389562924,18.1386979602117,-2.94227145996936));
#35334=CARTESIAN_POINT('Ctrl Pts',(-38.198184360507,18.1759736987718,-2.93843840821149));
#35335=CARTESIAN_POINT('Ctrl Pts',(-38.1549150551439,18.2049773241328,-2.9354232729364));
#35336=CARTESIAN_POINT('Ctrl Pts',(-38.1213464392414,18.2251692867483,-2.93331492411179));
#35337=CARTESIAN_POINT('Ctrl Pts',(-38.1042825224182,18.2348744500654,-2.93229905812222));
#35338=CARTESIAN_POINT('Ctrl Pts',(-38.0867927304674,18.243984444565,-2.93134241094606));
#35339=CARTESIAN_POINT('Ctrl Pts',(-38.0754919523261,18.2496943815878,-2.93074218958385));
#35340=CARTESIAN_POINT('Ctrl Pts',(-38.0700213262657,18.252380813858,-2.93045951516175));
#35341=CARTESIAN_POINT('Ctrl Pts',(-38.0645262657606,18.2550018687314,-2.93018339473831));
#35342=CARTESIAN_POINT('Ctrl Pts',(-37.718924746634,19.3314643670594,-4.62273145772315));
#35343=CARTESIAN_POINT('Ctrl Pts',(-37.7240432796227,19.3314643670594,-4.62273145772315));
#35344=CARTESIAN_POINT('Ctrl Pts',(-37.729105675728,19.330917508136,-4.62236438057516));
#35345=CARTESIAN_POINT('Ctrl Pts',(-37.7429480950038,19.3279914277147,-4.62039543755766));
#35346=CARTESIAN_POINT('Ctrl Pts',(-37.7511301340406,19.3246331108791,-4.61813211791741));
#35347=CARTESIAN_POINT('Ctrl Pts',(-37.7709118757918,19.3136757017161,-4.6106867021804));
#35348=CARTESIAN_POINT('Ctrl Pts',(-37.7817536948118,19.3044969837231,-4.60439028856606));
#35349=CARTESIAN_POINT('Ctrl Pts',(-37.8119215619376,19.273950159203,-4.58308087636467));
#35350=CARTESIAN_POINT('Ctrl Pts',(-37.8293065757878,19.2470367921451,-4.56367620611464));
#35351=CARTESIAN_POINT('Ctrl Pts',(-37.8842261422008,19.1493119759434,-4.49018612732299));
#35352=CARTESIAN_POINT('Ctrl Pts',(-37.9205683373981,19.0452717254973,-4.40565062734794));
#35353=CARTESIAN_POINT('Ctrl Pts',(-37.9994181115573,18.7553638270197,-4.10740388440347));
#35354=CARTESIAN_POINT('Ctrl Pts',(-38.0314877466367,18.5690397639075,-3.85835872738472));
#35355=CARTESIAN_POINT('Ctrl Pts',(-38.0598088046867,18.3530721778374,-3.36031585786156));
#35356=CARTESIAN_POINT('Ctrl Pts',(-38.0646084270943,18.2960215435642,-3.16946171823003));
#35357=CARTESIAN_POINT('Ctrl Pts',(-38.0646084270943,18.2621718608173,-2.9739074883211));
#35358=CARTESIAN_POINT('Ctrl Pts',(-38.0646084270943,18.2596508721519,-2.95934339326693));
#35359=CARTESIAN_POINT('Ctrl Pts',(-38.0645810063647,18.2572609718871,-2.94476807941075));
#35360=CARTESIAN_POINT('Ctrl Pts',(-38.0645262657607,18.2550018687316,-2.93018339473923));
#35361=CARTESIAN_POINT('',(-37.718924746634,23.3605792411954,-3.81059743858941));
#35362=CARTESIAN_POINT('Origin',(-37.718924746634,21.,-2.5));
#35363=CARTESIAN_POINT('Origin',(-37.718924746634,24.0600101274756,-4.19892260557888));
#35364=CARTESIAN_POINT('Origin',(-17.718924746634,21.,7.));
#35365=CARTESIAN_POINT('',(-17.718924746634,24.1393970581951,7.61982748486642));
#35366=CARTESIAN_POINT('Origin',(-17.718924746634,24.9242463227439,7.77478435608303));
#35367=CARTESIAN_POINT('',(-17.718924746634,17.8056396357716,6.81010093219959));
#35368=CARTESIAN_POINT('Origin',(-17.718924746634,21.,7.));
#35369=CARTESIAN_POINT('',(-18.503934654988,16.8564417728896,6.70366763718318));
#35370=CARTESIAN_POINT('Ctrl Pts',(-17.718924746634,17.8056396357716,6.81010093219959));
#35371=CARTESIAN_POINT('Ctrl Pts',(-17.7437642274753,17.805639936155,6.81010096743885));
#35372=CARTESIAN_POINT('Ctrl Pts',(-17.7945806620485,17.8032736219272,6.80985504288097));
#35373=CARTESIAN_POINT('Ctrl Pts',(-17.8705625761499,17.7924930279374,6.80873329662359));
#35374=CARTESIAN_POINT('Ctrl Pts',(-17.921492828803,17.7801311535749,6.80744359855836));
#35375=CARTESIAN_POINT('Ctrl Pts',(-17.9531061110628,17.7707796265052,6.80646566831214));
#35376=CARTESIAN_POINT('Ctrl Pts',(-17.9594238791357,17.7688257129027,6.80626124067242));
#35377=CARTESIAN_POINT('Ctrl Pts',(-17.9719700525308,17.7647754194567,6.80583724177927));
#35378=CARTESIAN_POINT('Ctrl Pts',(-17.9906772709459,17.7584809008687,6.80517797306814));
#35379=CARTESIAN_POINT('Ctrl Pts',(-18.0335480566535,17.7422697905638,6.80347718720341));
#35380=CARTESIAN_POINT('Ctrl Pts',(-18.0926092393002,17.7148435014562,6.80058915066718));
#35381=CARTESIAN_POINT('Ctrl Pts',(-18.1375535774513,17.6883976114347,6.79778673808222));
#35382=CARTESIAN_POINT('Ctrl Pts',(-18.1703813397044,17.6668424494962,6.7954934838427));
#35383=CARTESIAN_POINT('Ctrl Pts',(-18.1811769170662,17.6593700941287,6.79469709774963));
#35384=CARTESIAN_POINT('Ctrl Pts',(-18.1971452253442,17.6477217806831,6.7934531112477));
#35385=CARTESIAN_POINT('Ctrl Pts',(-18.2024277795054,17.6437672898988,6.79303038089619));
#35386=CARTESIAN_POINT('Ctrl Pts',(-18.2128589038726,17.6357562610639,6.79217313373619));
#35387=CARTESIAN_POINT('Ctrl Pts',(-18.2386372906825,17.6154455326787,6.78999755925242));
#35388=CARTESIAN_POINT('Ctrl Pts',(-18.2823885839682,17.5763805902293,6.78579238930071));
#35389=CARTESIAN_POINT('Ctrl Pts',(-18.335199074135,17.5190716076668,6.77956801624083));
#35390=CARTESIAN_POINT('Ctrl Pts',(-18.3667048102232,17.4773678386001,6.77499525393865));
#35391=CARTESIAN_POINT('Ctrl Pts',(-18.3851987148915,17.4501719281585,6.77199753817605));
#35392=CARTESIAN_POINT('Ctrl Pts',(-18.3888300757025,17.4446866457309,6.77139215707454));
#35393=CARTESIAN_POINT('Ctrl Pts',(-18.3959354367756,17.4336604106349,6.77017369611277));
#35394=CARTESIAN_POINT('Ctrl Pts',(-18.4063691081392,17.4170215549816,6.76833269446205));
#35395=CARTESIAN_POINT('Ctrl Pts',(-18.4291527063757,17.3775050758205,6.76394379344769));
#35396=CARTESIAN_POINT('Ctrl Pts',(-18.4573221090362,17.3191117620688,6.7574088008242));
#35397=CARTESIAN_POINT('Ctrl Pts',(-18.4752252427967,17.2703441070257,6.75189395522156));
#35398=CARTESIAN_POINT('Ctrl Pts',(-18.4868790983566,17.2329825881833,6.74764614586732));
#35399=CARTESIAN_POINT('Ctrl Pts',(-18.4904676066854,17.2203975511552,6.74621156959817));
#35400=CARTESIAN_POINT('Ctrl Pts',(-18.4970395596012,17.1949594180543,6.74330409490759));
#35401=CARTESIAN_POINT('Ctrl Pts',(-18.4999963095876,17.1822091381994,6.74184294570588));
#35402=CARTESIAN_POINT('Ctrl Pts',(-18.5078943414964,17.1438889055983,6.73744002022504));
#35403=CARTESIAN_POINT('Ctrl Pts',(-18.5158427423235,17.0925907201539,6.7315152759013));
#35404=CARTESIAN_POINT('Ctrl Pts',(-18.5187347637249,17.0408921832155,6.72548308130679));
#35405=CARTESIAN_POINT('Ctrl Pts',(-18.5189935253682,17.001967015951,6.72091847384795));
#35406=CARTESIAN_POINT('Ctrl Pts',(-18.5187608417161,16.9889667041771,6.71939018918219));
#35407=CARTESIAN_POINT('Ctrl Pts',(-18.5176482397637,16.9629148154356,6.71632002713026));
#35408=CARTESIAN_POINT('Ctrl Pts',(-18.5167674431033,16.9498537547869,6.71477702649695));
#35409=CARTESIAN_POINT('Ctrl Pts',(-18.5131381950841,16.9106515627424,6.71013447800261));
#35410=CARTESIAN_POINT('Ctrl Pts',(-18.5093031380889,16.8838623643511,6.70694639835343));
#35411=CARTESIAN_POINT('Ctrl Pts',(-18.5041119180302,16.8573391865427,6.70377496037948));
#35412=CARTESIAN_POINT('Ctrl Pts',(-18.5039346585515,16.8564417721916,6.70366763713326));
#35413=CARTESIAN_POINT('',(-17.718924746634,16.2147387265569,6.62413484998572));
#35414=CARTESIAN_POINT('Ctrl Pts',(-18.5039346585515,16.8564417721916,6.70366763713326));
#35415=CARTESIAN_POINT('Ctrl Pts',(-18.4990520338128,16.8317224311244,6.70071141080989));
#35416=CARTESIAN_POINT('Ctrl Pts',(-18.4929900691117,16.8072344206075,6.69776969800538));
#35417=CARTESIAN_POINT('Ctrl Pts',(-18.4838530007988,16.7766971106601,6.69408581848945));
#35418=CARTESIAN_POINT('Ctrl Pts',(-18.481891446972,16.7704267103922,6.69332855080655));
#35419=CARTESIAN_POINT('Ctrl Pts',(-18.4778252926784,16.7579733179017,6.69182295030277));
#35420=CARTESIAN_POINT('Ctrl Pts',(-18.4715061772404,16.7394035120316,6.68957544372212));
#35421=CARTESIAN_POINT('Ctrl Pts',(-18.4552314545873,16.6968413309535,6.68440761131254));
#35422=CARTESIAN_POINT('Ctrl Pts',(-18.4276933217952,16.6381885851568,6.67724190315151));
#35423=CARTESIAN_POINT('Ctrl Pts',(-18.4011288767869,16.5935389735778,6.67174551679615));
#35424=CARTESIAN_POINT('Ctrl Pts',(-18.379470949919,16.5609208580899,6.66771645958401));
#35425=CARTESIAN_POINT('Ctrl Pts',(-18.371962026184,16.5501932599997,6.66638900938586));
#35426=CARTESIAN_POINT('Ctrl Pts',(-18.3563525988859,16.5290344037261,6.6637664185393));
#35427=CARTESIAN_POINT('Ctrl Pts',(-18.3483028175492,16.518672885763,6.66247991996544));
#35428=CARTESIAN_POINT('Ctrl Pts',(-18.3234959875097,16.4883125244316,6.65870444956298));
#35429=CARTESIAN_POINT('Ctrl Pts',(-18.2886161598463,16.4496856970626,6.65388502913153));
#35430=CARTESIAN_POINT('Ctrl Pts',(-18.2502021300267,16.4146892602587,6.64949372875457));
#35431=CARTESIAN_POINT('Ctrl Pts',(-18.2200556979461,16.3898138372835,6.6463649871714));
#35432=CARTESIAN_POINT('Ctrl Pts',(-18.2046479670122,16.3777196541662,6.6448418639455));
#35433=CARTESIAN_POINT('Ctrl Pts',(-18.1887307386623,16.3661486304109,6.64338209528373));
#35434=CARTESIAN_POINT('Ctrl Pts',(-18.1780048436419,16.3585520846253,6.64242320052006));
#35435=CARTESIAN_POINT('Ctrl Pts',(-18.1725777225939,16.3548079090092,6.64195030912558));
#35436=CARTESIAN_POINT('Ctrl Pts',(-18.1452408175762,16.336443365656,6.63962960324257));
#35437=CARTESIAN_POINT('Ctrl Pts',(-18.1003916816812,16.309440410321,6.63620924911408));
#35438=CARTESIAN_POINT('Ctrl Pts',(-18.0298938090306,16.2758481786742,6.63193887289174));
#35439=CARTESIAN_POINT('Ctrl Pts',(-17.9807546607501,16.2580417410788,6.62966864832929));
#35440=CARTESIAN_POINT('Ctrl Pts',(-17.9493568559871,16.2483826473291,6.62843600572121));
#35441=CARTESIAN_POINT('Ctrl Pts',(-17.9430429233677,16.2465244962757,6.62819881007824));
#35442=CARTESIAN_POINT('Ctrl Pts',(-17.9303455620517,16.2429571389029,6.62774332035942));
#35443=CARTESIAN_POINT('Ctrl Pts',(-17.9239586678768,16.2412473003856,6.62752494537815));
#35444=CARTESIAN_POINT('Ctrl Pts',(-17.9047992194454,16.2363691840864,6.62690179590072));
#35445=CARTESIAN_POINT('Ctrl Pts',(-17.8663831007668,16.2275932534501,6.62578012373376));
#35446=CARTESIAN_POINT('Ctrl Pts',(-17.8018815463507,16.2177528554165,6.62452085559388));
#35447=CARTESIAN_POINT('Ctrl Pts',(-17.7497820050364,16.2149044523123,6.62415607053616));
#35448=CARTESIAN_POINT('Ctrl Pts',(-17.7220460714532,16.2147432699944,6.62413543169615));
#35449=CARTESIAN_POINT('Ctrl Pts',(-17.7204856339758,16.2147387305049,6.62413485045537));
#35450=CARTESIAN_POINT('Ctrl Pts',(-17.718924746634,16.2147387265569,6.62413484998572));
#35451=CARTESIAN_POINT('',(-16.9340264357173,17.1635288511797,6.73969634067107));
#35452=CARTESIAN_POINT('Ctrl Pts',(-17.718924746634,16.2147387265569,6.62413484998572));
#35453=CARTESIAN_POINT('Ctrl Pts',(-17.7073901207539,16.2147386973818,6.62413484651512));
#35454=CARTESIAN_POINT('Ctrl Pts',(-17.6958309281618,16.214986349411,6.62416655835217));
#35455=CARTESIAN_POINT('Ctrl Pts',(-17.6710950665175,16.2160521816488,6.62430302504923));
#35456=CARTESIAN_POINT('Ctrl Pts',(-17.6578800967229,16.2169470871587,6.62441760265911));
#35457=CARTESIAN_POINT('Ctrl Pts',(-17.618539737525,16.2205845052797,6.62488321315798));
#35458=CARTESIAN_POINT('Ctrl Pts',(-17.5667062451157,16.2279645901634,6.62582775169573));
#35459=CARTESIAN_POINT('Ctrl Pts',(-17.4907655414855,16.2464159284195,6.62818590268485));
#35460=CARTESIAN_POINT('Ctrl Pts',(-17.4413448027588,16.2636382051738,6.63038235379587));
#35461=CARTESIAN_POINT('Ctrl Pts',(-17.4108450610503,16.275986019519,6.63195461113918));
#35462=CARTESIAN_POINT('Ctrl Pts',(-17.4047573329155,16.2785381347074,6.63227946159647));
#35463=CARTESIAN_POINT('Ctrl Pts',(-17.392656553187,16.2837875791675,6.63294738475772));
#35464=CARTESIAN_POINT('Ctrl Pts',(-17.3746406531229,16.2918680856118,6.63397514809339));
#35465=CARTESIAN_POINT('Ctrl Pts',(-17.333543938793,16.3121571257405,6.63655266849902));
#35466=CARTESIAN_POINT('Ctrl Pts',(-17.2774646495951,16.3451542416341,6.64073395855193));
#35467=CARTESIAN_POINT('Ctrl Pts',(-17.2353718106155,16.37577953871,6.64459834653782));
#35468=CARTESIAN_POINT('Ctrl Pts',(-17.2048581546413,16.4003601492348,6.64769185760752));
#35469=CARTESIAN_POINT('Ctrl Pts',(-17.1948632441005,16.4088227697541,6.64875561975649));
#35470=CARTESIAN_POINT('Ctrl Pts',(-17.1801404493712,16.4219281696642,6.65040072833764));
#35471=CARTESIAN_POINT('Ctrl Pts',(-17.1752713191261,16.4263714613955,6.65095812427235));
#35472=CARTESIAN_POINT('Ctrl Pts',(-17.1656691894842,16.4353539396767,6.65208416112202));
#35473=CARTESIAN_POINT('Ctrl Pts',(-17.1419929093713,16.4580609542231,6.65492876298833));
#35474=CARTESIAN_POINT('Ctrl Pts',(-17.102285326311,16.5011517480721,6.66030848420105));
#35475=CARTESIAN_POINT('Ctrl Pts',(-17.0553941325125,16.5632214156579,6.66800927694668));
#35476=CARTESIAN_POINT('Ctrl Pts',(-17.02817892591,16.6076872190025,6.67348812469957));
#35477=CARTESIAN_POINT('Ctrl Pts',(-17.0124748344788,16.6364744349879,6.67702127116173));
#35478=CARTESIAN_POINT('Ctrl Pts',(-17.0093968359646,16.6422873010984,6.67773402886076));
#35479=CARTESIAN_POINT('Ctrl Pts',(-17.0034052213629,16.6539503720992,6.67916272927562));
#35480=CARTESIAN_POINT('Ctrl Pts',(-16.9946522678938,16.6715209503219,6.6813130134438));
#35481=CARTESIAN_POINT('Ctrl Pts',(-16.9758596752147,16.7130474928295,6.68638011044747));
#35482=CARTESIAN_POINT('Ctrl Pts',(-16.9535805813423,16.7738516553674,6.6937548144664));
#35483=CARTESIAN_POINT('Ctrl Pts',(-16.9405788954198,16.824058627078,6.69979202793982));
#35484=CARTESIAN_POINT('Ctrl Pts',(-16.9326693696693,16.8623113652087,6.7043705098731));
#35485=CARTESIAN_POINT('Ctrl Pts',(-16.9303403635677,16.8751620394352,6.70590511847467));
#35486=CARTESIAN_POINT('Ctrl Pts',(-16.9273175517075,16.8945907808836,6.7082197633061));
#35487=CARTESIAN_POINT('Ctrl Pts',(-16.9263885149695,16.9010931471414,6.70899351049072));
#35488=CARTESIAN_POINT('Ctrl Pts',(-16.9246942153957,16.9141079987304,6.71054035440315));
#35489=CARTESIAN_POINT('Ctrl Pts',(-16.9239281128653,16.9206255601628,6.71131405642648));
#35490=CARTESIAN_POINT('Ctrl Pts',(-16.920503229783,16.9532643609428,6.71518393496801));
#35491=CARTESIAN_POINT('Ctrl Pts',(-16.9176572816504,17.0053713760446,6.72133216615983));
#35492=CARTESIAN_POINT('Ctrl Pts',(-16.9210645020192,17.0831969363472,6.73042420827673));
#35493=CARTESIAN_POINT('Ctrl Pts',(-16.9284495603501,17.1348575716213,6.73639817772183));
#35494=CARTESIAN_POINT('Ctrl Pts',(-16.933645427244,17.161596976226,6.73947417131325));
#35495=CARTESIAN_POINT('Ctrl Pts',(-16.9338350389026,17.1625631269947,6.73958529147372));
#35496=CARTESIAN_POINT('Ctrl Pts',(-16.9340264381954,17.1635288506924,6.739696340638));
#35497=CARTESIAN_POINT('Ctrl Pts',(-16.9340264381954,17.1635288506924,6.739696340638));
#35498=CARTESIAN_POINT('Ctrl Pts',(-16.9351109981369,17.1690011030818,6.74032559831906));
#35499=CARTESIAN_POINT('Ctrl Pts',(-16.9362529571807,17.1744596426592,6.74095257638505));
#35500=CARTESIAN_POINT('Ctrl Pts',(-16.9388568010243,17.186283641671,6.74230919334707));
#35501=CARTESIAN_POINT('Ctrl Pts',(-16.9433081085948,17.2053688483162,6.74449603083134));
#35502=CARTESIAN_POINT('Ctrl Pts',(-16.9552863579889,17.2492826463594,6.74950793438583));
#35503=CARTESIAN_POINT('Ctrl Pts',(-16.9768561553689,17.3102847941397,6.75641516254366));
#35504=CARTESIAN_POINT('Ctrl Pts',(-16.9988177277096,17.3572579116379,6.76167884669307));
#35505=CARTESIAN_POINT('Ctrl Pts',(-17.0170860870797,17.3917891174648,6.76552887059901));
#35506=CARTESIAN_POINT('Ctrl Pts',(-17.0234756011144,17.4031828736261,6.76679589924646));
#35507=CARTESIAN_POINT('Ctrl Pts',(-17.033519120055,17.420094939934,6.76867182765814));
#35508=CARTESIAN_POINT('Ctrl Pts',(-17.036947410201,17.4257086449722,6.76929371066084));
#35509=CARTESIAN_POINT('Ctrl Pts',(-17.0439406736216,17.4368468258563,6.77052603009099));
#35510=CARTESIAN_POINT('Ctrl Pts',(-17.0617383518508,17.464424047629,6.77357320762057));
#35511=CARTESIAN_POINT('Ctrl Pts',(-17.0965584766246,17.5116883613631,6.77876195919935));
#35512=CARTESIAN_POINT('Ctrl Pts',(-17.1313811716546,17.550398225015,6.78297104726967));
#35513=CARTESIAN_POINT('Ctrl Pts',(-17.1589589461814,17.5781840235213,6.78597933669272));
#35514=CARTESIAN_POINT('Ctrl Pts',(-17.1731136118301,17.5917647691345,6.78744629220304));
#35515=CARTESIAN_POINT('Ctrl Pts',(-17.187824895331,17.604870422577,6.78885736137875));
#35516=CARTESIAN_POINT('Ctrl Pts',(-17.197757352162,17.6135008803574,6.78978561002206));
#35517=CARTESIAN_POINT('Ctrl Pts',(-17.2027922558143,17.6177677510881,6.79024403430444));
#35518=CARTESIAN_POINT('Ctrl Pts',(-17.2281606385066,17.6387327999837,6.79249414672339));
#35519=CARTESIAN_POINT('Ctrl Pts',(-17.2700991321529,17.6700274474653,6.79583792030219));
#35520=CARTESIAN_POINT('Ctrl Pts',(-17.3369316643949,17.7104237496203,6.80012224085272));
#35521=CARTESIAN_POINT('Ctrl Pts',(-17.384096505469,17.7330010511229,6.80250132612996));
#35522=CARTESIAN_POINT('Ctrl Pts',(-17.4144120897862,17.7457144101392,6.80383778899833));
#35523=CARTESIAN_POINT('Ctrl Pts',(-17.4205171825721,17.7481870458338,6.80409753968387));
#35524=CARTESIAN_POINT('Ctrl Pts',(-17.4328122755551,17.7529906441943,6.80460184646387));
#35525=CARTESIAN_POINT('Ctrl Pts',(-17.4389911007516,17.7553170440476,6.80484592328607));
#35526=CARTESIAN_POINT('Ctrl Pts',(-17.4575584676089,17.7620489786898,6.80555181272847));
#35527=CARTESIAN_POINT('Ctrl Pts',(-17.4948927783289,17.7745487978019,6.8068607858668));
#35528=CARTESIAN_POINT('Ctrl Pts',(-17.5580921261442,17.7906693688048,6.80854332410195));
#35529=CARTESIAN_POINT('Ctrl Pts',(-17.609677577175,17.7986089778658,6.80936966339988));
#35530=CARTESIAN_POINT('Ctrl Pts',(-17.6487571126183,17.8026771607332,6.80979290243887));
#35531=CARTESIAN_POINT('Ctrl Pts',(-17.6618488145178,17.8037182435059,6.80990116365931));
#35532=CARTESIAN_POINT('Ctrl Pts',(-17.6815859652612,17.8047986328145,6.81001349995407));
#35533=CARTESIAN_POINT('Ctrl Pts',(-17.6881898144631,17.8050787312053,6.81004262041923));
#35534=CARTESIAN_POINT('Ctrl Pts',(-17.7013903129314,17.8054755893881,6.8100838811623));
#35535=CARTESIAN_POINT('Ctrl Pts',(-17.7094380700629,17.8056177510387,6.81009865616776));
#35536=CARTESIAN_POINT('Ctrl Pts',(-17.7174696864885,17.8056396181756,6.81010093013532));
#35537=CARTESIAN_POINT('Ctrl Pts',(-17.718924746634,17.8056396357716,6.81010093219959));
#35538=CARTESIAN_POINT('Origin',(-37.718924746634,24.0015386818685,-0.183979981426689));
#35539=CARTESIAN_POINT('',(-37.718924746634,25.0506850112887,-0.766467731910886));
#35540=CARTESIAN_POINT('Origin',(-37.718924746634,25.7501158975689,-1.15479289890034));
#35541=CARTESIAN_POINT('Origin',(-37.718924746634,24.0015386818685,-0.183979981426689));
#35542=CARTESIAN_POINT('Origin',(-17.718924746634,11.0131091329632,0.793137146317211));
#35543=CARTESIAN_POINT('',(-17.718924746634,24.9441835787041,3.54362161041199));
#35544=CARTESIAN_POINT('Origin',(-17.718924746634,11.0131091329632,0.793137146317211));
#35545=CARTESIAN_POINT('Origin',(-17.718924746634,25.7290328432529,3.6985784816286));
#35546=CARTESIAN_POINT('Origin',(-31.,34.999999994595,6.54998265276524E-10));
#35547=CARTESIAN_POINT('',(-31.,34.999999994595,4.000000000655));
#35548=CARTESIAN_POINT('Origin',(-31.,34.999999994595,6.54998265276524E-10));
#35549=CARTESIAN_POINT('',(-39.,34.999999994595,4.000000000655));
#35550=CARTESIAN_POINT('',(-31.,34.999999994595,4.000000000655));
#35551=CARTESIAN_POINT('Origin',(-39.,34.999999994595,6.54998265276524E-10));
#35552=CARTESIAN_POINT('Origin',(-45.7,34.999999994595,6.54998265276524E-10));
#35553=CARTESIAN_POINT('',(-45.7,34.999999994595,4.000000000655));
#35554=CARTESIAN_POINT('',(-45.7,34.999999994595,-3.999999999345));
#35555=CARTESIAN_POINT('Origin',(-45.7,34.999999994595,6.54998265276524E-10));
#35556=CARTESIAN_POINT('Origin',(-45.7,34.999999994595,6.54998265276524E-10));
#35557=CARTESIAN_POINT('',(-46.,34.999999994595,-3.699999999345));
#35558=CARTESIAN_POINT('',(-45.7,34.999999994595,-3.999999999345));
#35559=CARTESIAN_POINT('Origin',(-46.,34.999999994595,6.54998265276524E-10));
#35560=CARTESIAN_POINT('Origin',(-31.,34.999999994595,6.54998265276524E-10));
#35561=CARTESIAN_POINT('',(-45.5,34.999999994595,4.000000000655));
#35562=CARTESIAN_POINT('',(-45.5,30.999999994595,6.5499951014128E-10));
#35563=CARTESIAN_POINT('Origin',(-45.5,34.999999994595,6.55E-10));
#35564=CARTESIAN_POINT('Origin',(-45.5,34.999999994595,6.55E-10));
#35565=CARTESIAN_POINT('',(-31.,34.999999994595,4.000000000655));
#35566=CARTESIAN_POINT('Origin',(-56.6690017314647,48.5946168001447,-6.3392739254555));
#35567=CARTESIAN_POINT('',(-39.,48.5946168001447,-3.5392739254555));
#35568=CARTESIAN_POINT('',(-39.,45.7946168001447,-6.3392739254555));
#35569=CARTESIAN_POINT('Origin',(-39.,48.5946168001447,-6.3392739254555));
#35570=CARTESIAN_POINT('',(-45.5,45.7946168001447,-6.3392739254555));
#35571=CARTESIAN_POINT('',(-56.6690017314647,45.7946168001447,-6.3392739254555));
#35572=CARTESIAN_POINT('',(-45.5,51.3913318198147,-6.47486558726599));
#35573=CARTESIAN_POINT('Origin',(-45.5,48.5946168001447,-6.3392739254555));
#35574=CARTESIAN_POINT('',(-45.,51.3913318198147,-6.47486558726599));
#35575=CARTESIAN_POINT('',(-45.,51.3913318198147,-6.47486558726599));
#35576=CARTESIAN_POINT('',(-45.,49.0519043965673,-3.57686771815033));
#35577=CARTESIAN_POINT('Origin',(-45.,48.5946168001447,-6.3392739254555));
#35578=CARTESIAN_POINT('',(-44.,48.0109313132992,-3.60078688834068));
#35579=CARTESIAN_POINT('Ctrl Pts',(-45.,49.0519043965673,-3.57686771815035));
#35580=CARTESIAN_POINT('Ctrl Pts',(-45.,48.9957251357862,-3.56756782624327));
#35581=CARTESIAN_POINT('Ctrl Pts',(-44.9951745711715,48.9392147266966,-3.55998370975779));
#35582=CARTESIAN_POINT('Ctrl Pts',(-44.9630876045502,48.7514236666012,-3.5405436690203));
#35583=CARTESIAN_POINT('Ctrl Pts',(-44.9151278102305,48.6247757407979,-3.53708953016471));
#35584=CARTESIAN_POINT('Ctrl Pts',(-44.7751927091309,48.3936711000784,-3.54406290383913));
#35585=CARTESIAN_POINT('Ctrl Pts',(-44.6832058663738,48.2908272034433,-3.55457782983572));
#35586=CARTESIAN_POINT('Ctrl Pts',(-44.4781736557104,48.1357194801071,-3.57614322542986));
#35587=CARTESIAN_POINT('Ctrl Pts',(-44.3689066136297,48.0798168915966,-3.58679425502691));
#35588=CARTESIAN_POINT('Ctrl Pts',(-44.1695174787766,48.022881826187,-3.59816232312806));
#35589=CARTESIAN_POINT('Ctrl Pts',(-44.0850432793417,48.0109313132992,-3.60078688834069));
#35590=CARTESIAN_POINT('Ctrl Pts',(-44.,48.0109313132992,-3.60078688834069));
#35591=CARTESIAN_POINT('',(-43.,48.0109313132992,-3.60078688834069));
#35592=CARTESIAN_POINT('',(-43.5,48.0109313132992,-3.60078688834069));
#35593=CARTESIAN_POINT('',(-42.,49.0519043965673,-3.57686771815033));
#35594=CARTESIAN_POINT('Ctrl Pts',(-43.,48.0109313132992,-3.60078688834069));
#35595=CARTESIAN_POINT('Ctrl Pts',(-42.9691893177197,48.0109313132992,-3.60078688834069));
#35596=CARTESIAN_POINT('Ctrl Pts',(-42.9383039359468,48.0125011261107,-3.60045085699698));
#35597=CARTESIAN_POINT('Ctrl Pts',(-42.7839130068819,48.0283194174735,-3.59710789163843));
#35598=CARTESIAN_POINT('Ctrl Pts',(-42.6652177139826,48.0659731655586,-3.58898860882495));
#35599=CARTESIAN_POINT('Ctrl Pts',(-42.4345634815223,48.1900964691459,-3.56785168328553));
#35600=CARTESIAN_POINT('Ctrl Pts',(-42.3270875778571,48.2807056420326,-3.55483109731437));
#35601=CARTESIAN_POINT('Ctrl Pts',(-42.1572239135169,48.490393491272,-3.53934603484932));
#35602=CARTESIAN_POINT('Ctrl Pts',(-42.0931335275273,48.6071980157876,-3.53651307227344));
#35603=CARTESIAN_POINT('Ctrl Pts',(-42.0177600379801,48.8361031309839,-3.54776238095549));
#35604=CARTESIAN_POINT('Ctrl Pts',(-42.,48.9440345489199,-3.55901098758455));
#35605=CARTESIAN_POINT('Ctrl Pts',(-42.,49.0519043965673,-3.57686771815035));
#35606=CARTESIAN_POINT('',(-42.,50.599158431302,-8.29421966612385));
#35607=CARTESIAN_POINT('Origin',(-42.,48.5946168001447,-6.3392739254555));
#35608=CARTESIAN_POINT('',(-45.,50.599158431302,-8.29421966612386));
#35609=CARTESIAN_POINT('',(-56.6690017314647,50.599158431302,-8.29421966612386));
#35610=CARTESIAN_POINT('',(-45.,50.5871414377259,-8.30646623141651));
#35611=CARTESIAN_POINT('Origin',(-45.,48.5946168001447,-6.3392739254555));
#35612=CARTESIAN_POINT('',(-45.5,50.5871414377259,-8.30646623141651));
#35613=CARTESIAN_POINT('',(-45.,50.5871414377259,-8.30646623141651));
#35614=CARTESIAN_POINT('Origin',(-45.5,48.5946168001447,-6.3392739254555));
#35615=CARTESIAN_POINT('Origin',(-39.,48.5946168001447,-6.3392739254555));
#35616=CARTESIAN_POINT('Origin',(-35.3179607461319,20.7255401693197,-2.54750793782168));
#35617=CARTESIAN_POINT('',(-30.,23.2255401693197,-2.54750793782168));
#35618=CARTESIAN_POINT('Origin',(-30.,20.7255401693197,-2.54750793782168));
#35619=CARTESIAN_POINT('',(-38.5,23.2255401693197,-2.54750793782168));
#35620=CARTESIAN_POINT('',(-35.3179607461319,23.2255401693197,-2.54750793782168));
#35621=CARTESIAN_POINT('',(-38.5,21.2255401693197,-0.0980181950384966));
#35622=CARTESIAN_POINT('Origin',(-38.5,20.7255401693197,-2.54750793782168));
#35623=CARTESIAN_POINT('',(-35.1565965239697,21.2255401693197,-0.0980181950384966));
#35624=CARTESIAN_POINT('',(-35.3179607461319,21.2255401693197,-0.0980181950384966));
#35625=CARTESIAN_POINT('',(-35.1565965239697,20.2255401693197,-0.0980181950385001));
#35626=CARTESIAN_POINT('Ctrl Pts',(-35.1565965239697,21.2255401693197,-0.098018195038502));
#35627=CARTESIAN_POINT('Ctrl Pts',(-35.0760059557493,21.2255401693197,-0.098018195038502));
#35628=CARTESIAN_POINT('Ctrl Pts',(-34.9884055345433,21.2153179188118,-0.0958304096017428));
#35629=CARTESIAN_POINT('Ctrl Pts',(-34.8229201950239,21.1669869100577,-0.0866687028340092));
#35630=CARTESIAN_POINT('Ctrl Pts',(-34.7450786649676,21.1287241345178,-0.0797242857551705));
#35631=CARTESIAN_POINT('Ctrl Pts',(-34.6299180077935,21.0381431963904,-0.0667841517369663));
#35632=CARTESIAN_POINT('Ctrl Pts',(-34.5820250297599,20.9842926662468,-0.0601688196471046));
#35633=CARTESIAN_POINT('Ctrl Pts',(-34.5170648437554,20.8612473945026,-0.0504311897554679));
#35634=CARTESIAN_POINT('Ctrl Pts',(-34.5,20.7920357336245,-0.0475079378216808));
#35635=CARTESIAN_POINT('Ctrl Pts',(-34.5,20.6590446050149,-0.0475079378216808));
#35636=CARTESIAN_POINT('Ctrl Pts',(-34.5170648437554,20.5898329441368,-0.0504311897554679));
#35637=CARTESIAN_POINT('Ctrl Pts',(-34.5820250297599,20.4667876723926,-0.0601688196471046));
#35638=CARTESIAN_POINT('Ctrl Pts',(-34.6299180077935,20.412937142249,-0.0667841517369663));
#35639=CARTESIAN_POINT('Ctrl Pts',(-34.7450786649676,20.3223562041216,-0.0797242857551706));
#35640=CARTESIAN_POINT('Ctrl Pts',(-34.8229201950239,20.2840934285817,-0.0866687028340092));
#35641=CARTESIAN_POINT('Ctrl Pts',(-34.9884055345433,20.2357624198276,-0.0958304096017427));
#35642=CARTESIAN_POINT('Ctrl Pts',(-35.0760059557493,20.2255401693197,-0.0980181950385028));
#35643=CARTESIAN_POINT('Ctrl Pts',(-35.1565965239697,20.2255401693197,-0.0980181950385028));
#35644=CARTESIAN_POINT('',(-38.5,20.2255401693197,-0.0980181950385001));
#35645=CARTESIAN_POINT('',(-35.3179607461319,20.2255401693197,-0.0980181950385001));
#35646=CARTESIAN_POINT('',(-38.5,18.8779263022516,-0.863369286101596));
#35647=CARTESIAN_POINT('Origin',(-38.5,20.7255401693197,-2.54750793782168));
#35648=CARTESIAN_POINT('',(-39.224471181792,18.2255370962949,-2.547507937818));
#35649=CARTESIAN_POINT('Ctrl Pts',(-38.5,18.8779263022516,-0.863369286101596));
#35650=CARTESIAN_POINT('Ctrl Pts',(-38.5,18.8418134627679,-0.902987510492509));
#35651=CARTESIAN_POINT('Ctrl Pts',(-38.5029913583948,18.8074241910345,-0.943268205815897));
#35652=CARTESIAN_POINT('Ctrl Pts',(-38.513756919099,18.741792668973,-1.02517424287596));
#35653=CARTESIAN_POINT('Ctrl Pts',(-38.5215384310811,18.7105519790673,-1.06679926913165));
#35654=CARTESIAN_POINT('Ctrl Pts',(-38.5411026664266,18.651029869407,-1.15141245973054));
#35655=CARTESIAN_POINT('Ctrl Pts',(-38.5528891238843,18.6227492495679,-1.19440046494414));
#35656=CARTESIAN_POINT('Ctrl Pts',(-38.5731607994899,18.5824620218676,-1.25992360068095));
#35657=CARTESIAN_POINT('Ctrl Pts',(-38.5803546854392,18.5693838675296,-1.28194731863795));
#35658=CARTESIAN_POINT('Ctrl Pts',(-38.5955434055275,18.5439521349797,-1.3263088029536));
#35659=CARTESIAN_POINT('Ctrl Pts',(-38.6034889685688,18.5316796196784,-1.34850420543431));
#35660=CARTESIAN_POINT('Ctrl Pts',(-38.6282756681186,18.4961209979196,-1.41515357438277));
#35661=CARTESIAN_POINT('Ctrl Pts',(-38.6460625712208,18.4740906795495,-1.45967140046796));
#35662=CARTESIAN_POINT('Ctrl Pts',(-38.6837385046754,18.4330942498066,-1.54895656553476));
#35663=CARTESIAN_POINT('Ctrl Pts',(-38.7036292324255,18.4141292052936,-1.59372355142654));
#35664=CARTESIAN_POINT('Ctrl Pts',(-38.745211491781,18.3790679312211,-1.68356735179541));
#35665=CARTESIAN_POINT('Ctrl Pts',(-38.788595931521,18.3468763471817,-1.77372069830513));
#35666=CARTESIAN_POINT('Ctrl Pts',(-38.8351353172829,18.3201595782086,-1.86459367854188));
#35667=CARTESIAN_POINT('Ctrl Pts',(-38.8710944633591,18.3021126177066,-1.9330522270599));
#35668=CARTESIAN_POINT('Ctrl Pts',(-38.8832569805968,18.296429086976,-1.95592235061537));
#35669=CARTESIAN_POINT('Ctrl Pts',(-38.9079166969854,18.2857197929667,-2.00176927464294));
#35670=CARTESIAN_POINT('Ctrl Pts',(-38.920357181891,18.2807186421253,-2.0246406900419));
#35671=CARTESIAN_POINT('Ctrl Pts',(-38.9579733632456,18.2667428790988,-2.09310093948371));
#35672=CARTESIAN_POINT('Ctrl Pts',(-39.0089188989727,18.2508425791602,-2.18398462221447));
#35673=CARTESIAN_POINT('Ctrl Pts',(-39.0873223383069,18.2347459403829,-2.3193393269623));
#35674=CARTESIAN_POINT('Ctrl Pts',(-39.1407093081975,18.2289758926703,-2.40904581727342));
#35675=CARTESIAN_POINT('Ctrl Pts',(-39.186472043237,18.2261235988577,-2.48508031520527));
#35676=CARTESIAN_POINT('Ctrl Pts',(-39.2054196067492,18.2255380886718,-2.51631704202074));
#35677=CARTESIAN_POINT('Ctrl Pts',(-39.2244711817888,18.2255371663434,-2.54750793782168));
#35678=CARTESIAN_POINT('',(-39.5,18.2644264063412,-2.9867334444556));
#35679=CARTESIAN_POINT('Ctrl Pts',(-39.2244711817953,18.2255370262464,-2.54750793781432));
#35680=CARTESIAN_POINT('Ctrl Pts',(-39.2589632575303,18.2255356570879,-2.60397760789945));
#35681=CARTESIAN_POINT('Ctrl Pts',(-39.2937962530053,18.2274503724719,-2.66029706465531));
#35682=CARTESIAN_POINT('Ctrl Pts',(-39.3289017777147,18.2312588219439,-2.71650663643555));
#35683=CARTESIAN_POINT('Ctrl Pts',(-39.3298642110874,18.2313632322583,-2.71804764652428));
#35684=CARTESIAN_POINT('Ctrl Pts',(-39.3308268508299,18.2314690702069,-2.71958857350432));
#35685=CARTESIAN_POINT('Ctrl Pts',(-39.331789695751,18.2315763362011,-2.72112941814041));
#35686=CARTESIAN_POINT('Ctrl Pts',(-39.3590347419993,18.2346115778152,-2.76472977626034));
#35687=CARTESIAN_POINT('Ctrl Pts',(-39.3864439213512,18.2387901600934,-2.80826403375964));
#35688=CARTESIAN_POINT('Ctrl Pts',(-39.4139900200143,18.2441217238816,-2.85174879411711));
#35689=CARTESIAN_POINT('Ctrl Pts',(-39.4144915148842,18.2442187885121,-2.85254046282139));
#35690=CARTESIAN_POINT('Ctrl Pts',(-39.414993055187,18.2443162355879,-2.85333211510684));
#35691=CARTESIAN_POINT('Ctrl Pts',(-39.4154946407658,18.2444140652289,-2.85412375107242));
#35692=CARTESIAN_POINT('Ctrl Pts',(-39.4292658612322,18.247100014769,-2.87585841385372));
#35693=CARTESIAN_POINT('Ctrl Pts',(-39.4430712030152,18.2500743365209,-2.89758076757143));
#35694=CARTESIAN_POINT('Ctrl Pts',(-39.4569074113687,18.253339532556,-2.91929283744107));
#35695=CARTESIAN_POINT('Ctrl Pts',(-39.4571637281578,18.2534000205554,-2.91969505515071));
#35696=CARTESIAN_POINT('Ctrl Pts',(-39.4574200555418,18.2534606083965,-2.92009726933075));
#35697=CARTESIAN_POINT('Ctrl Pts',(-39.4576763935003,18.2535212960994,-2.9204994799941));
#35698=CARTESIAN_POINT('Ctrl Pts',(-39.4645930575922,18.2551588079922,-2.9313521686462));
#35699=CARTESIAN_POINT('Ctrl Pts',(-39.4715174189979,18.2568690247549,-2.9422022947352));
#35700=CARTESIAN_POINT('Ctrl Pts',(-39.4784490768014,18.2586523436986,-2.95305011294296));
#35701=CARTESIAN_POINT('Ctrl Pts',(-39.4785795394355,18.2586859080339,-2.95325428270692));
#35702=CARTESIAN_POINT('Ctrl Pts',(-39.4787100046545,18.2587194982663,-2.95345845165321));
#35703=CARTESIAN_POINT('Ctrl Pts',(-39.4788404724558,18.2587531143986,-2.95366261978354));
#35704=CARTESIAN_POINT('Ctrl Pts',(-39.4823049708794,18.2596457717164,-2.95908418861828));
#35705=CARTESIAN_POINT('Ctrl Pts',(-39.4857712218867,18.2605566737303,-2.96450507496648));
#35706=CARTESIAN_POINT('Ctrl Pts',(-39.489239377884,18.2614859299042,-2.96992562828773));
#35707=CARTESIAN_POINT('Ctrl Pts',(-39.4893061499531,18.2615038207827,-2.97002998967213));
#35708=CARTESIAN_POINT('Ctrl Pts',(-39.4893729221599,18.2615217183572,-2.97013435003213));
#35709=CARTESIAN_POINT('Ctrl Pts',(-39.4894396942678,18.2615396225595,-2.97023870899992));
#35710=CARTESIAN_POINT('Ctrl Pts',(-39.4912071593253,18.2620135487691,-2.97300110238481));
#35711=CARTESIAN_POINT('Ctrl Pts',(-39.4929834237806,18.2624945429552,-2.97577637133006));
#35712=CARTESIAN_POINT('Ctrl Pts',(-39.494737563525,18.2629740863298,-2.97851624630382));
#35713=CARTESIAN_POINT('Ctrl Pts',(-39.4964917032695,18.2634536297045,-2.98125612127759));
#35714=CARTESIAN_POINT('Ctrl Pts',(-39.498245849939,18.2639377205127,-2.98399518950415));
#35715=CARTESIAN_POINT('Ctrl Pts',(-39.5,18.2644264063412,-2.98673344445558));
#35716=CARTESIAN_POINT('',(-42.,18.2644264063412,-2.98673344445559));
#35717=CARTESIAN_POINT('',(-35.3179607461319,18.2644264063412,-2.9867334444556));
#35718=CARTESIAN_POINT('',(-42.,19.2255401693197,-4.54750793782168));
#35719=CARTESIAN_POINT('Origin',(-42.,20.7255401693197,-2.54750793782168));
#35720=CARTESIAN_POINT('',(-41.5,20.7255401693197,-5.04750793782167));
#35721=CARTESIAN_POINT('Ctrl Pts',(-42.,19.2255401693197,-4.54750793782168));
#35722=CARTESIAN_POINT('Ctrl Pts',(-42.,19.4186296086203,-4.6923250172971));
#35723=CARTESIAN_POINT('Ctrl Pts',(-41.9306808358121,19.6671490362798,-4.8239338831961));
#35724=CARTESIAN_POINT('Ctrl Pts',(-41.7602708300839,20.1428670310053,-4.99434388892433));
#35725=CARTESIAN_POINT('Ctrl Pts',(-41.6191747972635,20.4590572214339,-5.04750793782168));
#35726=CARTESIAN_POINT('Ctrl Pts',(-41.5,20.7255401693197,-5.04750793782168));
#35727=CARTESIAN_POINT('',(-38.5,20.7255401693197,-5.04750793782167));
#35728=CARTESIAN_POINT('',(-35.3179607461319,20.7255401693197,-5.04750793782167));
#35729=CARTESIAN_POINT('Origin',(-38.5,20.7255401693197,-2.54750793782168));
#35730=CARTESIAN_POINT('Ctrl Pts',(-38.0645258088056,18.2550018689912,-2.93018339641562));
#35731=CARTESIAN_POINT('Ctrl Pts',(-38.0644730720159,18.2528283685745,-2.91615135985618));
#35732=CARTESIAN_POINT('Ctrl Pts',(-38.0627705408083,18.2507930257081,-2.90221536006827));
#35733=CARTESIAN_POINT('Ctrl Pts',(-38.0559345119105,18.2468879595698,-2.87385547063433));
#35734=CARTESIAN_POINT('Ctrl Pts',(-38.0506165440385,18.2450719281466,-2.85969728188328));
#35735=CARTESIAN_POINT('Ctrl Pts',(-38.0297502918864,18.2401419398439,-2.81872937384456));
#35736=CARTESIAN_POINT('Ctrl Pts',(-38.009731245707,18.2377145869542,-2.7947624867808));
#35737=CARTESIAN_POINT('Ctrl Pts',(-37.9545422712628,18.2334031798558,-2.74749017343037));
#35738=CARTESIAN_POINT('Ctrl Pts',(-37.9142901746769,18.2318218020662,-2.72528538397519));
#35739=CARTESIAN_POINT('Ctrl Pts',(-37.8414545038188,18.2302840973431,-2.70167022451812));
#35740=CARTESIAN_POINT('Ctrl Pts',(-37.8150018767136,18.2299373708106,-2.69576579367227));
#35741=CARTESIAN_POINT('Ctrl Pts',(-37.7751190161242,18.2296160821703,-2.6902187720473));
#35742=CARTESIAN_POINT('Ctrl Pts',(-37.7617249415434,18.229542319151,-2.688912786255));
#35743=CARTESIAN_POINT('Ctrl Pts',(-37.7385545523854,18.2294669900933,-2.68757578997696));
#35744=CARTESIAN_POINT('Ctrl Pts',(-37.7287578120477,18.2294512869825,-2.68729453043002));
#35745=CARTESIAN_POINT('Ctrl Pts',(-37.7186850743359,18.2294512549474,-2.68729395839443));
#35746=CARTESIAN_POINT('Ctrl Pts',(-37.7184052938003,18.2294512668884,-2.68729417161882));
#35747=CARTESIAN_POINT('Ctrl Pts',(-37.7082212513325,18.2294521685178,-2.68731027148849));
#35748=CARTESIAN_POINT('Ctrl Pts',(-37.6982616367749,18.229469077187,-2.68761309404929));
#35749=CARTESIAN_POINT('Ctrl Pts',(-37.6745901668933,18.2295488107686,-2.68902760581585));
#35750=CARTESIAN_POINT('Ctrl Pts',(-37.6608510644345,18.2296269718215,-2.69041058653413));
#35751=CARTESIAN_POINT('Ctrl Pts',(-37.6204173711276,18.2299641651506,-2.69621997972945));
#35752=CARTESIAN_POINT('Ctrl Pts',(-37.593882430355,18.2303230840297,-2.7023106862664));
#35753=CARTESIAN_POINT('Ctrl Pts',(-37.5221982448574,18.2318783259906,-2.72607215467));
#35754=CARTESIAN_POINT('Ctrl Pts',(-37.4820604543081,18.2334561001718,-2.7482132333471));
#35755=CARTESIAN_POINT('Ctrl Pts',(-37.4270061886743,18.2378361403167,-2.79598498835417));
#35756=CARTESIAN_POINT('Ctrl Pts',(-37.4072815134747,18.2402743818913,-2.81993098846459));
#35757=CARTESIAN_POINT('Ctrl Pts',(-37.3868559987021,18.2451921415202,-2.86064392007558));
#35758=CARTESIAN_POINT('Ctrl Pts',(-37.3816847042406,18.2469892393911,-2.87461428212165));
#35759=CARTESIAN_POINT('Ctrl Pts',(-37.3750315800499,18.2508476435117,-2.90258940114771));
#35760=CARTESIAN_POINT('Ctrl Pts',(-37.3733738334646,18.2528576526636,-2.91634041908177));
#35761=CARTESIAN_POINT('Ctrl Pts',(-37.3733218817896,18.2550018784108,-2.9301834572279));
#35762=CARTESIAN_POINT('Origin',(-45.5,34.999999994595,6.55E-10));
#35763=CARTESIAN_POINT('',(-46.,30.499999994595,6.5499944890894E-10));
#35764=CARTESIAN_POINT('Origin',(-46.,34.999999994595,6.55E-10));
#35765=CARTESIAN_POINT('Origin',(-45.5,30.499999994595,6.5499944890894E-10));
#35766=CARTESIAN_POINT('Origin',(-42.5,34.999999994595,6.55E-10));
#35767=CARTESIAN_POINT('',(-42.5,44.7486243140984,-3.90055430318255));
#35768=CARTESIAN_POINT('',(-42.5,39.9429588225849,9.26375507215795));
#35769=CARTESIAN_POINT('Origin',(-42.5,34.999999994595,6.55E-10));
#35770=CARTESIAN_POINT('',(-42.,44.4674750811422,-3.21976947643629));
#35771=CARTESIAN_POINT('Ctrl Pts',(-42.5,44.7486243140985,-3.90055430318255));
#35772=CARTESIAN_POINT('Ctrl Pts',(-42.4544360876625,44.7486243140985,-3.90055430318255));
#35773=CARTESIAN_POINT('Ctrl Pts',(-42.4099205589807,44.7452865463964,-3.8921541598089));
#35774=CARTESIAN_POINT('Ctrl Pts',(-42.3189430447185,44.7318256326699,-3.8584039871009));
#35775=CARTESIAN_POINT('Ctrl Pts',(-42.2748783192192,44.7210296796986,-3.83138728482829));
#35776=CARTESIAN_POINT('Ctrl Pts',(-42.1833702395799,44.6900628273989,-3.75439747859195));
#35777=CARTESIAN_POINT('Ctrl Pts',(-42.1405089721587,44.6680439529169,-3.69999801674033));
#35778=CARTESIAN_POINT('Ctrl Pts',(-42.071269518933,44.6190581603652,-3.58027604363302));
#35779=CARTESIAN_POINT('Ctrl Pts',(-42.0453333388043,44.5914650656171,-3.51348614097825));
#35780=CARTESIAN_POINT('Ctrl Pts',(-42.0094486376468,44.5328201717076,-3.37321530750872));
#35781=CARTESIAN_POINT('Ctrl Pts',(-42.0003510591405,44.5011283734183,-3.29830693481085));
#35782=CARTESIAN_POINT('Ctrl Pts',(-42.0000033224979,44.4687146531266,-3.22266128213935));
#35783=CARTESIAN_POINT('Ctrl Pts',(-42.,44.4680949296128,-3.22121534995777));
#35784=CARTESIAN_POINT('Ctrl Pts',(-42.,44.4674750811422,-3.21976947643629));
#35785=CARTESIAN_POINT('',(-42.,40.1687696585666,8.56059695184988));
#35786=CARTESIAN_POINT('Origin',(-42.,34.999999994595,6.55E-10));
#35787=CARTESIAN_POINT('Ctrl Pts',(-42.,40.1687696585666,8.56059695184987));
#35788=CARTESIAN_POINT('Ctrl Pts',(-42.,40.1683075129929,8.56210529777178));
#35789=CARTESIAN_POINT('Ctrl Pts',(-42.0000033223958,40.1678452330699,8.56361360751137));
#35790=CARTESIAN_POINT('Ctrl Pts',(-42.0003519017721,40.1435951711248,8.64271093468089));
#35791=CARTESIAN_POINT('Ctrl Pts',(-42.0094939504562,40.1192631524652,8.72078571814814));
#35792=CARTESIAN_POINT('Ctrl Pts',(-42.0455618257965,40.0731794932059,8.86646140204777));
#35793=CARTESIAN_POINT('Ctrl Pts',(-42.0716251146577,40.0509849747696,8.93559739857092));
#35794=CARTESIAN_POINT('Ctrl Pts',(-42.1410737799586,40.0109460683308,9.05886941152539));
#35795=CARTESIAN_POINT('Ctrl Pts',(-42.1839363914962,39.9926110365693,9.11460125114772));
#35796=CARTESIAN_POINT('Ctrl Pts',(-42.2753727862073,39.9665354166906,9.1932806146181));
#35797=CARTESIAN_POINT('Ctrl Pts',(-42.3193584730603,39.9573371288592,9.22082690969534));
#35798=CARTESIAN_POINT('Ctrl Pts',(-42.4101445564635,39.9458315569623,9.25520747716902));
#35799=CARTESIAN_POINT('Ctrl Pts',(-42.4545481243919,39.9429588225849,9.26375507215796));
#35800=CARTESIAN_POINT('Ctrl Pts',(-42.5,39.9429588225849,9.26375507215796));
#35801=CARTESIAN_POINT('Origin',(-42.5,34.999999994595,6.55E-10));
#35802=CARTESIAN_POINT('',(-42.,41.2631553534218,-1.7386445723384));
#35803=CARTESIAN_POINT('',(-42.,38.6863865866985,5.35355525801058));
#35804=CARTESIAN_POINT('Origin',(-42.,34.999999994595,6.55E-10));
#35805=CARTESIAN_POINT('',(-42.5,40.65404535889,-2.00792704445741));
#35806=CARTESIAN_POINT('Ctrl Pts',(-42.5,40.65404535889,-2.00792704445741));
#35807=CARTESIAN_POINT('Ctrl Pts',(-42.4826491826238,40.65404535889,-2.00792704445741));
#35808=CARTESIAN_POINT('Ctrl Pts',(-42.4652566053828,40.6551721057398,-2.00745307088224));
#35809=CARTESIAN_POINT('Ctrl Pts',(-42.3984104029602,40.6639091994707,-2.00377454682564));
#35810=CARTESIAN_POINT('Ctrl Pts',(-42.3512786216695,40.6793649916246,-1.99726827466977));
#35811=CARTESIAN_POINT('Ctrl Pts',(-42.2553373204744,40.7290519040805,-1.97619081125632));
#35812=CARTESIAN_POINT('Ctrl Pts',(-42.2093703460395,40.7657123920275,-1.96055718697034));
#35813=CARTESIAN_POINT('Ctrl Pts',(-42.1185333929893,40.86385370113,-1.91818900483338));
#35814=CARTESIAN_POINT('Ctrl Pts',(-42.0788703599454,40.9295917118304,-1.88945413699724));
#35815=CARTESIAN_POINT('Ctrl Pts',(-42.0174426176906,41.0817501876172,-1.82174794014236));
#35816=CARTESIAN_POINT('Ctrl Pts',(-42.0004779950668,41.1710675280286,-1.78124834309648));
#35817=CARTESIAN_POINT('Ctrl Pts',(-42.0000033202246,41.2606497333104,-1.73980423753342));
#35818=CARTESIAN_POINT('Ctrl Pts',(-42.,41.2619025742887,-1.73922446906986));
#35819=CARTESIAN_POINT('Ctrl Pts',(-42.,41.2631553534218,-1.7386445723384));
#35820=CARTESIAN_POINT('',(-42.5,38.0494565603535,5.1672831023974));
#35821=CARTESIAN_POINT('Origin',(-42.5,34.999999994595,6.55E-10));
#35822=CARTESIAN_POINT('Ctrl Pts',(-42.,38.6863865866985,5.35355525801058));
#35823=CARTESIAN_POINT('Ctrl Pts',(-42.,38.6850595270089,5.35319169843818));
#35824=CARTESIAN_POINT('Ctrl Pts',(-42.0000033204919,38.6837325023959,5.35282800249168));
#35825=CARTESIAN_POINT('Ctrl Pts',(-42.0004662363704,38.5912113638028,5.32746066601285));
#35826=CARTESIAN_POINT('Ctrl Pts',(-42.0165992209748,38.4995599069129,5.30160691452096));
#35827=CARTESIAN_POINT('Ctrl Pts',(-42.0758441660175,38.3412349144892,5.25577584370346));
#35828=CARTESIAN_POINT('Ctrl Pts',(-42.1151456113167,38.2718504181019,5.23519478871087));
#35829=CARTESIAN_POINT('Ctrl Pts',(-42.2056695167071,38.1682609648624,5.20395060199156));
#35830=CARTESIAN_POINT('Ctrl Pts',(-42.2516602512676,38.1295569539332,5.1920877752668));
#35831=CARTESIAN_POINT('Ctrl Pts',(-42.3477951889101,38.0769631371526,5.17585630236277));
#35832=CARTESIAN_POINT('Ctrl Pts',(-42.3950686181708,38.0605047528529,5.17072674405129));
#35833=CARTESIAN_POINT('Ctrl Pts',(-42.4631644468274,38.0507635189734,5.16769091110134));
#35834=CARTESIAN_POINT('Ctrl Pts',(-42.4816022135789,38.0494565603535,5.1672831023974));
#35835=CARTESIAN_POINT('Ctrl Pts',(-42.5,38.0494565603535,5.1672831023974));
#35836=CARTESIAN_POINT('Origin',(-46.,34.999999994595,6.54998265276524E-10));
#35837=CARTESIAN_POINT('',(-45.,18.0053133249326,0.425000000655));
#35838=CARTESIAN_POINT('',(-45.,51.6342808642875,-3.50723537042861));
#35839=CARTESIAN_POINT('Origin',(-45.,34.999999994595,6.55E-10));
#35840=CARTESIAN_POINT('',(-45.5,51.6342808642875,-3.50723537042861));
#35841=CARTESIAN_POINT('',(-46.,51.6342808642875,-3.50723537042861));
#35842=CARTESIAN_POINT('',(-45.5,18.0053133249326,0.425000000655));
#35843=CARTESIAN_POINT('Origin',(-45.5,34.999999994595,6.54998265276524E-10));
#35844=CARTESIAN_POINT('',(-46.,18.0053133249326,0.425000000655));
#35845=CARTESIAN_POINT('Origin',(-46.,34.999999994595,6.54998265276524E-10));
#35846=CARTESIAN_POINT('',(-39.5,39.2396510906294,16.4628478279264));
#35847=CARTESIAN_POINT('Origin',(-39.5,34.999999994595,6.54998265276524E-10));
#35848=CARTESIAN_POINT('',(-39.,40.8143424311314,15.9747745540155));
#35849=CARTESIAN_POINT('Ctrl Pts',(-39.5,39.2396510906294,16.4628478279264));
#35850=CARTESIAN_POINT('Ctrl Pts',(-39.4999999961656,39.257290636405,16.4583051436736));
#35851=CARTESIAN_POINT('Ctrl Pts',(-39.4997042609893,39.2749148588005,16.4537361753576));
#35852=CARTESIAN_POINT('Ctrl Pts',(-39.4991310319023,39.2925241298331,16.4491409067449));
#35853=CARTESIAN_POINT('Ctrl Pts',(-39.4991304749569,39.2925412388785,16.4491364420138));
#35854=CARTESIAN_POINT('Ctrl Pts',(-39.4991299177479,39.2925583479326,16.4491319772519));
#35855=CARTESIAN_POINT('Ctrl Pts',(-39.4991293602754,39.2925754569952,16.4491275124591));
#35856=CARTESIAN_POINT('Ctrl Pts',(-39.4985550311578,39.3102018547743,16.44452771556));
#35857=CARTESIAN_POINT('Ctrl Pts',(-39.4977016731233,39.3278275737071,16.4398977782837));
#35858=CARTESIAN_POINT('Ctrl Pts',(-39.4965887044839,39.3454033797105,16.4352508177434));
#35859=CARTESIAN_POINT('Ctrl Pts',(-39.4965870036635,39.3454302387686,16.4352437163346));
#35860=CARTESIAN_POINT('Ctrl Pts',(-39.4965853022347,39.3454570977297,16.4352366148808));
#35861=CARTESIAN_POINT('Ctrl Pts',(-39.4965836001976,39.3454839565936,16.435229513382));
#35862=CARTESIAN_POINT('Ctrl Pts',(-39.4943577725402,39.3806084556226,16.4259425760085));
#35863=CARTESIAN_POINT('Ctrl Pts',(-39.4911025840849,39.41548485882,16.4166008352451));
#35864=CARTESIAN_POINT('Ctrl Pts',(-39.4869518406598,39.4501426751304,16.4072005578185));
#35865=CARTESIAN_POINT('Ctrl Pts',(-39.4869357174425,39.450277300533,16.4071640432234));
#35866=CARTESIAN_POINT('Ctrl Pts',(-39.4869195807133,39.4504119226348,16.4071275277457));
#35867=CARTESIAN_POINT('Ctrl Pts',(-39.4869034304803,39.4505465414377,16.4070910113853));
#35868=CARTESIAN_POINT('Ctrl Pts',(-39.4827323057594,39.4853145731815,16.3976599218938));
#35869=CARTESIAN_POINT('Ctrl Pts',(-39.4776595176198,39.5198623488115,16.3881699877856));
#35870=CARTESIAN_POINT('Ctrl Pts',(-39.4717924919497,39.5542134049,16.3786183860195));
#35871=CARTESIAN_POINT('Ctrl Pts',(-39.4659770096339,39.5882626779798,16.369150697572));
#35872=CARTESIAN_POINT('Ctrl Pts',(-39.4593806799903,39.6221185586476,16.3596224420949));
#35873=CARTESIAN_POINT('Ctrl Pts',(-39.4520904807254,39.6557999053799,16.3500314131952));
#35874=CARTESIAN_POINT('Ctrl Pts',(-39.4520300985524,39.656078876205,16.3499519740544));
#35875=CARTESIAN_POINT('Ctrl Pts',(-39.4519696687774,39.6563578350588,16.3498725306069));
#35876=CARTESIAN_POINT('Ctrl Pts',(-39.4519091914498,39.6566367819523,16.3497930828512));
#35877=CARTESIAN_POINT('Ctrl Pts',(-39.4372730555425,39.724144802027,16.3305659080398));
#35878=CARTESIAN_POINT('Ctrl Pts',(-39.4198586838727,39.7909539305682,16.3110863403623));
#35879=CARTESIAN_POINT('Ctrl Pts',(-39.4002375988986,39.8571885237601,16.2913387913687));
#35880=CARTESIAN_POINT('Ctrl Pts',(-39.4001338742578,39.8575386654262,16.2912343981903));
#35881=CARTESIAN_POINT('Ctrl Pts',(-39.4000300879518,39.8578887910394,16.2911299975231));
#35882=CARTESIAN_POINT('Ctrl Pts',(-39.3999262400651,39.8582389006182,16.2910255893649));
#35883=CARTESIAN_POINT('Ctrl Pts',(-39.38030451741,39.9243909743711,16.2712980052008));
#35884=CARTESIAN_POINT('Ctrl Pts',(-39.3584791470918,39.9899694404819,16.2513031922256));
#35885=CARTESIAN_POINT('Ctrl Pts',(-39.3349302503083,40.0550779956201,16.2310254274449));
#35886=CARTESIAN_POINT('Ctrl Pts',(-39.3347975544398,40.0554448763429,16.2309111641045));
#35887=CARTESIAN_POINT('Ctrl Pts',(-39.3346648036945,40.0558117425731,16.2307968916474));
#35888=CARTESIAN_POINT('Ctrl Pts',(-39.3345319981584,40.0561785943288,16.2306826100709));
#35889=CARTESIAN_POINT('Ctrl Pts',(-39.3109717092849,40.1212597166307,16.210408553474));
#35890=CARTESIAN_POINT('Ctrl Pts',(-39.2858005512003,40.1855728622067,16.1899451074169));
#35891=CARTESIAN_POINT('Ctrl Pts',(-39.2594627711653,40.2492934160747,16.1692584430621));
#35892=CARTESIAN_POINT('Ctrl Pts',(-39.2593270376094,40.2496218043196,16.1691518329185));
#35893=CARTESIAN_POINT('Ctrl Pts',(-39.2591912730754,40.2499501768249,16.1690452168479));
#35894=CARTESIAN_POINT('Ctrl Pts',(-39.2590554776243,40.2502785336145,16.1689385948457));
#35895=CARTESIAN_POINT('Ctrl Pts',(-39.2326929533815,40.3140237751508,16.1482396311102));
#35896=CARTESIAN_POINT('Ctrl Pts',(-39.205162121713,40.3771784216706,16.1273164564048));
#35897=CARTESIAN_POINT('Ctrl Pts',(-39.1768657258588,40.4399066591195,16.1061297493681));
#35898=CARTESIAN_POINT('Ctrl Pts',(-39.1767555231826,40.4401509594776,16.1060472359686));
#35899=CARTESIAN_POINT('Ctrl Pts',(-39.1766453088967,40.44039525337,16.1059647185719));
#35900=CARTESIAN_POINT('Ctrl Pts',(-39.1765350830249,40.4406395408063,16.1058821971757));
#35901=CARTESIAN_POINT('Ctrl Pts',(-39.1481971695223,40.5034432739673,16.0846668132485));
#35902=CARTESIAN_POINT('Ctrl Pts',(-39.1190922361285,40.5658197445189,16.0631871765129));
#35903=CARTESIAN_POINT('Ctrl Pts',(-39.0896053781452,40.6279237128273,16.0413987745173));
#35904=CARTESIAN_POINT('Ctrl Pts',(-39.0895425553902,40.6280560274464,16.041352353585));
#35905=CARTESIAN_POINT('Ctrl Pts',(-39.0894797309058,40.6281883408303,16.0413059312506));
#35906=CARTESIAN_POINT('Ctrl Pts',(-39.0894169046956,40.6283206529806,16.0412595075139));
#35907=CARTESIAN_POINT('Ctrl Pts',(-39.0746781404176,40.6593605261092,16.0303686944148));
#35908=CARTESIAN_POINT('Ctrl Pts',(-39.0598441294354,40.6903323484342,16.0194006149621));
#35909=CARTESIAN_POINT('Ctrl Pts',(-39.0449619049029,40.7212548030359,16.0083491790342));
#35910=CARTESIAN_POINT('Ctrl Pts',(-39.0449279153316,40.7213254269518,16.0083239386162));
#35911=CARTESIAN_POINT('Ctrl Pts',(-39.044893925509,40.7213960506103,16.0082986977632));
#35912=CARTESIAN_POINT('Ctrl Pts',(-39.0448599354357,40.7214666740117,16.0082734564755));
#35913=CARTESIAN_POINT('Ctrl Pts',(-39.0374209839921,40.7369230705795,16.0027492343792));
#35914=CARTESIAN_POINT('Ctrl Pts',(-39.0299700122027,40.7523671405465,15.9972041756753));
#35915=CARTESIAN_POINT('Ctrl Pts',(-39.0225129137083,40.7678012106761,15.9916374756535));
#35916=CARTESIAN_POINT('Ctrl Pts',(-39.0224940110446,40.7678403338065,15.9916233648759));
#35917=CARTESIAN_POINT('Ctrl Pts',(-39.0224751082747,40.7678794570111,15.9916092539093));
#35918=CARTESIAN_POINT('Ctrl Pts',(-39.0224562053995,40.7679185802883,15.9915951427543));
#35919=CARTESIAN_POINT('Ctrl Pts',(-39.0187294806157,40.7756317818559,15.9888131114259));
#35920=CARTESIAN_POINT('Ctrl Pts',(-39.0150012674768,40.783342378541,15.9860257341351));
#35921=CARTESIAN_POINT('Ctrl Pts',(-39.0112722413038,40.7910508186585,15.9832328093444));
#35922=CARTESIAN_POINT('Ctrl Pts',(-39.009398270943,40.7949245882802,15.9818292637443));
#35923=CARTESIAN_POINT('Ctrl Pts',(-39.0075241022877,40.7987978000274,15.9804243232044));
#35924=CARTESIAN_POINT('Ctrl Pts',(-39.0056498316341,40.8026704927234,15.979017976295));
#35925=CARTESIAN_POINT('Ctrl Pts',(-39.0047126963073,40.8046068390714,15.9783148028403));
#35926=CARTESIAN_POINT('Ctrl Pts',(-39.0037735239429,40.8065472120575,15.9776097691188));
#35927=CARTESIAN_POINT('Ctrl Pts',(-39.0028301473931,40.8084961158097,15.9769012314385));
#35928=CARTESIAN_POINT('Ctrl Pts',(-39.0018867708432,40.8104450195619,15.9761926937581));
#35929=CARTESIAN_POINT('Ctrl Pts',(-39.000943384461,40.812393789486,15.9754838015716));
#35930=CARTESIAN_POINT('Ctrl Pts',(-39.,40.8143424311314,15.9747745540155));
#35931=CARTESIAN_POINT('',(-39.5,42.3343534352395,15.3364682905745));
#35932=CARTESIAN_POINT('Ctrl Pts',(-39.,40.8143424311314,15.9747745540155));
#35933=CARTESIAN_POINT('Ctrl Pts',(-39.0009433844611,40.8162910727767,15.9740653064594));
#35934=CARTESIAN_POINT('Ctrl Pts',(-39.0018867708433,40.8182395842621,15.9733557042182));
#35935=CARTESIAN_POINT('Ctrl Pts',(-39.002830147393,40.8201879703936,15.9726457443865));
#35936=CARTESIAN_POINT('Ctrl Pts',(-39.0037735239428,40.8221363565251,15.9719357845549));
#35937=CARTESIAN_POINT('Ctrl Pts',(-39.004712696307,40.8240759554092,15.9712286240058));
#35938=CARTESIAN_POINT('Ctrl Pts',(-39.0056498316338,40.8260112739532,15.9705226266828));
#35939=CARTESIAN_POINT('Ctrl Pts',(-39.0075241022874,40.8298819110412,15.9691106320367));
#35940=CARTESIAN_POINT('Ctrl Pts',(-39.0093982709428,40.8337520417486,15.9676972264094));
#35941=CARTESIAN_POINT('Ctrl Pts',(-39.0112722413036,40.8376217031625,15.9662823936014));
#35942=CARTESIAN_POINT('Ctrl Pts',(-39.0150012674767,40.8453219683299,15.9634670083199));
#35943=CARTESIAN_POINT('Ctrl Pts',(-39.0187294806157,40.8530203196596,15.9606459871919));
#35944=CARTESIAN_POINT('Ctrl Pts',(-39.0224562053995,40.8607172301268,15.957819196433));
#35945=CARTESIAN_POINT('Ctrl Pts',(-39.0224751082747,40.8607562707715,15.957804858247));
#35946=CARTESIAN_POINT('Ctrl Pts',(-39.0224940110446,40.8607953112395,15.9577905199634));
#35947=CARTESIAN_POINT('Ctrl Pts',(-39.0225129137083,40.8608343515291,15.9577761815826));
#35948=CARTESIAN_POINT('Ctrl Pts',(-39.0299700122027,40.8762357409875,15.9521196921546));
#35949=CARTESIAN_POINT('Ctrl Pts',(-39.0374209839922,40.8916308799947,15.9464401967435));
#35950=CARTESIAN_POINT('Ctrl Pts',(-39.0448599354357,40.9070220682127,15.9407368161787));
#35951=CARTESIAN_POINT('Ctrl Pts',(-39.0448939255091,40.9070923936639,15.9407107562796));
#35952=CARTESIAN_POINT('Ctrl Pts',(-39.0449279153317,40.9071627190326,15.9406846958821));
#35953=CARTESIAN_POINT('Ctrl Pts',(-39.0449619049029,40.907233044319,15.9406586349859));
#35954=CARTESIAN_POINT('Ctrl Pts',(-39.0598441294354,40.9380247449178,15.9292479553879));
#35955=CARTESIAN_POINT('Ctrl Pts',(-39.0746781404176,40.9688006828774,15.9177416880645));
#35956=CARTESIAN_POINT('Ctrl Pts',(-39.0894169046956,40.9995790849222,15.9061324890668));
#35957=CARTESIAN_POINT('Ctrl Pts',(-39.0894797309058,40.9997102825124,15.9060830031016));
#35958=CARTESIAN_POINT('Ctrl Pts',(-39.0895425553903,40.9998414801463,15.906033515269));
#35959=CARTESIAN_POINT('Ctrl Pts',(-39.0896053781452,40.9999726778251,15.9059840255685));
#35960=CARTESIAN_POINT('Ctrl Pts',(-39.1190922361287,41.061552392481,15.8827552485007));
#35961=CARTESIAN_POINT('Ctrl Pts',(-39.1481971695226,41.1231423854826,15.8591147824557));
#35962=CARTESIAN_POINT('Ctrl Pts',(-39.1765350830251,41.1848898222009,15.8349972479038));
#35963=CARTESIAN_POINT('Ctrl Pts',(-39.1766453088969,41.185130000965,15.8349034380236));
#35964=CARTESIAN_POINT('Ctrl Pts',(-39.1767555231828,41.1853701821039,15.8348096209297));
#35965=CARTESIAN_POINT('Ctrl Pts',(-39.176865725859,41.1856103656265,15.8347157966176));
#35966=CARTESIAN_POINT('Ctrl Pts',(-39.205162121713,41.2472815361242,15.8106248220014));
#35967=CARTESIAN_POINT('Ctrl Pts',(-39.2326929533814,41.3091099596038,15.7860578794398));
#35968=CARTESIAN_POINT('Ctrl Pts',(-39.2590554776243,41.3712466850805,15.7609395541517));
#35969=CARTESIAN_POINT('Ctrl Pts',(-39.2591912730753,41.3715667562765,15.760810167668));
#35970=CARTESIAN_POINT('Ctrl Pts',(-39.2593270376093,41.3718868356986,15.7606807665387));
#35971=CARTESIAN_POINT('Ctrl Pts',(-39.2594627711653,41.3722069233682,15.7605513507518));
#35972=CARTESIAN_POINT('Ctrl Pts',(-39.2858005512002,41.4343168311042,15.7354394725188));
#35973=CARTESIAN_POINT('Ctrl Pts',(-39.3109717092848,41.4967372084691,15.7097756885417));
#35974=CARTESIAN_POINT('Ctrl Pts',(-39.3345319981583,41.5596241529389,15.683473177897));
#35975=CARTESIAN_POINT('Ctrl Pts',(-39.3346648036944,41.5599786364693,15.6833249149005));
#35976=CARTESIAN_POINT('Ctrl Pts',(-39.3347975544398,41.560333125226,15.683176635614));
#35977=CARTESIAN_POINT('Ctrl Pts',(-39.3349302503083,41.5606876192244,15.6830283400282));
#35978=CARTESIAN_POINT('Ctrl Pts',(-39.3584791470918,41.6235979620406,15.6567110365299));
#35979=CARTESIAN_POINT('Ctrl Pts',(-39.3803045174101,41.6866863996315,15.6298749264226));
#35980=CARTESIAN_POINT('Ctrl Pts',(-39.3999262400652,41.7500424748004,15.6024653992843));
#35981=CARTESIAN_POINT('Ctrl Pts',(-39.4000300879518,41.7503777865682,15.6023203344744));
#35982=CARTESIAN_POINT('Ctrl Pts',(-39.4001338742579,41.7507131058039,15.6021752536193));
#35983=CARTESIAN_POINT('Ctrl Pts',(-39.4002375988987,41.7510484325233,15.6020301567089));
#35984=CARTESIAN_POINT('Ctrl Pts',(-39.4198586838727,41.8144805543948,15.5745828810443));
#35985=CARTESIAN_POINT('Ctrl Pts',(-39.4372730555425,41.8781805408086,15.5465610155777));
#35986=CARTESIAN_POINT('Ctrl Pts',(-39.4519091914498,41.9422536741908,15.5178965671404));
#35987=CARTESIAN_POINT('Ctrl Pts',(-39.4519696687774,41.9425184279414,15.5177781240452));
#35988=CARTESIAN_POINT('Ctrl Pts',(-39.4520300985524,41.9427831880851,15.5176596699619));
#35989=CARTESIAN_POINT('Ctrl Pts',(-39.4520904807254,41.9430479546309,15.5175412048844));
#35990=CARTESIAN_POINT('Ctrl Pts',(-39.4593806799903,41.9750143576728,15.5032384069197));
#35991=CARTESIAN_POINT('Ctrl Pts',(-39.465977009634,42.0070741114877,15.4887753334725));
#35992=CARTESIAN_POINT('Ctrl Pts',(-39.4717924919497,42.0392430807491,15.4741415527422));
#35993=CARTESIAN_POINT('Ctrl Pts',(-39.4776595176198,42.071697167649,15.4593780709647));
#35994=CARTESIAN_POINT('Ctrl Pts',(-39.4827323057594,42.1042623112539,15.4444409001366));
#35995=CARTESIAN_POINT('Ctrl Pts',(-39.4869034304802,42.1369583562403,15.4293170738161));
#35996=CARTESIAN_POINT('Ctrl Pts',(-39.4869195807133,42.1370849524904,15.4292585156725));
#35997=CARTESIAN_POINT('Ctrl Pts',(-39.4869357174425,42.1372115507001,15.4291999547321));
#35998=CARTESIAN_POINT('Ctrl Pts',(-39.4869518406598,42.137338150871,15.4291413909941));
#35999=CARTESIAN_POINT('Ctrl Pts',(-39.4911025840849,42.1699299603236,15.4140648063774));
#36000=CARTESIAN_POINT('Ctrl Pts',(-39.4943577725402,42.2026515904045,15.3988028751326));
#36001=CARTESIAN_POINT('Ctrl Pts',(-39.4965836001976,42.2355280459786,15.383339489129));
#36002=CARTESIAN_POINT('Ctrl Pts',(-39.4965853022347,42.2355531858175,15.3833276646477));
#36003=CARTESIAN_POINT('Ctrl Pts',(-39.4965870036635,42.235578325702,15.3833158400695));
#36004=CARTESIAN_POINT('Ctrl Pts',(-39.4965887044839,42.2356034656319,15.3833040153944));
#36005=CARTESIAN_POINT('Ctrl Pts',(-39.4977016731233,42.2520543228121,15.3755662833645));
#36006=CARTESIAN_POINT('Ctrl Pts',(-39.4985550311578,42.2685324731713,15.3677834273452));
#36007=CARTESIAN_POINT('Ctrl Pts',(-39.4991293602754,42.284991769696,15.3599770461034));
#36008=CARTESIAN_POINT('Ctrl Pts',(-39.4991299177479,42.2850077459118,15.3599694688396));
#36009=CARTESIAN_POINT('Ctrl Pts',(-39.4991304749569,42.2850237221012,15.3599618915577));
#36010=CARTESIAN_POINT('Ctrl Pts',(-39.4991310319023,42.2850396982641,15.3599543142578));
#36011=CARTESIAN_POINT('Ctrl Pts',(-39.4997042609893,42.3014829642135,15.3521554730077));
#36012=CARTESIAN_POINT('Ctrl Pts',(-39.4999999961656,42.3179207780666,15.3443268740108));
#36013=CARTESIAN_POINT('Ctrl Pts',(-39.5,42.3343534352395,15.3364682905744));
#36014=CARTESIAN_POINT('',(-39.5000000131726,51.3840964769944,4.53446620038969));
#36015=CARTESIAN_POINT('Origin',(-39.5,34.999999994595,6.54998265276524E-10));
#36016=CARTESIAN_POINT('',(-39.0362682345593,51.6364368368602,3.49699430910377));
#36017=CARTESIAN_POINT('Ctrl Pts',(-39.5,51.3840964378613,4.5344662027289));
#36018=CARTESIAN_POINT('Ctrl Pts',(-39.4968435532909,51.3872502998287,4.52307055518404));
#36019=CARTESIAN_POINT('Ctrl Pts',(-39.4936766092617,51.3903962860629,4.51165705063485));
#36020=CARTESIAN_POINT('Ctrl Pts',(-39.4904960460761,51.3935276966917,4.50024993600152));
#36021=CARTESIAN_POINT('Ctrl Pts',(-39.4873154828905,51.3966591073206,4.48884282136819));
#36022=CARTESIAN_POINT('Ctrl Pts',(-39.4841222891727,51.3997773936769,4.47743687379982));
#36023=CARTESIAN_POINT('Ctrl Pts',(-39.4809141689974,51.4028823781766,4.46603286107936));
#36024=CARTESIAN_POINT('Ctrl Pts',(-39.4744979286469,51.4090923471758,4.44322483563845));
#36025=CARTESIAN_POINT('Ctrl Pts',(-39.4680219824665,51.4152491017619,4.42042454768003));
#36026=CARTESIAN_POINT('Ctrl Pts',(-39.4614661068467,51.4213511333313,4.39763877371537));
#36027=CARTESIAN_POINT('Ctrl Pts',(-39.448354355607,51.4335551964702,4.35206722578608));
#36028=CARTESIAN_POINT('Ctrl Pts',(-39.4349262143165,51.4455405254189,4.30655259604968));
#36029=CARTESIAN_POINT('Ctrl Pts',(-39.4209875904999,51.4572936361253,4.26116017089597));
#36030=CARTESIAN_POINT('Ctrl Pts',(-39.4070489666834,51.4690467468316,4.21576774574225));
#36031=CARTESIAN_POINT('Ctrl Pts',(-39.3926019608065,51.4805677623338,4.17049681288467));
#36032=CARTESIAN_POINT('Ctrl Pts',(-39.3773863627455,51.4918399213891,4.12543522969451));
#36033=CARTESIAN_POINT('Ctrl Pts',(-39.3621707646845,51.5031120804444,4.08037364650435));
#36034=CARTESIAN_POINT('Ctrl Pts',(-39.3461896001512,51.5141355464633,4.0355203834572));
#36035=CARTESIAN_POINT('Ctrl Pts',(-39.329078342351,51.524888139763,3.99099884676946));
#36036=CARTESIAN_POINT('Ctrl Pts',(-39.3119670845507,51.5356407330627,3.94647731008172));
#36037=CARTESIAN_POINT('Ctrl Pts',(-39.2937299545982,51.546122664982,3.90228605929807));
#36038=CARTESIAN_POINT('Ctrl Pts',(-39.2738440874327,51.5563035390082,3.85860246077594));
#36039=CARTESIAN_POINT('Ctrl Pts',(-39.2639011538499,51.5613939760213,3.83676066151488));
#36040=CARTESIAN_POINT('Ctrl Pts',(-39.2535431996943,51.5664090022314,3.81504674210773));
#36041=CARTESIAN_POINT('Ctrl Pts',(-39.2426841573976,51.5713437578886,3.79348993457491));
#36042=CARTESIAN_POINT('Ctrl Pts',(-39.2372546362493,51.5738111357172,3.7827115308085));
#36043=CARTESIAN_POINT('Ctrl Pts',(-39.2316948510857,51.5762604415035,3.77196362852963));
#36044=CARTESIAN_POINT('Ctrl Pts',(-39.2260082601485,51.5786842720526,3.76128005249661));
#36045=CARTESIAN_POINT('Ctrl Pts',(-39.2203216692112,51.5811081026017,3.75059647646359));
#36046=CARTESIAN_POINT('Ctrl Pts',(-39.2145161338205,51.5835032245596,3.73999156307459));
#36047=CARTESIAN_POINT('Ctrl Pts',(-39.2085825697722,51.5858687263796,3.7294716002265));
#36048=CARTESIAN_POINT('Ctrl Pts',(-39.1848483135789,51.5953307336594,3.68739174883414));
#36049=CARTESIAN_POINT('Ctrl Pts',(-39.1590761421985,51.6043196023881,3.64666374823141));
#36050=CARTESIAN_POINT('Ctrl Pts',(-39.1306063976789,51.612771528083,3.60774472224096));
#36051=CARTESIAN_POINT('Ctrl Pts',(-39.1163715254191,51.6169974909304,3.58828520924573));
#36052=CARTESIAN_POINT('Ctrl Pts',(-39.1014603874055,51.6210890945102,3.56927925006868));
#36053=CARTESIAN_POINT('Ctrl Pts',(-39.0857737045518,51.6250368411351,3.55079566517632));
#36054=CARTESIAN_POINT('Ctrl Pts',(-39.0700870216981,51.6289845877601,3.53231208028396));
#36055=CARTESIAN_POINT('Ctrl Pts',(-39.0536247940042,51.632788472119,3.51435086854871));
#36056=CARTESIAN_POINT('Ctrl Pts',(-39.0362682345593,51.6364368368601,3.49699430910376));
#36057=CARTESIAN_POINT('',(-36.5,51.9728313851128,0.960726074544506));
#36058=CARTESIAN_POINT('Origin',(-35.5392739279158,35.0000000067947,2.46239528767234E-9));
#36059=CARTESIAN_POINT('',(-39.9010326004531,51.9728313851128,0.960726074544506));
#36060=CARTESIAN_POINT('',(-46.,51.9728313851128,0.960726074544506));
#36061=CARTESIAN_POINT('',(-40.9999916854184,51.9933713732604,0.474687473337844));
#36062=CARTESIAN_POINT('Ctrl Pts',(-39.9010326004531,51.9728313851129,0.960726074543242));
#36063=CARTESIAN_POINT('Ctrl Pts',(-39.9978786264107,51.9728313941464,0.960725914951945));
#36064=CARTESIAN_POINT('Ctrl Pts',(-40.0944034219574,51.9736959398618,0.945675215530035));
#36065=CARTESIAN_POINT('Ctrl Pts',(-40.2911429224183,51.976606028045,0.891986910632592));
#36066=CARTESIAN_POINT('Ctrl Pts',(-40.3906299377519,51.9787441069525,0.851223271414997));
#36067=CARTESIAN_POINT('Ctrl Pts',(-40.6662405913416,51.9853228295072,0.71209955870285));
#36068=CARTESIAN_POINT('Ctrl Pts',(-40.8325948331438,51.9899804626179,0.595396525128735));
#36069=CARTESIAN_POINT('Ctrl Pts',(-40.9974247789548,51.993320696534,0.476500092965129));
#36070=CARTESIAN_POINT('Ctrl Pts',(-40.9980817464721,51.9933332259892,0.476051023380418));
#36071=CARTESIAN_POINT('Ctrl Pts',(-40.9999833699879,51.9933713149156,0.474687475140312));
#36072=CARTESIAN_POINT('',(-41.,51.6274934940962,-3.5392739254555));
#36073=CARTESIAN_POINT('Origin',(-41.,34.999999994595,6.54998265276524E-10));
#36074=CARTESIAN_POINT('',(-39.,51.6274934940962,-3.5392739254555));
#36075=CARTESIAN_POINT('',(-46.,51.6274934940962,-3.5392739254555));
#36076=CARTESIAN_POINT('',(-39.,51.5380870962865,-3.93594652043317));
#36077=CARTESIAN_POINT('Origin',(-39.,34.999999994595,6.54998265276524E-10));
#36078=CARTESIAN_POINT('',(-42.,51.5380870962865,-3.93594652043317));
#36079=CARTESIAN_POINT('',(-42.5,51.5380870962865,-3.93594652043317));
#36080=CARTESIAN_POINT('Origin',(-42.,34.999999994595,6.55E-10));
#36081=CARTESIAN_POINT('Origin',(-45.5,48.5946168001447,-6.3392739254555));
#36082=CARTESIAN_POINT('',(-45.5,51.536059602328,-8.74508236369084));
#36083=CARTESIAN_POINT('Ctrl Pts',(-45.5,51.536059602328,-8.74508236369081));
#36084=CARTESIAN_POINT('Ctrl Pts',(-45.5610099545588,51.536059602328,-8.74508236369081));
#36085=CARTESIAN_POINT('Ctrl Pts',(-45.6327520230047,51.5228098390117,-8.73895795786099));
#36086=CARTESIAN_POINT('Ctrl Pts',(-45.7461170544744,51.4793988730731,-8.71889221279613));
#36087=CARTESIAN_POINT('Ctrl Pts',(-45.807537611249,51.4412292854533,-8.70124917726702));
#36088=CARTESIAN_POINT('Ctrl Pts',(-45.8953862936685,51.359854656071,-8.66363558050352));
#36089=CARTESIAN_POINT('Ctrl Pts',(-45.9369188502267,51.3018827723886,-8.63683937789094));
#36090=CARTESIAN_POINT('Ctrl Pts',(-45.9852418633363,51.193700420265,-8.58683451273094));
#36091=CARTESIAN_POINT('Ctrl Pts',(-46.,51.1240450977077,-8.5546379026205));
#36092=CARTESIAN_POINT('Ctrl Pts',(-46.,51.0054363441836,-8.49981366733315));
#36093=CARTESIAN_POINT('Ctrl Pts',(-45.9850887852051,50.9353323591387,-8.46740967305372));
#36094=CARTESIAN_POINT('Ctrl Pts',(-45.9365990223064,50.8258060489551,-8.41678359343263));
#36095=CARTESIAN_POINT('Ctrl Pts',(-45.8947712520246,50.7667016000801,-8.3894638879693));
#36096=CARTESIAN_POINT('Ctrl Pts',(-45.8065209977524,50.6837579493857,-8.35112504630582));
#36097=CARTESIAN_POINT('Ctrl Pts',(-45.7450048833574,50.644733012828,-8.3330866449202));
#36098=CARTESIAN_POINT('Ctrl Pts',(-45.6318339315503,50.6006225310584,-8.31269756435638));
#36099=CARTESIAN_POINT('Ctrl Pts',(-45.5606209586284,50.5871414377259,-8.30646623141648));
#36100=CARTESIAN_POINT('Ctrl Pts',(-45.5,50.5871414377259,-8.30646623141648));
#36101=CARTESIAN_POINT('',(-45.5,44.9368005344369,-5.30952630282035));
#36102=CARTESIAN_POINT('Origin',(-45.5,48.5946168001447,-6.3392739254555));
#36103=CARTESIAN_POINT('',(-46.,45.5585549887889,-5.04608844857037));
#36104=CARTESIAN_POINT('Ctrl Pts',(-46.,45.5585549887888,-5.04608844857035));
#36105=CARTESIAN_POINT('Ctrl Pts',(-46.,45.5571993022191,-5.04661049288134));
#36106=CARTESIAN_POINT('Ctrl Pts',(-45.9999967384478,45.5558437328877,-5.04713284993456));
#36107=CARTESIAN_POINT('Ctrl Pts',(-45.9996861771746,45.4913559119876,-5.07199968453559));
#36108=CARTESIAN_POINT('Ctrl Pts',(-45.9922970303438,45.4282529161658,-5.09712381602786));
#36109=CARTESIAN_POINT('Ctrl Pts',(-45.9628850855617,45.3094004254328,-5.14578236294185));
#36110=CARTESIAN_POINT('Ctrl Pts',(-45.9415281874646,45.2530369118137,-5.16949794189751));
#36111=CARTESIAN_POINT('Ctrl Pts',(-45.880111346903,45.1423569962183,-5.21706799128967));
#36112=CARTESIAN_POINT('Ctrl Pts',(-45.8380939739815,45.0887664804345,-5.24073487943443));
#36113=CARTESIAN_POINT('Ctrl Pts',(-45.7448590805052,45.0100882393425,-5.27600141359422));
#36114=CARTESIAN_POINT('Ctrl Pts',(-45.6978771986565,44.9818172501111,-5.28888307601759));
#36115=CARTESIAN_POINT('Ctrl Pts',(-45.5993681166238,44.9458077969971,-5.30536483849589));
#36116=CARTESIAN_POINT('Ctrl Pts',(-45.5501909035189,44.9368005344368,-5.30952630282034));
#36117=CARTESIAN_POINT('Ctrl Pts',(-45.5,44.9368005344368,-5.30952630282034));
#36118=CARTESIAN_POINT('',(-46.,51.3570957323555,-4.53408414344039));
#36119=CARTESIAN_POINT('Origin',(-46.,48.5946168001447,-6.3392739254555));
#36120=CARTESIAN_POINT('',(-46.,51.8936061016832,-6.25760637783006));
#36121=CARTESIAN_POINT('Origin',(-46.,48.5946168001447,-6.3392739254555));
#36122=CARTESIAN_POINT('Ctrl Pts',(-46.,51.8936061016832,-6.25760637783005));
#36123=CARTESIAN_POINT('Ctrl Pts',(-46.,51.8446981440034,-6.29759574004589));
#36124=CARTESIAN_POINT('Ctrl Pts',(-45.9925616565093,51.7945463220741,-6.33085249730313));
#36125=CARTESIAN_POINT('Ctrl Pts',(-45.9600599922931,51.6903418761989,-6.38858294994055));
#36126=CARTESIAN_POINT('Ctrl Pts',(-45.9330606613793,51.6362874460005,-6.41168372569964));
#36127=CARTESIAN_POINT('Ctrl Pts',(-45.8593582686235,51.5403124425339,-6.44478611383869));
#36128=CARTESIAN_POINT('Ctrl Pts',(-45.8153923054053,51.4997330114652,-6.45498930021723));
#36129=CARTESIAN_POINT('Ctrl Pts',(-45.7122950951514,51.4348321270486,-6.46872532783377));
#36130=CARTESIAN_POINT('Ctrl Pts',(-45.6542008350173,51.4118321455977,-6.47201663128939));
#36131=CARTESIAN_POINT('Ctrl Pts',(-45.5624520001501,51.394281159716,-6.47449009821175));
#36132=CARTESIAN_POINT('Ctrl Pts',(-45.5312249071534,51.3913318198146,-6.47486558726599));
#36133=CARTESIAN_POINT('Ctrl Pts',(-45.5,51.3913318198146,-6.47486558726599));
#36134=CARTESIAN_POINT('Origin',(-33.5,53.0946168001448,0.460726074544506));
#36135=CARTESIAN_POINT('',(-33.5,49.0946168001448,0.960726074544506));
#36136=CARTESIAN_POINT('',(-33.5,57.0946168001448,0.960726074544506));
#36137=CARTESIAN_POINT('Origin',(-33.5,53.0946168001448,0.960726074544506));
#36138=CARTESIAN_POINT('',(-33.5,48.5946168001447,0.460726074544507));
#36139=CARTESIAN_POINT('Origin',(-33.5,49.0946168001448,0.460726074544506));
#36140=CARTESIAN_POINT('',(-33.5,57.5946168001448,0.460726074544506));
#36141=CARTESIAN_POINT('Origin',(-33.5,53.0946168001448,0.460726074544507));
#36142=CARTESIAN_POINT('Origin',(-33.5,57.0946168001448,0.460726074544506));
#36143=CARTESIAN_POINT('Origin',(-30.,20.7255401693197,-2.54750793782168));
#36144=CARTESIAN_POINT('',(-29.,22.2255401693197,-2.54750793782168));
#36145=CARTESIAN_POINT('Origin',(-30.,22.2255401693197,-2.54750793782168));
#36146=CARTESIAN_POINT('Origin',(-29.,20.7255401693197,-2.54750793782168));
#36147=CARTESIAN_POINT('Origin',(-33.5,53.0946168001448,-7.02582898583051));
#36148=CARTESIAN_POINT('',(-32.,53.0946168001448,0.960726074544506));
#36149=CARTESIAN_POINT('Origin',(-33.5,53.0946168001448,0.960726074544506));
#36150=CARTESIAN_POINT('',(-32.,53.0946168001448,-3.5392739254555));
#36151=CARTESIAN_POINT('',(-32.,53.0946168001448,-7.02582898583051));
#36152=CARTESIAN_POINT('Origin',(-33.5,53.0946168001448,-3.5392739254555));
#36153=CARTESIAN_POINT('Origin',(-39.,48.5946168001447,-6.3392739254555));
#36154=CARTESIAN_POINT('',(-42.,51.508884771774,-8.77792974158369));
#36155=CARTESIAN_POINT('Origin',(-42.,48.5946168001447,-6.3392739254555));
#36156=CARTESIAN_POINT('',(-39.,45.925692710035,-9.04424050588343));
#36157=CARTESIAN_POINT('Origin',(-39.,48.5946168001447,-6.3392739254555));
#36158=CARTESIAN_POINT('',(-40.9828862029043,45.925692710035,-9.04424050588343));
#36159=CARTESIAN_POINT('',(-35.3179607461319,45.925692710035,-9.04424050588343));
#36160=CARTESIAN_POINT('',(-42.5,45.3322472608192,-8.28784904304297));
#36161=CARTESIAN_POINT('Ctrl Pts',(-40.9828862029043,45.9256927107335,-9.04424050517556));
#36162=CARTESIAN_POINT('Ctrl Pts',(-41.0173448936212,45.9443390811737,-9.06263841535526));
#36163=CARTESIAN_POINT('Ctrl Pts',(-41.053116758968,45.9615485000311,-9.07923938046472));
#36164=CARTESIAN_POINT('Ctrl Pts',(-41.0903148592313,45.9770857982912,-9.09400285120051));
#36165=CARTESIAN_POINT('Ctrl Pts',(-41.093443851758,45.9783927491784,-9.09524471003936));
#36166=CARTESIAN_POINT('Ctrl Pts',(-41.0965829780637,45.9796878314774,-9.09647352116651));
#36167=CARTESIAN_POINT('Ctrl Pts',(-41.0997323690468,45.980970846619,-9.09768919971767));
#36168=CARTESIAN_POINT('Ctrl Pts',(-41.1175783684503,45.9882410418966,-9.10457783273117));
#36169=CARTESIAN_POINT('Ctrl Pts',(-41.1357530721898,45.995124204242,-9.11104526644371));
#36170=CARTESIAN_POINT('Ctrl Pts',(-41.1542768365912,46.0015853108649,-9.11707659944144));
#36171=CARTESIAN_POINT('Ctrl Pts',(-41.156818842632,46.0024719649871,-9.11790427596452));
#36172=CARTESIAN_POINT('Ctrl Pts',(-41.1593674315456,46.0033506623359,-9.11872373054841));
#36173=CARTESIAN_POINT('Ctrl Pts',(-41.1619226753163,46.004221294345,-9.11953490665145));
#36174=CARTESIAN_POINT('Ctrl Pts',(-41.1704135486274,46.0071143357743,-9.1222303807988));
#36175=CARTESIAN_POINT('Ctrl Pts',(-41.1789781331318,46.0099185180234,-9.12483463091471));
#36176=CARTESIAN_POINT('Ctrl Pts',(-41.1876175255668,46.012629587761,-9.12734530816554));
#36177=CARTESIAN_POINT('Ctrl Pts',(-41.1897510659709,46.0132990997512,-9.12796533224672));
#36178=CARTESIAN_POINT('Ctrl Pts',(-41.1918897775883,46.0139630703871,-9.12857977397601));
#36179=CARTESIAN_POINT('Ctrl Pts',(-41.1940327772883,46.0146211955286,-9.12918837786116));
#36180=CARTESIAN_POINT('Ctrl Pts',(-41.1994431252239,46.0162827384585,-9.13072489640275));
#36181=CARTESIAN_POINT('Ctrl Pts',(-41.2048875125716,46.0179089567826,-9.13222599105199));
#36182=CARTESIAN_POINT('Ctrl Pts',(-41.2103433164833,46.01949241214,-9.13368519234456));
#36183=CARTESIAN_POINT('Ctrl Pts',(-41.2141730168133,46.0206039182724,-9.13470947836403));
#36184=CARTESIAN_POINT('Ctrl Pts',(-41.2180113408301,46.0216952045486,-9.1357139077503));
#36185=CARTESIAN_POINT('Ctrl Pts',(-41.2218548938735,46.0227649655191,-9.13669740800758));
#36186=CARTESIAN_POINT('Ctrl Pts',(-41.2234868793636,46.0232191896087,-9.13711500550951));
#36187=CARTESIAN_POINT('Ctrl Pts',(-41.2251202992978,46.023669717826,-9.13752900998855));
#36188=CARTESIAN_POINT('Ctrl Pts',(-41.2267552532063,46.0241165597052,-9.13793943857175));
#36189=CARTESIAN_POINT('Ctrl Pts',(-41.2706392371279,46.0361102934392,-9.14895579888199));
#36190=CARTESIAN_POINT('Ctrl Pts',(-41.3154708392568,46.0454052275782,-9.15735727293221));
#36191=CARTESIAN_POINT('Ctrl Pts',(-41.3613242473302,46.0517061076808,-9.16303121925624));
#36192=CARTESIAN_POINT('Ctrl Pts',(-41.3622325672626,46.0518309231575,-9.16314361566815));
#36193=CARTESIAN_POINT('Ctrl Pts',(-41.363141287959,46.0519545639161,-9.16325494161169));
#36194=CARTESIAN_POINT('Ctrl Pts',(-41.3640504097949,46.0520770278875,-9.16336519637614));
#36195=CARTESIAN_POINT('Ctrl Pts',(-41.3746147603127,46.0535001070264,-9.16464639976599));
#36196=CARTESIAN_POINT('Ctrl Pts',(-41.3852336299998,46.0547636322353,-9.16578203782526));
#36197=CARTESIAN_POINT('Ctrl Pts',(-41.3959082607259,46.0558632218831,-9.16676933263137));
#36198=CARTESIAN_POINT('Ctrl Pts',(-41.3975829399649,46.0560357299541,-9.1669242234334));
#36199=CARTESIAN_POINT('Ctrl Pts',(-41.3992586918721,46.0562041719286,-9.16707543505593));
#36200=CARTESIAN_POINT('Ctrl Pts',(-41.400935632367,46.0563685454413,-9.16722296981535));
#36201=CARTESIAN_POINT('Ctrl Pts',(-41.4050631402276,46.056773123283,-9.16758610188894));
#36202=CARTESIAN_POINT('Ctrl Pts',(-41.4092022420157,46.0571532335852,-9.16792712030245));
#36203=CARTESIAN_POINT('Ctrl Pts',(-41.4133477595884,46.0575084263247,-9.16824566991062));
#36204=CARTESIAN_POINT('Ctrl Pts',(-41.4191775347142,46.058007928199,-9.16869364113485));
#36205=CARTESIAN_POINT('Ctrl Pts',(-41.4250298031295,46.0584589035442,-9.16909785059445));
#36206=CARTESIAN_POINT('Ctrl Pts',(-41.4308719865823,46.0588582722967,-9.16945566965012));
#36207=CARTESIAN_POINT('Ctrl Pts',(-41.4333568786799,46.0590281382834,-9.16960786304682));
#36208=CARTESIAN_POINT('Ctrl Pts',(-41.4358415456161,46.0591888251255,-9.16975180467935));
#36209=CARTESIAN_POINT('Ctrl Pts',(-41.4383245331774,46.0593401770602,-9.16988736505531));
#36210=CARTESIAN_POINT('Ctrl Pts',(-41.4591923685483,46.0606121879659,-9.17102665856302));
#36211=CARTESIAN_POINT('Ctrl Pts',(-41.4799966113902,46.0612348057782,-9.17158334235594));
#36212=CARTESIAN_POINT('Ctrl Pts',(-41.5007378023747,46.0612196712951,-9.17156968029259));
#36213=CARTESIAN_POINT('Ctrl Pts',(-41.5047693863103,46.0612167295191,-9.17156702471919));
#36214=CARTESIAN_POINT('Ctrl Pts',(-41.5087985900968,46.0611896836042,-9.17154281273808));
#36215=CARTESIAN_POINT('Ctrl Pts',(-41.5128254233789,46.0611386323799,-9.17149714643567));
#36216=CARTESIAN_POINT('Ctrl Pts',(-41.5551621119526,46.0606018980201,-9.1710170272234));
#36217=CARTESIAN_POINT('Ctrl Pts',(-41.597237127505,46.0574150733128,-9.16817483501116));
#36218=CARTESIAN_POINT('Ctrl Pts',(-41.6390554803649,46.0516537176579,-9.16298455103823));
#36219=CARTESIAN_POINT('Ctrl Pts',(-41.6459705250399,46.0507010251434,-9.16212629041595));
#36220=CARTESIAN_POINT('Ctrl Pts',(-41.6528785212426,46.0496776586956,-9.16120357316154));
#36221=CARTESIAN_POINT('Ctrl Pts',(-41.6597795012171,46.0485840352099,-9.16021652676587));
#36222=CARTESIAN_POINT('Ctrl Pts',(-41.6643042060876,46.0478669887136,-9.15956935873315));
#36223=CARTESIAN_POINT('Ctrl Pts',(-41.6688258813008,46.0471196804026,-9.15889438348601));
#36224=CARTESIAN_POINT('Ctrl Pts',(-41.6733445308942,46.0463421899949,-9.15819153918479));
#36225=CARTESIAN_POINT('Ctrl Pts',(-41.6748835466363,46.0460773830096,-9.15795215606347));
#36226=CARTESIAN_POINT('Ctrl Pts',(-41.6764221541904,46.0458090855128,-9.1577095497241));
#36227=CARTESIAN_POINT('Ctrl Pts',(-41.6779604238888,46.0455372875763,-9.15746370590037));
#36228=CARTESIAN_POINT('Ctrl Pts',(-41.6840106761485,46.0444682643214,-9.15649676417899));
#36229=CARTESIAN_POINT('Ctrl Pts',(-41.6900641690809,46.0433433592062,-9.1554781681718));
#36230=CARTESIAN_POINT('Ctrl Pts',(-41.6960827237929,46.0421703401118,-9.15441460909197));
#36231=CARTESIAN_POINT('Ctrl Pts',(-41.6998790708115,46.0414304303237,-9.15374374382032));
#36232=CARTESIAN_POINT('Ctrl Pts',(-41.7036636983394,46.0406710582769,-9.15305470289116));
#36233=CARTESIAN_POINT('Ctrl Pts',(-41.7074378395222,46.0398922878319,-9.15234745459851));
#36234=CARTESIAN_POINT('Ctrl Pts',(-41.7155936736881,46.0382093824253,-9.15081910695343));
#36235=CARTESIAN_POINT('Ctrl Pts',(-41.72369729212,46.0364364941332,-9.14920628329334));
#36236=CARTESIAN_POINT('Ctrl Pts',(-41.7317501971088,46.0345766419165,-9.14751080796047));
#36237=CARTESIAN_POINT('Ctrl Pts',(-41.7459701129861,46.0312924926432,-9.14451691735341));
#36238=CARTESIAN_POINT('Ctrl Pts',(-41.7600321613098,46.0277375113706,-9.14126567927191));
#36239=CARTESIAN_POINT('Ctrl Pts',(-41.7739425547014,46.0239257273487,-9.13776416316361));
#36240=CARTESIAN_POINT('Ctrl Pts',(-41.7829275571194,46.0214636195068,-9.13550246359741));
#36241=CARTESIAN_POINT('Ctrl Pts',(-41.7918493634354,46.0188942453244,-9.13313622688385));
#36242=CARTESIAN_POINT('Ctrl Pts',(-41.8007097354328,46.0162214790045,-9.13066740684117));
#36243=CARTESIAN_POINT('Ctrl Pts',(-41.8231045987492,46.0094659797514,-9.12442738808974));
#36244=CARTESIAN_POINT('Ctrl Pts',(-41.8451065966985,46.0020494043586,-9.1175315624867));
#36245=CARTESIAN_POINT('Ctrl Pts',(-41.8667342232812,45.9940222828129,-9.1099973249351));
#36246=CARTESIAN_POINT('Ctrl Pts',(-41.877486866624,45.9900314253456,-9.10625151542884));
#36247=CARTESIAN_POINT('Ctrl Pts',(-41.8881468432435,45.9858895015613,-9.10234771278249));
#36248=CARTESIAN_POINT('Ctrl Pts',(-41.8987157309372,45.9816019214929,-9.09828701783937));
#36249=CARTESIAN_POINT('Ctrl Pts',(-41.8992684305478,45.9813777026439,-9.09807466393998));
#36250=CARTESIAN_POINT('Ctrl Pts',(-41.8998209127248,45.9811530714684,-9.0978618675743));
#36251=CARTESIAN_POINT('Ctrl Pts',(-41.9003731723471,45.9809280309924,-9.0976486310334));
#36252=CARTESIAN_POINT('Ctrl Pts',(-41.9054678885501,45.9788519832191,-9.09568147715134));
#36253=CARTESIAN_POINT('Ctrl Pts',(-41.9105415297137,45.9767419774063,-9.09367769460556));
#36254=CARTESIAN_POINT('Ctrl Pts',(-41.9155943505303,45.9745986307123,-9.09163740977237));
#36255=CARTESIAN_POINT('Ctrl Pts',(-41.920428408595,45.9725480805845,-9.08968545942426));
#36256=CARTESIAN_POINT('Ctrl Pts',(-41.9252467388496,45.9704655358539,-9.08769868451621));
#36257=CARTESIAN_POINT('Ctrl Pts',(-41.9300373853927,45.9683566610691,-9.0856820673569));
#36258=CARTESIAN_POINT('Ctrl Pts',(-41.9302541835792,45.9682612250513,-9.08559080640934));
#36259=CARTESIAN_POINT('Ctrl Pts',(-41.9304709087346,45.9681657434396,-9.0854994922948));
#36260=CARTESIAN_POINT('Ctrl Pts',(-41.9306875601532,45.9680702166347,-9.08540812536772));
#36261=CARTESIAN_POINT('Ctrl Pts',(-41.9406956697401,45.9636574011657,-9.08118747348054));
#36262=CARTESIAN_POINT('Ctrl Pts',(-41.9505663499056,45.9591375950147,-9.076844031651));
#36263=CARTESIAN_POINT('Ctrl Pts',(-41.9603058228263,45.9545177334838,-9.07238130366819));
#36264=CARTESIAN_POINT('Ctrl Pts',(-41.9797847686677,45.945278010422,-9.06345584770257));
#36265=CARTESIAN_POINT('Ctrl Pts',(-41.9987389093858,45.9356380219542,-9.05405328598334));
#36266=CARTESIAN_POINT('Ctrl Pts',(-42.0172051609414,45.9256425922258,-9.04419084073549));
#36267=CARTESIAN_POINT('Ctrl Pts',(-42.0270287387187,45.920325276957,-9.03894426983965));
#36268=CARTESIAN_POINT('Ctrl Pts',(-42.0367132025377,45.914906801506,-9.03356697121349));
#36269=CARTESIAN_POINT('Ctrl Pts',(-42.0462652696518,45.9093943753032,-9.02806185483883));
#36270=CARTESIAN_POINT('Ctrl Pts',(-42.0726249402372,45.8941824073494,-9.01287005892311));
#36271=CARTESIAN_POINT('Ctrl Pts',(-42.0979709345613,45.8782510965609,-8.99670208157806));
#36272=CARTESIAN_POINT('Ctrl Pts',(-42.1223609992132,45.8616940208704,-8.9795641926535));
#36273=CARTESIAN_POINT('Ctrl Pts',(-42.1313706154958,45.8555778870732,-8.97323350820027));
#36274=CARTESIAN_POINT('Ctrl Pts',(-42.1402490867898,45.8493758516663,-8.96676990574525));
#36275=CARTESIAN_POINT('Ctrl Pts',(-42.1489996451523,45.8430926072868,-8.96017350691971));
#36276=CARTESIAN_POINT('Ctrl Pts',(-42.1563855691804,45.8377892239237,-8.95460580500096));
#36277=CARTESIAN_POINT('Ctrl Pts',(-42.163679614432,45.8324274898817,-8.94894301025735));
#36278=CARTESIAN_POINT('Ctrl Pts',(-42.1708825098498,45.8270094521259,-8.94318436310254));
#36279=CARTESIAN_POINT('Ctrl Pts',(-42.1715164970955,45.826532565175,-8.94267749626121));
#36280=CARTESIAN_POINT('Ctrl Pts',(-42.1721497892792,45.8260552345097,-8.94216987881008));
#36281=CARTESIAN_POINT('Ctrl Pts',(-42.1727823839537,45.8255774636144,-8.94166151241245));
#36282=CARTESIAN_POINT('Ctrl Pts',(-42.1800008105882,45.8201257039106,-8.93586063280913));
#36283=CARTESIAN_POINT('Ctrl Pts',(-42.1871355609368,45.8146106227731,-8.92995567082541));
#36284=CARTESIAN_POINT('Ctrl Pts',(-42.1941438037635,45.8090689774266,-8.92398344742641));
#36285=CARTESIAN_POINT('Ctrl Pts',(-42.1947012737151,45.8086281678201,-8.92350838753319));
#36286=CARTESIAN_POINT('Ctrl Pts',(-42.1952579602536,45.8081871725404,-8.92303288316482));
#36287=CARTESIAN_POINT('Ctrl Pts',(-42.1958138432048,45.8077460097417,-8.92255695245784));
#36288=CARTESIAN_POINT('Ctrl Pts',(-42.202858678639,45.8021550497934,-8.91652537062681));
#36289=CARTESIAN_POINT('Ctrl Pts',(-42.2097822113911,45.7965317839233,-8.9104196370166));
#36290=CARTESIAN_POINT('Ctrl Pts',(-42.2165862799542,45.7908805491703,-8.90424233881281));
#36291=CARTESIAN_POINT('Ctrl Pts',(-42.2242882910079,45.7844835130251,-8.89724981388376));
#36292=CARTESIAN_POINT('Ctrl Pts',(-42.2318368229378,45.7780494925984,-8.89016435004907));
#36293=CARTESIAN_POINT('Ctrl Pts',(-42.2392360579893,45.7715817007783,-8.8829863360389));
#36294=CARTESIAN_POINT('Ctrl Pts',(-42.2600463073129,45.7533911230477,-8.86279826792616));
#36295=CARTESIAN_POINT('Ctrl Pts',(-42.279680437653,45.7349349810326,-8.84187997974338));
#36296=CARTESIAN_POINT('Ctrl Pts',(-42.2981779437348,45.7162661626306,-8.82022080225078));
#36297=CARTESIAN_POINT('Ctrl Pts',(-42.3042442450087,45.7101436790723,-8.81311762329066));
#36298=CARTESIAN_POINT('Ctrl Pts',(-42.3101877355428,45.7039981411622,-8.80593453369296));
#36299=CARTESIAN_POINT('Ctrl Pts',(-42.3160100276813,45.6978313537452,-8.79867102180722));
#36300=CARTESIAN_POINT('Ctrl Pts',(-42.3342535775375,45.6785083635863,-8.7759115590276));
#36301=CARTESIAN_POINT('Ctrl Pts',(-42.3513057904162,45.6589759364203,-8.75236245922885));
#36302=CARTESIAN_POINT('Ctrl Pts',(-42.3671510448732,45.639270031241,-8.72798189773159));
#36303=CARTESIAN_POINT('Ctrl Pts',(-42.3715615707197,45.6337848934441,-8.7211955695645));
#36304=CARTESIAN_POINT('Ctrl Pts',(-42.3758781640535,45.6282861677551,-8.71434461824596));
#36305=CARTESIAN_POINT('Ctrl Pts',(-42.3801005365623,45.6227745982512,-8.70742804354935));
#36306=CARTESIAN_POINT('Ctrl Pts',(-42.3858833948021,45.6152260873007,-8.69795527180989));
#36307=CARTESIAN_POINT('Ctrl Pts',(-42.391488806919,45.6076532830732,-8.68835912959438));
#36308=CARTESIAN_POINT('Ctrl Pts',(-42.396913432122,45.6000574580988,-8.67863589617369));
#36309=CARTESIAN_POINT('Ctrl Pts',(-42.4005109005079,45.5950201072796,-8.67218770417322));
#36310=CARTESIAN_POINT('Ctrl Pts',(-42.4040280633186,45.5899737539531,-8.66568507158052));
#36311=CARTESIAN_POINT('Ctrl Pts',(-42.4074661359585,45.5849153351961,-8.65912243169166));
#36312=CARTESIAN_POINT('Ctrl Pts',(-42.4085128559495,45.5833753014067,-8.65712443831429));
#36313=CARTESIAN_POINT('Ctrl Pts',(-42.4095518863119,45.5818346257886,-8.6551214860273));
#36314=CARTESIAN_POINT('Ctrl Pts',(-42.4105830246306,45.5802936100937,-8.65311393995478));
#36315=CARTESIAN_POINT('Ctrl Pts',(-42.4137820536097,45.5755127249539,-8.64688567945247));
#36316=CARTESIAN_POINT('Ctrl Pts',(-42.4168989413963,45.5707374091497,-8.64062475253282));
#36317=CARTESIAN_POINT('Ctrl Pts',(-42.4199303687472,45.5659741019819,-8.63433893692391));
#36318=CARTESIAN_POINT('Ctrl Pts',(-42.4210855056866,45.5641590256413,-8.63194370294227));
#36319=CARTESIAN_POINT('Ctrl Pts',(-42.4222286704019,45.5623450452855,-8.62954401310694));
#36320=CARTESIAN_POINT('Ctrl Pts',(-42.4233600795134,45.5605318737104,-8.62713945024177));
#36321=CARTESIAN_POINT('Ctrl Pts',(-42.4261468114457,45.5560659178722,-8.62121686039213));
#36322=CARTESIAN_POINT('Ctrl Pts',(-42.4288602395602,45.5516073585664,-8.61526800567393));
#36323=CARTESIAN_POINT('Ctrl Pts',(-42.4315004765197,45.5471564369526,-8.60929272158343));
#36324=CARTESIAN_POINT('Ctrl Pts',(-42.4444002629478,45.5254099274124,-8.58009841448179));
#36325=CARTESIAN_POINT('Ctrl Pts',(-42.4555601676492,45.5038462446935,-8.55027435752416));
#36326=CARTESIAN_POINT('Ctrl Pts',(-42.4649412712655,45.4824896513182,-8.51979328516327));
#36327=CARTESIAN_POINT('Ctrl Pts',(-42.4663006213825,45.4793950167323,-8.5153764861409));
#36328=CARTESIAN_POINT('Ctrl Pts',(-42.4676225398243,45.4763047255679,-8.51094588086722));
#36329=CARTESIAN_POINT('Ctrl Pts',(-42.4689069078218,45.4732188423179,-8.50650136826789));
#36330=CARTESIAN_POINT('Ctrl Pts',(-42.4783003261938,45.4506497714042,-8.4739957574255));
#36331=CARTESIAN_POINT('Ctrl Pts',(-42.4856862257662,45.4283162396088,-8.44074673253793));
#36332=CARTESIAN_POINT('Ctrl Pts',(-42.4909152369877,45.4062381526062,-8.40669784041856));
#36333=CARTESIAN_POINT('Ctrl Pts',(-42.4912865460965,45.4046704002222,-8.40428004798091));
#36334=CARTESIAN_POINT('Ctrl Pts',(-42.4916469287141,45.4031039305286,-8.40185821169987));
#36335=CARTESIAN_POINT('Ctrl Pts',(-42.4919963320089,45.4015387505793,-8.39943230999391));
#36336=CARTESIAN_POINT('Ctrl Pts',(-42.4930452550499,45.3968400160896,-8.39214965344062));
#36337=CARTESIAN_POINT('Ctrl Pts',(-42.4939953305734,45.3921528864746,-8.38483035099147));
#36338=CARTESIAN_POINT('Ctrl Pts',(-42.4948439764137,45.3874775165642,-8.37747363926369));
#36339=CARTESIAN_POINT('Ctrl Pts',(-42.495975311871,45.3812447496024,-8.367666357555));
#36340=CARTESIAN_POINT('Ctrl Pts',(-42.4969273136303,45.3750282608174,-8.35778516090225));
#36341=CARTESIAN_POINT('Ctrl Pts',(-42.4976922377975,45.3688434603943,-8.34785239611548));
#36342=CARTESIAN_POINT('Ctrl Pts',(-42.499222086132,45.356473859548,-8.32798686654192));
#36343=CARTESIAN_POINT('Ctrl Pts',(-42.4999999944414,45.3442749544122,-8.30798620935071));
#36344=CARTESIAN_POINT('Ctrl Pts',(-42.5,45.3322472608192,-8.28784904304297));
#36345=CARTESIAN_POINT('',(-42.5,44.9368005344369,-5.30952630282035));
#36346=CARTESIAN_POINT('Origin',(-42.5,48.5946168001447,-6.3392739254555));
#36347=CARTESIAN_POINT('',(-42.,44.9368005344369,-5.30952630282035));
#36348=CARTESIAN_POINT('',(-45.,51.536059602328,-8.74508236369084));
#36349=CARTESIAN_POINT('',(-45.,51.536059602328,-8.74508236369084));
#36350=CARTESIAN_POINT('',(-45.,51.508884771774,-8.77792974158369));
#36351=CARTESIAN_POINT('Origin',(-45.,48.5946168001447,-6.3392739254555));
#36352=CARTESIAN_POINT('',(-39.,51.508884771774,-8.77792974158369));
#36353=CARTESIAN_POINT('Origin',(-33.6035533905933,20.7255401693197,-1.65106132841495));
#36354=CARTESIAN_POINT('',(-38.5,21.2255401693197,3.24538528099178));
#36355=CARTESIAN_POINT('',(-33.6035533905933,21.2255401693197,-1.65106132841495));
#36356=CARTESIAN_POINT('',(-38.1464466094067,20.7255401693197,3.59893867158506));
#36357=CARTESIAN_POINT('Origin',(-38.5,20.7255401693197,3.24538528099178));
#36358=CARTESIAN_POINT('',(-38.5,20.2255401693197,3.24538528099178));
#36359=CARTESIAN_POINT('Origin',(-38.5,20.7255401693197,3.24538528099178));
#36360=CARTESIAN_POINT('',(-33.6035533905933,20.2255401693197,-1.65106132841495));
#36361=CARTESIAN_POINT('Origin',(-56.6690017314647,51.2606171391062,-5.48344555910069));
#36362=CARTESIAN_POINT('',(-45.,52.2127601173067,-5.17779257111684));
#36363=CARTESIAN_POINT('Origin',(-45.,51.2606171391062,-5.48344555910069));
#36364=CARTESIAN_POINT('',(-46.,52.2127601173067,-5.17779257111684));
#36365=CARTESIAN_POINT('Origin',(-46.,51.2606171391062,-5.48344555910069));
#36366=CARTESIAN_POINT('',(-39.,52.2127601173067,-5.17779257111684));
#36367=CARTESIAN_POINT('Origin',(-45.5,34.999999994595,6.54998265276524E-10));
#36368=CARTESIAN_POINT('',(-46.,18.5003030276807,-0.0999999993449978));
#36369=CARTESIAN_POINT('',(-46.,51.1450373092966,-3.40408138892615));
#36370=CARTESIAN_POINT('Origin',(-46.,34.999999994595,6.54998265276524E-10));
#36371=CARTESIAN_POINT('',(-45.9555887800306,18.2967958718846,-0.306006949495285));
#36372=CARTESIAN_POINT('Ctrl Pts',(-46.,18.5003030276807,-0.0999999993450115));
#36373=CARTESIAN_POINT('Ctrl Pts',(-46.,18.4992558329104,-0.101053560099588));
#36374=CARTESIAN_POINT('Ctrl Pts',(-45.9999966700292,18.4982086857198,-0.102107173286065));
#36375=CARTESIAN_POINT('Ctrl Pts',(-45.9996635810359,18.4458478552488,-0.15479633935181));
#36376=CARTESIAN_POINT('Ctrl Pts',(-45.9913355526387,18.3943785329297,-0.206835262360072));
#36377=CARTESIAN_POINT('Ctrl Pts',(-45.9691910264621,18.3285791615519,-0.273658918954145));
#36378=CARTESIAN_POINT('Ctrl Pts',(-45.9628568381822,18.3125775652319,-0.289933483313417));
#36379=CARTESIAN_POINT('Ctrl Pts',(-45.9555887800306,18.2967958718846,-0.306006949495283));
#36380=CARTESIAN_POINT('Ctrl Pts',(-45.9555887800306,18.2967958718846,-0.306006949495305));
#36381=CARTESIAN_POINT('Ctrl Pts',(-45.9449932969391,18.2729210477128,-0.282057797773911));
#36382=CARTESIAN_POINT('Ctrl Pts',(-45.9326039209885,18.2499149945026,-0.256551740908599));
#36383=CARTESIAN_POINT('Ctrl Pts',(-45.8727877520938,18.1568360367878,-0.141654083468818));
#36384=CARTESIAN_POINT('Ctrl Pts',(-45.8108354668021,18.0994281624082,-0.0403766288579828));
#36385=CARTESIAN_POINT('Ctrl Pts',(-45.66422179789,18.0209250472194,0.185216864286121));
#36386=CARTESIAN_POINT('Ctrl Pts',(-45.5833719890191,18.0028239046249,0.303488964622345));
#36387=CARTESIAN_POINT('Ctrl Pts',(-45.5021062448037,18.005240100147,0.421930518868415));
#36388=CARTESIAN_POINT('Ctrl Pts',(-45.5010531216555,18.0052749455469,0.423465305044224));
#36389=CARTESIAN_POINT('Ctrl Pts',(-45.5,18.0053133249326,0.425000000654998));
#36390=CARTESIAN_POINT('Origin',(-45.5,51.1450373092966,-3.40408138892615));
#36391=CARTESIAN_POINT('Origin',(-38.5,20.7255401693197,-2.54750793782168));
#36392=CARTESIAN_POINT('',(-39.,22.3838525644974,-5.04750793782168));
#36393=CARTESIAN_POINT('Ctrl Pts',(-39.,22.3838525644974,-5.04750793782167));
#36394=CARTESIAN_POINT('Ctrl Pts',(-39.,21.8319612940798,-5.04750793782167));
#36395=CARTESIAN_POINT('Ctrl Pts',(-38.7253086676699,21.2293456661496,-5.04750793782167));
#36396=CARTESIAN_POINT('Ctrl Pts',(-38.5,20.7255401693197,-5.04750793782167));
#36397=CARTESIAN_POINT('',(-39.,21.7255401693197,0.280919186924516));
#36398=CARTESIAN_POINT('Origin',(-39.,20.7255401693197,-2.54750793782168));
#36399=CARTESIAN_POINT('Ctrl Pts',(-38.5,21.2255401693197,-0.0980181950384987));
#36400=CARTESIAN_POINT('Ctrl Pts',(-38.5068454246389,21.2255401693197,-0.0980181950384987));
#36401=CARTESIAN_POINT('Ctrl Pts',(-38.5137049378611,21.2256807402194,-0.0979034111946656));
#36402=CARTESIAN_POINT('Ctrl Pts',(-38.574487053383,21.2281840126506,-0.0958597862843718));
#36403=CARTESIAN_POINT('Ctrl Pts',(-38.6266179130002,21.2390520815176,-0.0869664209613689));
#36404=CARTESIAN_POINT('Ctrl Pts',(-38.7343668418878,21.2793907655706,-0.0543730508899923));
#36405=CARTESIAN_POINT('Ctrl Pts',(-38.78643803375,21.3115857796177,-0.0285603789798281));
#36406=CARTESIAN_POINT('Ctrl Pts',(-38.8850764070747,21.3983579125978,0.0395179277113517));
#36407=CARTESIAN_POINT('Ctrl Pts',(-38.9288507671717,21.4581607205219,0.0855519592452586));
#36408=CARTESIAN_POINT('Ctrl Pts',(-38.9855092027928,21.5879815055175,0.182314659292807));
#36409=CARTESIAN_POINT('Ctrl Pts',(-38.9995659056513,21.6549720437981,0.23098157372654));
#36410=CARTESIAN_POINT('Ctrl Pts',(-38.9999967004912,21.7234428444743,0.279435862662996));
#36411=CARTESIAN_POINT('Ctrl Pts',(-39.,21.7244914385065,0.280177622254829));
#36412=CARTESIAN_POINT('Ctrl Pts',(-39.,21.7255401693197,0.280919186924513));
#36413=CARTESIAN_POINT('Origin',(-29.,39.9592920728172,13.6255430020507));
#36414=CARTESIAN_POINT('',(-38.5,42.4320695804642,13.2576144795422));
#36415=CARTESIAN_POINT('',(-38.5,42.3431727827618,14.3786118971418));
#36416=CARTESIAN_POINT('Origin',(-38.5,39.9592920728172,13.6255430020507));
#36417=CARTESIAN_POINT('',(-39.0000007124813,41.5278577838399,15.5722329253343));
#36418=CARTESIAN_POINT('Ctrl Pts',(-38.5,42.3431727827618,14.3786118971418));
#36419=CARTESIAN_POINT('Ctrl Pts',(-38.5000000077005,42.3332086900109,14.4101537768502));
#36420=CARTESIAN_POINT('Ctrl Pts',(-38.5011441382107,42.3226977455079,14.4412538314269));
#36421=CARTESIAN_POINT('Ctrl Pts',(-38.5032795388733,42.3116545294946,14.4719455803148));
#36422=CARTESIAN_POINT('Ctrl Pts',(-38.5053650307195,42.3008694167266,14.5019199983108));
#36423=CARTESIAN_POINT('Ctrl Pts',(-38.508397245918,42.2895766285646,14.5315047214286));
#36424=CARTESIAN_POINT('Ctrl Pts',(-38.5122659121586,42.2777903788033,14.560725126099));
#36425=CARTESIAN_POINT('Ctrl Pts',(-38.5123584949005,42.2775083169113,14.5614244123686));
#36426=CARTESIAN_POINT('Ctrl Pts',(-38.5124515587901,42.2772259722098,14.5621234898174));
#36427=CARTESIAN_POINT('Ctrl Pts',(-38.5125451029203,42.2769433448068,14.5628223586732));
#36428=CARTESIAN_POINT('Ctrl Pts',(-38.5204047012563,42.2531969284258,14.6215414731906));
#36429=CARTESIAN_POINT('Ctrl Pts',(-38.5316230864511,42.2274542851575,14.678791826982));
#36430=CARTESIAN_POINT('Ctrl Pts',(-38.5455756576484,42.1997725506805,14.7347081062229));
#36431=CARTESIAN_POINT('Ctrl Pts',(-38.5458333631473,42.1992612660511,14.7357408859475));
#36432=CARTESIAN_POINT('Ctrl Pts',(-38.5460920078943,42.1987493186971,14.7367732092197));
#36433=CARTESIAN_POINT('Ctrl Pts',(-38.5463515890497,42.198236708752,14.7378050766535));
#36434=CARTESIAN_POINT('Ctrl Pts',(-38.5532264361405,42.1846605499451,14.7651334503657));
#36435=CARTESIAN_POINT('Ctrl Pts',(-38.5607577577241,42.1706197463063,14.7921419417493));
#36436=CARTESIAN_POINT('Ctrl Pts',(-38.5688931749403,42.1561170515871,14.8188409584105));
#36437=CARTESIAN_POINT('Ctrl Pts',(-38.5692268877671,42.1555221545926,14.8199361455517));
#36438=CARTESIAN_POINT('Ctrl Pts',(-38.5695616183357,42.1549264801115,14.8210308116731));
#36439=CARTESIAN_POINT('Ctrl Pts',(-38.5698973635473,42.154330028203,14.8221249573718));
#36440=CARTESIAN_POINT('Ctrl Pts',(-38.5738150194497,42.14737030619,14.8348920385001));
#36441=CARTESIAN_POINT('Ctrl Pts',(-38.577870714569,42.1403046598116,14.8475883947252));
#36442=CARTESIAN_POINT('Ctrl Pts',(-38.5820595331401,42.1331334156534,14.8602145438691));
#36443=CARTESIAN_POINT('Ctrl Pts',(-38.5824259517601,42.1325061081337,14.8613190214363));
#36444=CARTESIAN_POINT('Ctrl Pts',(-38.5827934015943,42.131877974359,14.8624229867996));
#36445=CARTESIAN_POINT('Ctrl Pts',(-38.583161865111,42.1312490379265,14.8635264020773));
#36446=CARTESIAN_POINT('Ctrl Pts',(-38.5854521945635,42.1273396369413,14.8703851123555));
#36447=CARTESIAN_POINT('Ctrl Pts',(-38.5877835411621,42.1233961168598,14.8772279257529));
#36448=CARTESIAN_POINT('Ctrl Pts',(-38.5901473083312,42.1194314671435,14.8840331025438));
#36449=CARTESIAN_POINT('Ctrl Pts',(-38.5921285576339,42.1161083989546,14.889737028018));
#36450=CARTESIAN_POINT('Ctrl Pts',(-38.5941334747018,42.1127691873607,14.8954168261815));
#36451=CARTESIAN_POINT('Ctrl Pts',(-38.5961604876585,42.109415270011,14.9010704368357));
#36452=CARTESIAN_POINT('Ctrl Pts',(-38.5965518410689,42.1087677324663,14.9021619739191));
#36453=CARTESIAN_POINT('Ctrl Pts',(-38.5969440505148,42.1081195824686,14.9032526548805));
#36454=CARTESIAN_POINT('Ctrl Pts',(-38.5973371193626,42.1074708069969,14.9043425046045));
#36455=CARTESIAN_POINT('Ctrl Pts',(-38.616455858449,42.0759145820762,14.9573524356527));
#36456=CARTESIAN_POINT('Ctrl Pts',(-38.637546796424,42.0429898336134,15.0082122863806));
#36457=CARTESIAN_POINT('Ctrl Pts',(-38.6602044929259,42.0087701554417,15.0571992418101));
#36458=CARTESIAN_POINT('Ctrl Pts',(-38.6605754259393,42.0082099392546,15.0580012156115));
#36459=CARTESIAN_POINT('Ctrl Pts',(-38.660946780572,42.0076493755921,15.05880268647));
#36460=CARTESIAN_POINT('Ctrl Pts',(-38.6613185556365,42.0070884646104,15.0596036552468));
#36461=CARTESIAN_POINT('Ctrl Pts',(-38.6842707148083,41.9724596813525,15.1090528104149));
#36462=CARTESIAN_POINT('Ctrl Pts',(-38.7088227250363,41.9365078483921,15.1565891613654));
#36463=CARTESIAN_POINT('Ctrl Pts',(-38.7346967461674,41.8992750612305,15.2023961989802));
#36464=CARTESIAN_POINT('Ctrl Pts',(-38.7348418833976,41.8990662083594,15.2026531480849));
#36465=CARTESIAN_POINT('Ctrl Pts',(-38.7349870623364,41.8988573151551,15.2029100427124));
#36466=CARTESIAN_POINT('Ctrl Pts',(-38.7351322829497,41.8986483816199,15.2031668828852));
#36467=CARTESIAN_POINT('Ctrl Pts',(-38.7611663896273,41.8611922807128,15.2492113410937));
#36468=CARTESIAN_POINT('Ctrl Pts',(-38.7885386651593,41.8224405096622,15.2935061409713));
#36469=CARTESIAN_POINT('Ctrl Pts',(-38.8170528293073,41.7824089839123,15.336170002502));
#36470=CARTESIAN_POINT('Ctrl Pts',(-38.8173470127179,41.7819959747595,15.3366101697196));
#36471=CARTESIAN_POINT('Ctrl Pts',(-38.8176413177686,41.7815828293836,15.3370501632323));
#36472=CARTESIAN_POINT('Ctrl Pts',(-38.8179357442455,41.7811695478035,15.3374899831624));
#36473=CARTESIAN_POINT('Ctrl Pts',(-38.8319101796259,41.7615538637952,15.3583652633232));
#36474=CARTESIAN_POINT('Ctrl Pts',(-38.8461591058041,41.7416309802697,15.3788488599945));
#36475=CARTESIAN_POINT('Ctrl Pts',(-38.8606646627554,41.721400690848,15.3989502376356));
#36476=CARTESIAN_POINT('Ctrl Pts',(-38.8612582506509,41.7205728388073,15.399772814424));
#36477=CARTESIAN_POINT('Ctrl Pts',(-38.8618522681823,41.7197444719415,15.4005947511531));
#36478=CARTESIAN_POINT('Ctrl Pts',(-38.8624467141622,41.7189155902482,15.4014160484433));
#36479=CARTESIAN_POINT('Ctrl Pts',(-38.8692685604167,41.7094033659809,15.4108412343021));
#36480=CARTESIAN_POINT('Ctrl Pts',(-38.8761468721562,41.6998233208851,15.4201821773756));
#36481=CARTESIAN_POINT('Ctrl Pts',(-38.8830800584607,41.6901753398805,15.4294396502778));
#36482=CARTESIAN_POINT('Ctrl Pts',(-38.8838431424214,41.6891134587721,15.4304585510802));
#36483=CARTESIAN_POINT('Ctrl Pts',(-38.8846068740394,41.6880507781269,15.4314764182716));
#36484=CARTESIAN_POINT('Ctrl Pts',(-38.8853712624626,41.6869872820628,15.4324932680928));
#36485=CARTESIAN_POINT('Ctrl Pts',(-38.892157093119,41.6775461341138,15.4415203157032));
#36486=CARTESIAN_POINT('Ctrl Pts',(-38.8989982959301,41.6680357161533,15.450471659057));
#36487=CARTESIAN_POINT('Ctrl Pts',(-38.9058773734152,41.6584782132661,15.4593277211414));
#36488=CARTESIAN_POINT('Ctrl Pts',(-38.906818535116,41.6571706025156,15.4605393641955));
#36489=CARTESIAN_POINT('Ctrl Pts',(-38.9077604254252,41.6558620830411,15.4617492470449));
#36490=CARTESIAN_POINT('Ctrl Pts',(-38.9087029786515,41.6545527406419,15.4629572906983));
#36491=CARTESIAN_POINT('Ctrl Pts',(-38.9384215702937,41.6132693298003,15.5010467640772));
#36492=CARTESIAN_POINT('Ctrl Pts',(-38.9688951268995,41.5710315059527,15.537445734224));
#36493=CARTESIAN_POINT('Ctrl Pts',(-39.0000000000001,41.5278577956883,15.5722329400385));
#36494=CARTESIAN_POINT('Ctrl Pts',(-39.,40.8143424311349,15.9747745540142));
#36495=CARTESIAN_POINT('Ctrl Pts',(-38.9999968905168,40.8170927138004,15.9737735329881));
#36496=CARTESIAN_POINT('Ctrl Pts',(-38.9999946894569,40.8198412391743,15.9727676820533));
#36497=CARTESIAN_POINT('Ctrl Pts',(-38.9999897502085,40.8289450514986,15.9694179091687));
#36498=CARTESIAN_POINT('Ctrl Pts',(-38.9999901119293,40.8352925259715,15.9670530039168));
#36499=CARTESIAN_POINT('Ctrl Pts',(-38.9999942307407,40.8506913969669,15.9612444021708));
#36500=CARTESIAN_POINT('Ctrl Pts',(-38.9999993739327,40.8597325759833,15.9577738411329));
#36501=CARTESIAN_POINT('Ctrl Pts',(-39.0000003297456,40.8747622467481,15.9519041034816));
#36502=CARTESIAN_POINT('Ctrl Pts',(-39.0000000885938,40.8807723014066,15.9495301114465));
#36503=CARTESIAN_POINT('Ctrl Pts',(-39.0000001965139,40.8947797407981,15.9439340336549));
#36504=CARTESIAN_POINT('Ctrl Pts',(-39.0000001605784,40.9027598121034,15.940698024332));
#36505=CARTESIAN_POINT('Ctrl Pts',(-38.9999998192051,40.942521297217,15.9243345703678));
#36506=CARTESIAN_POINT('Ctrl Pts',(-39.0000017835329,40.97404626887,15.9105936160279));
#36507=CARTESIAN_POINT('Ctrl Pts',(-38.9999985969878,41.0673343728555,15.8676202695839));
#36508=CARTESIAN_POINT('Ctrl Pts',(-39.0000128649755,41.1281933283618,15.836501644433));
#36509=CARTESIAN_POINT('Ctrl Pts',(-38.9999896085028,41.3072289986956,15.7354956717247));
#36510=CARTESIAN_POINT('Ctrl Pts',(-39.0000027484886,41.420993774444,15.6583397034461));
#36511=CARTESIAN_POINT('Ctrl Pts',(-39.0000021374439,41.5278577779207,15.5722329179781));
#36512=CARTESIAN_POINT('',(-39.0000009660842,40.0090091820249,16.1250482632156));
#36513=CARTESIAN_POINT('Ctrl Pts',(-39.0000021374439,40.009009188616,16.1250485948423));
#36514=CARTESIAN_POINT('Ctrl Pts',(-39.0000027484886,40.1462201394576,16.1223193620086));
#36515=CARTESIAN_POINT('Ctrl Pts',(-38.9999896085026,40.2829639141646,16.1082976744922));
#36516=CARTESIAN_POINT('Ctrl Pts',(-39.000012709303,40.4836859506285,16.070843227177));
#36517=CARTESIAN_POINT('Ctrl Pts',(-38.999998495505,40.5489785071788,16.0559240454488));
#36518=CARTESIAN_POINT('Ctrl Pts',(-39.00000168396,40.6474424173353,16.0292233275237));
#36519=CARTESIAN_POINT('Ctrl Pts',(-38.9999997950044,40.6810944759589,16.0193331550335));
#36520=CARTESIAN_POINT('Ctrl Pts',(-39.0000001459518,40.7229000764915,16.0060849487778));
#36521=CARTESIAN_POINT('Ctrl Pts',(-39.0000001992107,40.7312588065207,16.0033875103362));
#36522=CARTESIAN_POINT('Ctrl Pts',(-39.0000001046533,40.7458809046931,15.9985835987506));
#36523=CARTESIAN_POINT('Ctrl Pts',(-39.0000001267302,40.7521343550355,15.9965015278252));
#36524=CARTESIAN_POINT('Ctrl Pts',(-38.9999997949692,40.7677237236382,15.9912428672298));
#36525=CARTESIAN_POINT('Ctrl Pts',(-38.999994537334,40.7770652735991,15.9880299495346));
#36526=CARTESIAN_POINT('Ctrl Pts',(-38.9999906714831,40.7910293624736,15.9831344162146));
#36527=CARTESIAN_POINT('Ctrl Pts',(-38.9999900510404,40.7956664120109,15.9814933750465));
#36528=CARTESIAN_POINT('Ctrl Pts',(-38.9999915437067,40.8026152317053,15.9790111028118));
#36529=CARTESIAN_POINT('Ctrl Pts',(-38.999992445271,40.8049306360383,15.9781801334451));
#36530=CARTESIAN_POINT('Ctrl Pts',(-38.9999945939801,40.8084239880366,15.9769205901392));
#36531=CARTESIAN_POINT('Ctrl Pts',(-38.9999954547499,40.8096028407755,15.9764945475109));
#36532=CARTESIAN_POINT('Ctrl Pts',(-38.9999972820434,40.8117313539399,15.9757234829694));
#36533=CARTESIAN_POINT('Ctrl Pts',(-38.9999981957157,40.8126811315419,15.9753787697989));
#36534=CARTESIAN_POINT('Ctrl Pts',(-38.9999994703163,40.8138679676572,15.9749472039047));
#36535=CARTESIAN_POINT('Ctrl Pts',(-38.9999997317273,40.8141052060082,15.9748608968992));
#36536=CARTESIAN_POINT('Ctrl Pts',(-39.,40.8143424311286,15.9747745540165));
#36537=CARTESIAN_POINT('',(-38.5,38.6171968569105,15.7347562277442));
#36538=CARTESIAN_POINT('Ctrl Pts',(-39.0000000000001,40.0090091891848,16.1250486231625));
#36539=CARTESIAN_POINT('Ctrl Pts',(-38.9688951268995,39.9535754234747,16.1261516034788));
#36540=CARTESIAN_POINT('Ctrl Pts',(-38.9384215702936,39.8978225662111,16.1254183244919));
#36541=CARTESIAN_POINT('Ctrl Pts',(-38.9087029786515,39.8417141971955,16.1227765600433));
#36542=CARTESIAN_POINT('Ctrl Pts',(-38.900871177093,39.8269278433471,16.1220803704265));
#36543=CARTESIAN_POINT('Ctrl Pts',(-38.8930854972452,39.812104173315,16.121250562334));
#36544=CARTESIAN_POINT('Ctrl Pts',(-38.8853712624626,39.7972860007029,16.1202882861625));
#36545=CARTESIAN_POINT('Ctrl Pts',(-38.8776618357207,39.7824770637934,16.1193266097476));
#36546=CARTESIAN_POINT('Ctrl Pts',(-38.8700193900109,39.7676654292003,16.1182323509774));
#36547=CARTESIAN_POINT('Ctrl Pts',(-38.8624467141621,39.7528514459051,16.1170048756422));
#36548=CARTESIAN_POINT('Ctrl Pts',(-38.8473257421527,39.7232711718738,16.1145538767407));
#36549=CARTESIAN_POINT('Ctrl Pts',(-38.8324820332758,39.6936801258928,16.1115718386542));
#36550=CARTESIAN_POINT('Ctrl Pts',(-38.8179357442455,39.6640712649591,16.1080507411338));
#36551=CARTESIAN_POINT('Ctrl Pts',(-38.789103594054,39.6053836420433,16.1010715856711));
#36552=CARTESIAN_POINT('Ctrl Pts',(-38.7614349860432,39.546627259783,16.0919785071308));
#36553=CARTESIAN_POINT('Ctrl Pts',(-38.7351322829496,39.4877360325772,16.0806672153616));
#36554=CARTESIAN_POINT('Ctrl Pts',(-38.7090981762719,39.4294461873854,16.0694714315848));
#36555=CARTESIAN_POINT('Ctrl Pts',(-38.6843994622029,39.3710250338492,16.0561042678525));
#36556=CARTESIAN_POINT('Ctrl Pts',(-38.6613185556365,39.3123854456582,16.0403953443325));
#36557=CARTESIAN_POINT('Ctrl Pts',(-38.6382376490702,39.2537458574673,16.0246864208126));
#36558=CARTESIAN_POINT('Ctrl Pts',(-38.6167688528615,39.1948893427871,16.0066396660535));
#36559=CARTESIAN_POINT('Ctrl Pts',(-38.5973369701107,39.1356882476495,15.9859829569921));
#36560=CARTESIAN_POINT('Ctrl Pts',(-38.5949079847669,39.1282881107573,15.9834008683595));
#36561=CARTESIAN_POINT('Ctrl Pts',(-38.5925110755004,39.1208825181482,15.980777828273));
#36562=CARTESIAN_POINT('Ctrl Pts',(-38.5901473083312,39.1134711369412,15.9781131881224));
#36563=CARTESIAN_POINT('Ctrl Pts',(-38.5877835411621,39.1060597557343,15.9754485479717));
#36564=CARTESIAN_POINT('Ctrl Pts',(-38.5854521945635,39.0986403684223,15.9727414946403));
#36565=CARTESIAN_POINT('Ctrl Pts',(-38.583161865111,39.0912368995364,15.9700003322593));
#36566=CARTESIAN_POINT('Ctrl Pts',(-38.578581206206,39.0764299617645,15.9645180074973));
#36567=CARTESIAN_POINT('Ctrl Pts',(-38.5741577180041,39.0616657176126,15.9588918794025));
#36568=CARTESIAN_POINT('Ctrl Pts',(-38.5698973635473,39.0469434995135,15.9531211601745));
#36569=CARTESIAN_POINT('Ctrl Pts',(-38.5613766546335,39.0174990633154,15.9415797217185));
#36570=CARTESIAN_POINT('Ctrl Pts',(-38.5535084406888,38.9882227073311,15.9294599923279));
#36571=CARTESIAN_POINT('Ctrl Pts',(-38.5463515890497,38.9591092562873,15.9167510543452));
#36572=CARTESIAN_POINT('Ctrl Pts',(-38.5320378857717,38.9008823541996,15.8913331783798));
#36573=CARTESIAN_POINT('Ctrl Pts',(-38.5205498688876,38.8433076021544,15.8635646015542));
#36574=CARTESIAN_POINT('Ctrl Pts',(-38.5125451029203,38.7863397520739,15.8332981660507));
#36575=CARTESIAN_POINT('Ctrl Pts',(-38.5085427199367,38.7578558270336,15.8181649482989));
#36576=CARTESIAN_POINT('Ctrl Pts',(-38.5054149395359,38.7295228449587,15.8024072356763));
#36577=CARTESIAN_POINT('Ctrl Pts',(-38.5032795388733,38.7013349747927,15.7859944344156));
#36578=CARTESIAN_POINT('Ctrl Pts',(-38.5011441382107,38.6731471046267,15.7695816331548));
#36579=CARTESIAN_POINT('Ctrl Pts',(-38.5000000077005,38.6451045242559,15.7525139140583));
#36580=CARTESIAN_POINT('Ctrl Pts',(-38.5,38.6171968569105,15.7347562277442));
#36581=CARTESIAN_POINT('',(-38.5,37.8285347084959,14.9331641453451));
#36582=CARTESIAN_POINT('Origin',(-38.5,39.9592920728172,13.6255430020507));
#36583=CARTESIAN_POINT('',(-35.0170134743162,37.8285347084959,14.9331641453451));
#36584=CARTESIAN_POINT('',(-29.,37.8285347084959,14.9331641453451));
#36585=CARTESIAN_POINT('',(-34.,37.6100605208524,14.4805933603648));
#36586=CARTESIAN_POINT('Ctrl Pts',(-35.0170134743162,37.8285347084959,14.9331641453451));
#36587=CARTESIAN_POINT('Ctrl Pts',(-34.7766127063766,37.8285347084959,14.9331641453451));
#36588=CARTESIAN_POINT('Ctrl Pts',(-34.4906799668777,37.8067211571775,14.9017335941734));
#36589=CARTESIAN_POINT('Ctrl Pts',(-34.1966444375895,37.7349198556759,14.7674315769327));
#36590=CARTESIAN_POINT('Ctrl Pts',(-34.1089154055285,37.7055249860502,14.710036118503));
#36591=CARTESIAN_POINT('Ctrl Pts',(-34.0408467644713,37.6652672213039,14.619544442247));
#36592=CARTESIAN_POINT('Ctrl Pts',(-34.0255956953052,37.6540485473767,14.5934125444763));
#36593=CARTESIAN_POINT('Ctrl Pts',(-34.0051635787926,37.6314787713743,14.537775795392));
#36594=CARTESIAN_POINT('Ctrl Pts',(-34.,37.6201314456043,14.5082629987137));
#36595=CARTESIAN_POINT('Ctrl Pts',(-34.,37.6100605208524,14.4805933603648));
#36596=CARTESIAN_POINT('',(-34.,40.8143424311314,15.9747745540155));
#36597=CARTESIAN_POINT('Origin',(-34.,39.9592920728172,13.6255430020507));
#36598=CARTESIAN_POINT('',(-30.,40.8143424311314,15.9747745540155));
#36599=CARTESIAN_POINT('',(-29.,40.8143424311314,15.9747745540155));
#36600=CARTESIAN_POINT('',(-30.,39.104241714503,11.2763114500859));
#36601=CARTESIAN_POINT('Origin',(-30.,39.9592920728172,13.6255430020507));
#36602=CARTESIAN_POINT('',(-34.,39.104241714503,11.2763114500859));
#36603=CARTESIAN_POINT('',(-29.,39.104241714503,11.2763114500859));
#36604=CARTESIAN_POINT('',(-34.,37.4865145651702,13.9934715245592));
#36605=CARTESIAN_POINT('Origin',(-34.,39.9592920728172,13.6255430020507));
#36606=CARTESIAN_POINT('',(-38.5,37.4865145651702,13.9934715245592));
#36607=CARTESIAN_POINT('',(-29.,37.4865145651702,13.9934715245592));
#36608=CARTESIAN_POINT('',(-38.5,42.0900494371385,12.3179218587563));
#36609=CARTESIAN_POINT('Origin',(-38.5,39.9592920728172,13.6255430020507));
#36610=CARTESIAN_POINT('',(-35.0170134743163,42.0900494371385,12.3179218587563));
#36611=CARTESIAN_POINT('',(-29.,42.0900494371385,12.3179218587563));
#36612=CARTESIAN_POINT('',(-35.0170134743163,42.4320695804642,13.2576144795422));
#36613=CARTESIAN_POINT('Ctrl Pts',(-35.0170134743162,42.0900494371384,12.3179218587562));
#36614=CARTESIAN_POINT('Ctrl Pts',(-34.8763912574935,42.0900494371384,12.3179218587562));
#36615=CARTESIAN_POINT('Ctrl Pts',(-34.7227068456195,42.0966450458144,12.3283241056387));
#36616=CARTESIAN_POINT('Ctrl Pts',(-34.4287581602092,42.129619262702,12.3842797507388));
#36617=CARTESIAN_POINT('Ctrl Pts',(-34.2881480947843,42.1555402154976,12.4282739810068));
#36618=CARTESIAN_POINT('Ctrl Pts',(-34.1203544496629,42.2110688218831,12.5387497630338));
#36619=CARTESIAN_POINT('Ctrl Pts',(-34.0637027306899,42.2362087483756,12.5914709241387));
#36620=CARTESIAN_POINT('Ctrl Pts',(-34.0133005472596,42.2750367777858,12.6827660115511));
#36621=CARTESIAN_POINT('Ctrl Pts',(-34.,42.2936559145693,12.7296439456481));
#36622=CARTESIAN_POINT('Ctrl Pts',(-34.,42.3233913349946,12.8113413418248));
#36623=CARTESIAN_POINT('Ctrl Pts',(-34.0133005472596,42.3392608039313,12.8592200731723));
#36624=CARTESIAN_POINT('Ctrl Pts',(-34.0637027306899,42.3682001587783,12.954114343782));
#36625=CARTESIAN_POINT('Ctrl Pts',(-34.1203544496629,42.3828303669148,13.010660729539));
#36626=CARTESIAN_POINT('Ctrl Pts',(-34.2881480947843,42.4113054504164,13.1309831886277));
#36627=CARTESIAN_POINT('Ctrl Pts',(-34.4287581602092,42.419727794681,13.1813463915421));
#36628=CARTESIAN_POINT('Ctrl Pts',(-34.7227068456195,42.4304356744304,13.2454063205866));
#36629=CARTESIAN_POINT('Ctrl Pts',(-34.8763912574935,42.4320695804641,13.2576144795422));
#36630=CARTESIAN_POINT('Ctrl Pts',(-35.0170134743163,42.4320695804641,13.2576144795422));
#36631=CARTESIAN_POINT('',(-29.,42.4320695804641,13.2576144795422));
#36632=CARTESIAN_POINT('Origin',(-39.22360679775,44.2375118611403,12.0683983434524));
#36633=CARTESIAN_POINT('',(-38.5,43.7265178053794,11.7222960833984));
#36634=CARTESIAN_POINT('',(-34.22360679775,41.7172702375127,12.4536023913736));
#36635=CARTESIAN_POINT('',(-38.5441280858669,43.7468303076589,11.7137963479747));
#36636=CARTESIAN_POINT('Ctrl Pts',(-38.5440016100281,43.7469422033269,11.7139571265323));
#36637=CARTESIAN_POINT('Ctrl Pts',(-38.5292760478545,43.7401182142464,11.7166614290024));
#36638=CARTESIAN_POINT('Ctrl Pts',(-38.5146380311988,43.733428008513,11.7197809751451));
#36639=CARTESIAN_POINT('Ctrl Pts',(-38.5,43.7265178053794,11.7222960833984));
#36640=CARTESIAN_POINT('',(-38.72360679775,44.5278928504519,11.9627083067462));
#36641=CARTESIAN_POINT('Ctrl Pts',(-38.72360679775,44.5278928504519,11.9627083067462));
#36642=CARTESIAN_POINT('Ctrl Pts',(-38.7236071164119,44.5278766506594,11.9626610048945));
#36643=CARTESIAN_POINT('Ctrl Pts',(-38.7236377977353,44.5263169066445,11.9581067008717));
#36644=CARTESIAN_POINT('Ctrl Pts',(-38.7234503028571,44.520850205933,11.9447315525215));
#36645=CARTESIAN_POINT('Ctrl Pts',(-38.723342992434,44.5184918291995,11.9391932030999));
#36646=CARTESIAN_POINT('Ctrl Pts',(-38.7230280284375,44.5139105406859,11.9293688690194));
#36647=CARTESIAN_POINT('Ctrl Pts',(-38.7228315133244,44.5113575460494,11.9240782791388));
#36648=CARTESIAN_POINT('Ctrl Pts',(-38.7225554022308,44.5083537654735,11.9182473393015));
#36649=CARTESIAN_POINT('Ctrl Pts',(-38.7223509758947,44.5062438964329,11.9142436273831));
#36650=CARTESIAN_POINT('Ctrl Pts',(-38.7221757851806,44.5045443141253,11.9111107329527));
#36651=CARTESIAN_POINT('Ctrl Pts',(-38.7211370061962,44.4947708585985,11.893369944279));
#36652=CARTESIAN_POINT('Ctrl Pts',(-38.7197824514153,44.4839246948589,11.8766973126298));
#36653=CARTESIAN_POINT('Ctrl Pts',(-38.7166904074296,44.4614933674347,11.8468572654181));
#36654=CARTESIAN_POINT('Ctrl Pts',(-38.7136115309805,44.4428720028296,11.8254832543129));
#36655=CARTESIAN_POINT('Ctrl Pts',(-38.70872340737,44.4182229539639,11.802559675333));
#36656=CARTESIAN_POINT('Ctrl Pts',(-38.7059584939507,44.4051961946696,11.7916315968734));
#36657=CARTESIAN_POINT('Ctrl Pts',(-38.7047052738609,44.3994663885684,11.7870654782422));
#36658=CARTESIAN_POINT('Ctrl Pts',(-38.7038547062334,44.3956143340404,11.7840477294714));
#36659=CARTESIAN_POINT('Ctrl Pts',(-38.7032214091466,44.3927808200249,11.7818771590184));
#36660=CARTESIAN_POINT('Ctrl Pts',(-38.6991435597199,44.3746484434328,11.768149243923));
#36661=CARTESIAN_POINT('Ctrl Pts',(-38.6939534751656,44.3509398269105,11.7516647130115));
#36662=CARTESIAN_POINT('Ctrl Pts',(-38.6825469826753,44.3014072596727,11.7259746102914));
#36663=CARTESIAN_POINT('Ctrl Pts',(-38.6781356817267,44.2825555777659,11.7172813976112));
#36664=CARTESIAN_POINT('Ctrl Pts',(-38.6703956763465,44.2502811390231,11.7048893824249));
#36665=CARTESIAN_POINT('Ctrl Pts',(-38.6676285755574,44.2388574863255,11.700869024046));
#36666=CARTESIAN_POINT('Ctrl Pts',(-38.6631728052587,44.220673155864,11.6951324489139));
#36667=CARTESIAN_POINT('Ctrl Pts',(-38.6608686350217,44.2113188406999,11.692337984379));
#36668=CARTESIAN_POINT('Ctrl Pts',(-38.6584459125517,44.2015637758563,11.689680377803));
#36669=CARTESIAN_POINT('Ctrl Pts',(-38.6568040371926,44.1949707280962,11.6879419285137));
#36670=CARTESIAN_POINT('Ctrl Pts',(-38.6557035360131,44.1905661326844,11.6868273823973));
#36671=CARTESIAN_POINT('Ctrl Pts',(-38.6178946480498,44.0395516274507,11.6496180167347));
#36672=CARTESIAN_POINT('Ctrl Pts',(-38.5753923705026,43.8784299792084,11.6667202780775));
#36673=CARTESIAN_POINT('Ctrl Pts',(-38.5440337731008,43.7469571082004,11.713951220573));
#36674=CARTESIAN_POINT('',(-38.7126236016579,44.5498673281012,12.1194208390779));
#36675=CARTESIAN_POINT('Origin',(-38.4999999999771,43.897527876974,12.1921423938054));
#36676=CARTESIAN_POINT('',(-38.5,44.068537948705,12.6619887041843));
#36677=CARTESIAN_POINT('Origin',(-38.4999999999998,43.8975278770413,12.1921423937908));
#36678=CARTESIAN_POINT('',(-40.02360679775,44.7843989811175,12.4014365965151));
#36679=CARTESIAN_POINT('Origin',(-38.5,39.9592920728172,13.6255430020507));
#36680=CARTESIAN_POINT('',(-39.,42.9591643136975,13.5978565722447));
#36681=CARTESIAN_POINT('Ctrl Pts',(-39.,42.9591643136975,13.5978565722447));
#36682=CARTESIAN_POINT('Ctrl Pts',(-39.,42.9581087837868,13.5971247176931));
#36683=CARTESIAN_POINT('Ctrl Pts',(-38.9999967004912,42.957053117491,13.596393058341));
#36684=CARTESIAN_POINT('Ctrl Pts',(-38.9995659056514,42.8881025866701,13.5486238950522));
#36685=CARTESIAN_POINT('Ctrl Pts',(-38.9855092027928,42.8194585327967,13.5023184456178));
#36686=CARTESIAN_POINT('Ctrl Pts',(-38.9288507671717,42.6841300141038,13.4134216044716));
#36687=CARTESIAN_POINT('Ctrl Pts',(-38.8850764070747,42.6204184094289,13.3729699132262));
#36688=CARTESIAN_POINT('Ctrl Pts',(-38.78643803375,42.5267679096371,13.3147149323868));
#36689=CARTESIAN_POINT('Ctrl Pts',(-38.7343668418878,42.4915005890015,13.2932899690069));
#36690=CARTESIAN_POINT('Ctrl Pts',(-38.6266179130002,42.4470761971575,13.2665315943734));
#36691=CARTESIAN_POINT('Ctrl Pts',(-38.574487053383,42.435002068918,13.2593606603393));
#36692=CARTESIAN_POINT('Ctrl Pts',(-38.5137049378611,42.4322255200745,13.2577073145927));
#36693=CARTESIAN_POINT('Ctrl Pts',(-38.5068454246389,42.4320695804641,13.2576144795422));
#36694=CARTESIAN_POINT('Ctrl Pts',(-38.5,42.4320695804641,13.2576144795422));
#36695=CARTESIAN_POINT('',(-39.,42.8199489247508,14.5292256761601));
#36696=CARTESIAN_POINT('Origin',(-39.,39.9592920728172,13.6255430020507));
#36697=CARTESIAN_POINT('Origin',(-38.5,42.8199489247508,14.5292256761601));
#36698=CARTESIAN_POINT('Origin',(-45.5,34.999999994595,6.55E-10));
#36699=CARTESIAN_POINT('',(-46.,37.3980464303344,4.94968416149168));
#36700=CARTESIAN_POINT('',(-46.,40.0130956859299,-2.2624923395573));
#36701=CARTESIAN_POINT('Origin',(-46.,34.999999994595,6.55E-10));
#36702=CARTESIAN_POINT('',(-45.5,38.0494565603535,5.1672831023974));
#36703=CARTESIAN_POINT('Ctrl Pts',(-46.,37.3980464303344,4.94968416149168));
#36704=CARTESIAN_POINT('Ctrl Pts',(-46.,37.3994318538483,4.95017943538276));
#36705=CARTESIAN_POINT('Ctrl Pts',(-45.9999966939211,37.4008173501861,4.95067451566463));
#36706=CARTESIAN_POINT('Ctrl Pts',(-45.9996751413526,37.4681689180479,4.97473062725169));
#36707=CARTESIAN_POINT('Ctrl Pts',(-45.9918589780635,37.5346003819143,4.99794942213878));
#36708=CARTESIAN_POINT('Ctrl Pts',(-45.9609910872761,37.660320616289,5.04101720165774));
#36709=CARTESIAN_POINT('Ctrl Pts',(-45.9385897729845,37.7203693432866,5.06117119476266));
#36710=CARTESIAN_POINT('Ctrl Pts',(-45.8753161788561,37.8365974383146,5.09953476308977));
#36711=CARTESIAN_POINT('Ctrl Pts',(-45.8328892935188,37.8925460613842,5.1176110195544));
#36712=CARTESIAN_POINT('Ctrl Pts',(-45.7398209612911,37.9740390280872,5.14361816527401));
#36713=CARTESIAN_POINT('Ctrl Pts',(-45.6935221969332,38.0032214033414,5.15280579280595));
#36714=CARTESIAN_POINT('Ctrl Pts',(-45.5969081567834,38.0402032793475,5.16440403484684));
#36715=CARTESIAN_POINT('Ctrl Pts',(-45.548970157778,38.0494565603535,5.16728310239741));
#36716=CARTESIAN_POINT('Ctrl Pts',(-45.5,38.0494565603535,5.1672831023974));
#36717=CARTESIAN_POINT('',(-45.5,40.65404535889,-2.00792704445741));
#36718=CARTESIAN_POINT('Origin',(-45.5,34.999999994595,6.55E-10));
#36719=CARTESIAN_POINT('Ctrl Pts',(-45.5,40.6540453588901,-2.00792704445741));
#36720=CARTESIAN_POINT('Ctrl Pts',(-45.548789362425,40.6540453588901,-2.00792704445741));
#36721=CARTESIAN_POINT('Ctrl Pts',(-45.5965455901767,40.6451475101065,-2.01167834637272));
#36722=CARTESIAN_POINT('Ctrl Pts',(-45.6928616793168,40.6095174739276,-2.02660507937416));
#36723=CARTESIAN_POINT('Ctrl Pts',(-45.7390416503862,40.5813587441991,-2.03836511974797));
#36724=CARTESIAN_POINT('Ctrl Pts',(-45.8320302750286,40.5024145653791,-2.07097275523011));
#36725=CARTESIAN_POINT('Ctrl Pts',(-45.8744779446781,40.4479929468233,-2.0932224681912));
#36726=CARTESIAN_POINT('Ctrl Pts',(-45.938073114642,40.3340359761707,-2.13897191074204));
#36727=CARTESIAN_POINT('Ctrl Pts',(-45.9606603025493,40.274676254965,-2.16245456892374));
#36728=CARTESIAN_POINT('Ctrl Pts',(-45.9917939389948,40.149785821394,-2.21095308019115));
#36729=CARTESIAN_POINT('Ctrl Pts',(-45.9996738586592,40.0834454567978,-2.23623621749007));
#36730=CARTESIAN_POINT('Ctrl Pts',(-45.9999966944273,40.0158649969536,-2.261459414675));
#36731=CARTESIAN_POINT('Ctrl Pts',(-46.,40.0144803764284,-2.2619759759402));
#36732=CARTESIAN_POINT('Ctrl Pts',(-46.,40.0130956859299,-2.2624923395573));
#36733=CARTESIAN_POINT('Origin',(-45.5,34.999999994595,6.55E-10));
#36734=CARTESIAN_POINT('',(-45.5,39.9429588225849,9.26375507215795));
#36735=CARTESIAN_POINT('',(-45.5,44.7486243140984,-3.90055430318255));
#36736=CARTESIAN_POINT('Origin',(-45.5,34.999999994595,6.55E-10));
#36737=CARTESIAN_POINT('',(-46.,39.7058929474701,9.94256362962317));
#36738=CARTESIAN_POINT('Ctrl Pts',(-46.,39.7058929474701,9.94256362962317));
#36739=CARTESIAN_POINT('Ctrl Pts',(-46.,39.7064029596768,9.94115718202826));
#36740=CARTESIAN_POINT('Ctrl Pts',(-45.9999966732101,39.7069128712589,9.93975069394934));
#36741=CARTESIAN_POINT('Ctrl Pts',(-45.9994167224429,39.7513586367457,9.81712829100708));
#36742=CARTESIAN_POINT('Ctrl Pts',(-45.9741804024558,39.793704872613,9.69777801260392));
#36743=CARTESIAN_POINT('Ctrl Pts',(-45.8908401903906,39.8587623022576,9.51130839381713));
#36744=CARTESIAN_POINT('Ctrl Pts',(-45.8419265836025,39.8831029548383,9.44038249890876));
#36745=CARTESIAN_POINT('Ctrl Pts',(-45.7416688429776,39.9154223669426,9.34548629444458));
#36746=CARTESIAN_POINT('Ctrl Pts',(-45.692683116429,39.9266743500376,9.31215790076818));
#36747=CARTESIAN_POINT('Ctrl Pts',(-45.5938300790286,39.9398264006189,9.27310033615707));
#36748=CARTESIAN_POINT('Ctrl Pts',(-45.5475202328385,39.9429588225849,9.26375507215796));
#36749=CARTESIAN_POINT('Ctrl Pts',(-45.5,39.9429588225849,9.26375507215796));
#36750=CARTESIAN_POINT('',(-46.,45.0056642132324,-4.57019513127084));
#36751=CARTESIAN_POINT('Origin',(-46.,34.999999994595,6.55E-10));
#36752=CARTESIAN_POINT('Ctrl Pts',(-45.5,44.7486243140985,-3.90055430318256));
#36753=CARTESIAN_POINT('Ctrl Pts',(-45.547591906806,44.7486243140985,-3.90055430318256));
#36754=CARTESIAN_POINT('Ctrl Pts',(-45.5939774616156,44.7522730358909,-3.90971545551159));
#36755=CARTESIAN_POINT('Ctrl Pts',(-45.6929687045191,44.7674781615144,-3.94804694909195));
#36756=CARTESIAN_POINT('Ctrl Pts',(-45.7420177519214,44.7804280920619,-3.98076791095232));
#36757=CARTESIAN_POINT('Ctrl Pts',(-45.8422980854956,44.8170645841968,-4.07406216072172));
#36758=CARTESIAN_POINT('Ctrl Pts',(-45.8911666603025,44.8442733910796,-4.14382603215572));
#36759=CARTESIAN_POINT('Ctrl Pts',(-45.974280185293,44.9148993422513,-4.32766254923343));
#36760=CARTESIAN_POINT('Ctrl Pts',(-45.999417856672,44.9595063347814,-4.44561304986796));
#36761=CARTESIAN_POINT('Ctrl Pts',(-45.9999966731511,45.0046273583855,-4.56739570686552));
#36762=CARTESIAN_POINT('Ctrl Pts',(-46.,45.0051458369342,-4.56879540212099));
#36763=CARTESIAN_POINT('Ctrl Pts',(-46.,45.0056642132324,-4.57019513127083));
#36764=CARTESIAN_POINT('Ctrl Pts',(-36.918924746634,26.,0.));
#36765=CARTESIAN_POINT('Ctrl Pts',(-36.7522580799673,26.,5.19615242270663));
#36766=CARTESIAN_POINT('Ctrl Pts',(-36.5855914133007,30.5,7.79422863405995));
#36767=CARTESIAN_POINT('Ctrl Pts',(-36.418924746634,35.,10.3923048454133));
#36768=CARTESIAN_POINT('Ctrl Pts',(-36.2522580799673,39.5,7.79422863405995));
#36769=CARTESIAN_POINT('Ctrl Pts',(-36.0855914133007,44.,5.19615242270663));
#36770=CARTESIAN_POINT('Ctrl Pts',(-35.918924746634,44.,1.10218211923262E-15));
#36771=CARTESIAN_POINT('Ctrl Pts',(-35.7522580799673,44.,-5.19615242270663));
#36772=CARTESIAN_POINT('Ctrl Pts',(-35.5855914133007,39.5,-7.79422863405995));
#36773=CARTESIAN_POINT('Ctrl Pts',(-35.418924746634,35.,-10.3923048454133));
#36774=CARTESIAN_POINT('Ctrl Pts',(-35.2522580799673,30.5,-7.79422863405995));
#36775=CARTESIAN_POINT('Ctrl Pts',(-35.0855914133007,26.,-5.19615242270663));
#36776=CARTESIAN_POINT('Ctrl Pts',(-34.918924746634,26.,0.));
#36777=CARTESIAN_POINT('Ctrl Pts',(-34.7522580799673,26.,5.19615242270663));
#36778=CARTESIAN_POINT('Ctrl Pts',(-34.5855914133007,30.5,7.79422863405995));
#36779=CARTESIAN_POINT('Ctrl Pts',(-34.418924746634,35.,10.3923048454133));
#36780=CARTESIAN_POINT('Ctrl Pts',(-34.2522580799673,39.5,7.79422863405995));
#36781=CARTESIAN_POINT('Ctrl Pts',(-34.0855914133007,44.,5.19615242270663));
#36782=CARTESIAN_POINT('Ctrl Pts',(-33.918924746634,44.,1.10218211923262E-15));
#36783=CARTESIAN_POINT('Ctrl Pts',(-33.7522580799673,44.,-5.19615242270663));
#36784=CARTESIAN_POINT('Ctrl Pts',(-33.5855914133007,39.5,-7.79422863405995));
#36785=CARTESIAN_POINT('Ctrl Pts',(-33.418924746634,35.,-10.3923048454133));
#36786=CARTESIAN_POINT('Ctrl Pts',(-33.2522580799673,30.5,-7.79422863405995));
#36787=CARTESIAN_POINT('Ctrl Pts',(-33.0855914133007,26.,-5.19615242270663));
#36788=CARTESIAN_POINT('Ctrl Pts',(-32.918924746634,26.,0.));
#36789=CARTESIAN_POINT('Ctrl Pts',(-32.7522580799673,26.,5.19615242270663));
#36790=CARTESIAN_POINT('Ctrl Pts',(-32.5855914133007,30.5,7.79422863405995));
#36791=CARTESIAN_POINT('Ctrl Pts',(-32.418924746634,35.,10.3923048454133));
#36792=CARTESIAN_POINT('Ctrl Pts',(-32.2522580799673,39.5,7.79422863405995));
#36793=CARTESIAN_POINT('Ctrl Pts',(-32.0855914133007,44.,5.19615242270663));
#36794=CARTESIAN_POINT('Ctrl Pts',(-31.918924746634,44.,1.10218211923262E-15));
#36795=CARTESIAN_POINT('Ctrl Pts',(-31.7522580799673,44.,-5.19615242270663));
#36796=CARTESIAN_POINT('Ctrl Pts',(-31.5855914133007,39.5,-7.79422863405995));
#36797=CARTESIAN_POINT('Ctrl Pts',(-31.418924746634,35.,-10.3923048454133));
#36798=CARTESIAN_POINT('Ctrl Pts',(-31.2522580799673,30.5,-7.79422863405995));
#36799=CARTESIAN_POINT('Ctrl Pts',(-31.0855914133007,26.,-5.19615242270663));
#36800=CARTESIAN_POINT('Ctrl Pts',(-30.918924746634,26.,0.));
#36801=CARTESIAN_POINT('Ctrl Pts',(-30.7522580799673,26.,5.19615242270663));
#36802=CARTESIAN_POINT('Ctrl Pts',(-30.5855914133007,30.5,7.79422863405995));
#36803=CARTESIAN_POINT('Ctrl Pts',(-30.418924746634,35.,10.3923048454133));
#36804=CARTESIAN_POINT('Ctrl Pts',(-30.2522580799673,39.5,7.79422863405995));
#36805=CARTESIAN_POINT('Ctrl Pts',(-30.0855914133007,44.,5.19615242270663));
#36806=CARTESIAN_POINT('Ctrl Pts',(-29.918924746634,44.,1.10218211923262E-15));
#36807=CARTESIAN_POINT('Ctrl Pts',(-29.7522580799673,44.,-5.19615242270663));
#36808=CARTESIAN_POINT('Ctrl Pts',(-29.5855914133007,39.5,-7.79422863405995));
#36809=CARTESIAN_POINT('Ctrl Pts',(-29.418924746634,35.,-10.3923048454133));
#36810=CARTESIAN_POINT('Ctrl Pts',(-29.2522580799673,30.5,-7.79422863405995));
#36811=CARTESIAN_POINT('Ctrl Pts',(-29.0855914133007,26.,-5.19615242270663));
#36812=CARTESIAN_POINT('Ctrl Pts',(-28.918924746634,26.,0.));
#36813=CARTESIAN_POINT('Ctrl Pts',(-28.7522580799673,26.,5.19615242270663));
#36814=CARTESIAN_POINT('Ctrl Pts',(-28.5855914133007,30.5,7.79422863405995));
#36815=CARTESIAN_POINT('Ctrl Pts',(-28.418924746634,35.,10.3923048454133));
#36816=CARTESIAN_POINT('Ctrl Pts',(-28.2522580799673,39.5,7.79422863405995));
#36817=CARTESIAN_POINT('Ctrl Pts',(-28.0855914133007,44.,5.19615242270663));
#36818=CARTESIAN_POINT('Ctrl Pts',(-27.918924746634,44.,1.10218211923262E-15));
#36819=CARTESIAN_POINT('Ctrl Pts',(-27.7522580799673,44.,-5.19615242270663));
#36820=CARTESIAN_POINT('Ctrl Pts',(-27.5855914133007,39.5,-7.79422863405995));
#36821=CARTESIAN_POINT('Ctrl Pts',(-27.418924746634,35.,-10.3923048454133));
#36822=CARTESIAN_POINT('Ctrl Pts',(-27.2522580799673,30.5,-7.79422863405995));
#36823=CARTESIAN_POINT('Ctrl Pts',(-27.0855914133007,26.,-5.19615242270663));
#36824=CARTESIAN_POINT('Ctrl Pts',(-26.918924746634,26.,0.));
#36825=CARTESIAN_POINT('Ctrl Pts',(-26.7522580799673,26.,5.19615242270663));
#36826=CARTESIAN_POINT('Ctrl Pts',(-26.5855914133007,30.5,7.79422863405995));
#36827=CARTESIAN_POINT('Ctrl Pts',(-26.418924746634,35.,10.3923048454133));
#36828=CARTESIAN_POINT('Ctrl Pts',(-26.2522580799673,39.5,7.79422863405995));
#36829=CARTESIAN_POINT('Ctrl Pts',(-26.0855914133007,44.,5.19615242270663));
#36830=CARTESIAN_POINT('Ctrl Pts',(-25.918924746634,44.,1.10218211923262E-15));
#36831=CARTESIAN_POINT('Ctrl Pts',(-25.7522580799673,44.,-5.19615242270663));
#36832=CARTESIAN_POINT('Ctrl Pts',(-25.5855914133007,39.5,-7.79422863405995));
#36833=CARTESIAN_POINT('Ctrl Pts',(-25.418924746634,35.,-10.3923048454133));
#36834=CARTESIAN_POINT('Ctrl Pts',(-25.2522580799673,30.5,-7.79422863405995));
#36835=CARTESIAN_POINT('Ctrl Pts',(-25.0855914133007,26.,-5.19615242270663));
#36836=CARTESIAN_POINT('Ctrl Pts',(-24.918924746634,26.,0.));
#36837=CARTESIAN_POINT('Ctrl Pts',(-24.7522580799673,26.,5.19615242270663));
#36838=CARTESIAN_POINT('Ctrl Pts',(-24.5855914133007,30.5,7.79422863405995));
#36839=CARTESIAN_POINT('Ctrl Pts',(-24.418924746634,35.,10.3923048454133));
#36840=CARTESIAN_POINT('Ctrl Pts',(-24.2522580799673,39.5,7.79422863405995));
#36841=CARTESIAN_POINT('Ctrl Pts',(-24.0855914133007,44.,5.19615242270663));
#36842=CARTESIAN_POINT('Ctrl Pts',(-23.918924746634,44.,1.10218211923262E-15));
#36843=CARTESIAN_POINT('Ctrl Pts',(-23.7522580799673,44.,-5.19615242270663));
#36844=CARTESIAN_POINT('Ctrl Pts',(-23.5855914133007,39.5,-7.79422863405995));
#36845=CARTESIAN_POINT('Ctrl Pts',(-23.418924746634,35.,-10.3923048454133));
#36846=CARTESIAN_POINT('Ctrl Pts',(-23.2522580799673,30.5,-7.79422863405995));
#36847=CARTESIAN_POINT('Ctrl Pts',(-23.0855914133007,26.,-5.19615242270663));
#36848=CARTESIAN_POINT('Ctrl Pts',(-22.918924746634,26.,0.));
#36849=CARTESIAN_POINT('Ctrl Pts',(-22.7522580799673,26.,5.19615242270663));
#36850=CARTESIAN_POINT('Ctrl Pts',(-22.5855914133007,30.5,7.79422863405995));
#36851=CARTESIAN_POINT('Ctrl Pts',(-22.418924746634,35.,10.3923048454133));
#36852=CARTESIAN_POINT('Ctrl Pts',(-22.2522580799674,39.5,7.79422863405995));
#36853=CARTESIAN_POINT('Ctrl Pts',(-22.0855914133007,44.,5.19615242270663));
#36854=CARTESIAN_POINT('Ctrl Pts',(-21.918924746634,44.,1.10218211923262E-15));
#36855=CARTESIAN_POINT('Ctrl Pts',(-21.7522580799673,44.,-5.19615242270663));
#36856=CARTESIAN_POINT('Ctrl Pts',(-21.5855914133006,39.5,-7.79422863405995));
#36857=CARTESIAN_POINT('Ctrl Pts',(-21.418924746634,35.,-10.3923048454133));
#36858=CARTESIAN_POINT('Ctrl Pts',(-21.2522580799673,30.5,-7.79422863405995));
#36859=CARTESIAN_POINT('Ctrl Pts',(-21.0855914133007,26.,-5.19615242270663));
#36860=CARTESIAN_POINT('Ctrl Pts',(-20.918924746634,26.,0.));
#36861=CARTESIAN_POINT('Ctrl Pts',(-20.7522580799673,26.,5.19615242270663));
#36862=CARTESIAN_POINT('Ctrl Pts',(-20.5855914133006,30.5,7.79422863405995));
#36863=CARTESIAN_POINT('Ctrl Pts',(-20.418924746634,35.,10.3923048454133));
#36864=CARTESIAN_POINT('Ctrl Pts',(-20.2522580799673,39.5,7.79422863405995));
#36865=CARTESIAN_POINT('Ctrl Pts',(-20.0855914133007,44.,5.19615242270663));
#36866=CARTESIAN_POINT('Ctrl Pts',(-19.918924746634,44.,1.10218211923262E-15));
#36867=CARTESIAN_POINT('Ctrl Pts',(-19.7522580799674,44.,-5.19615242270663));
#36868=CARTESIAN_POINT('Ctrl Pts',(-19.5855914133006,39.5,-7.79422863405995));
#36869=CARTESIAN_POINT('Ctrl Pts',(-19.418924746634,35.,-10.3923048454133));
#36870=CARTESIAN_POINT('Ctrl Pts',(-19.2522580799674,30.5,-7.79422863405995));
#36871=CARTESIAN_POINT('Ctrl Pts',(-19.0855914133007,26.,-5.19615242270663));
#36872=CARTESIAN_POINT('Ctrl Pts',(-18.918924746634,26.,0.));
#36873=CARTESIAN_POINT('Ctrl Pts',(-18.7522580799673,26.,5.19615242270663));
#36874=CARTESIAN_POINT('Ctrl Pts',(-18.5855914133006,30.5,7.79422863405995));
#36875=CARTESIAN_POINT('Ctrl Pts',(-18.418924746634,35.,10.3923048454133));
#36876=CARTESIAN_POINT('Ctrl Pts',(-18.2522580799673,39.5,7.79422863405995));
#36877=CARTESIAN_POINT('Ctrl Pts',(-18.0855914133006,44.,5.19615242270663));
#36878=CARTESIAN_POINT('Ctrl Pts',(-17.918924746634,44.,1.10218211923262E-15));
#36879=CARTESIAN_POINT('Ctrl Pts',(-17.7522580799673,44.,-5.19615242270663));
#36880=CARTESIAN_POINT('Ctrl Pts',(-17.5855914133006,39.5,-7.79422863405995));
#36881=CARTESIAN_POINT('Ctrl Pts',(-17.418924746634,35.,-10.3923048454133));
#36882=CARTESIAN_POINT('Ctrl Pts',(-17.2522580799673,30.5,-7.79422863405995));
#36883=CARTESIAN_POINT('Ctrl Pts',(-17.0855914133007,26.,-5.19615242270663));
#36884=CARTESIAN_POINT('Ctrl Pts',(-16.918924746634,26.,0.));
#36885=CARTESIAN_POINT('Ctrl Pts',(-36.918924746634,24.4,0.));
#36886=CARTESIAN_POINT('Ctrl Pts',(-36.7522580799673,24.4,6.11991285341003));
#36887=CARTESIAN_POINT('Ctrl Pts',(-36.5855914133007,29.7,9.17986928011504));
#36888=CARTESIAN_POINT('Ctrl Pts',(-36.418924746634,35.,12.2398257068201));
#36889=CARTESIAN_POINT('Ctrl Pts',(-36.2522580799673,40.3,9.17986928011504));
#36890=CARTESIAN_POINT('Ctrl Pts',(-36.0855914133007,45.6,6.11991285341004));
#36891=CARTESIAN_POINT('Ctrl Pts',(-35.918924746634,45.6,1.29812560709619E-15));
#36892=CARTESIAN_POINT('Ctrl Pts',(-35.7522580799673,45.6,-6.11991285341003));
#36893=CARTESIAN_POINT('Ctrl Pts',(-35.5855914133007,40.3,-9.17986928011504));
#36894=CARTESIAN_POINT('Ctrl Pts',(-35.418924746634,35.,-12.2398257068201));
#36895=CARTESIAN_POINT('Ctrl Pts',(-35.2522580799673,29.7,-9.17986928011506));
#36896=CARTESIAN_POINT('Ctrl Pts',(-35.0855914133007,24.4,-6.11991285341004));
#36897=CARTESIAN_POINT('Ctrl Pts',(-34.918924746634,24.4,0.));
#36898=CARTESIAN_POINT('Ctrl Pts',(-34.7522580799673,24.4,6.11991285341003));
#36899=CARTESIAN_POINT('Ctrl Pts',(-34.5855914133007,29.7,9.17986928011504));
#36900=CARTESIAN_POINT('Ctrl Pts',(-34.418924746634,35.,12.2398257068201));
#36901=CARTESIAN_POINT('Ctrl Pts',(-34.2522580799673,40.3,9.17986928011504));
#36902=CARTESIAN_POINT('Ctrl Pts',(-34.0855914133007,45.6,6.11991285341004));
#36903=CARTESIAN_POINT('Ctrl Pts',(-33.918924746634,45.6,1.29812560709619E-15));
#36904=CARTESIAN_POINT('Ctrl Pts',(-33.7522580799673,45.6,-6.11991285341003));
#36905=CARTESIAN_POINT('Ctrl Pts',(-33.5855914133007,40.3,-9.17986928011504));
#36906=CARTESIAN_POINT('Ctrl Pts',(-33.418924746634,35.,-12.2398257068201));
#36907=CARTESIAN_POINT('Ctrl Pts',(-33.2522580799673,29.7,-9.17986928011506));
#36908=CARTESIAN_POINT('Ctrl Pts',(-33.0855914133007,24.4,-6.11991285341004));
#36909=CARTESIAN_POINT('Ctrl Pts',(-32.918924746634,24.4,0.));
#36910=CARTESIAN_POINT('Ctrl Pts',(-32.7522580799673,24.4,6.11991285341003));
#36911=CARTESIAN_POINT('Ctrl Pts',(-32.5855914133007,29.7,9.17986928011504));
#36912=CARTESIAN_POINT('Ctrl Pts',(-32.418924746634,35.,12.2398257068201));
#36913=CARTESIAN_POINT('Ctrl Pts',(-32.2522580799673,40.3,9.17986928011504));
#36914=CARTESIAN_POINT('Ctrl Pts',(-32.0855914133007,45.6,6.11991285341004));
#36915=CARTESIAN_POINT('Ctrl Pts',(-31.918924746634,45.6,1.29812560709619E-15));
#36916=CARTESIAN_POINT('Ctrl Pts',(-31.7522580799673,45.6,-6.11991285341003));
#36917=CARTESIAN_POINT('Ctrl Pts',(-31.5855914133007,40.3,-9.17986928011504));
#36918=CARTESIAN_POINT('Ctrl Pts',(-31.418924746634,35.,-12.2398257068201));
#36919=CARTESIAN_POINT('Ctrl Pts',(-31.2522580799673,29.7,-9.17986928011506));
#36920=CARTESIAN_POINT('Ctrl Pts',(-31.0855914133007,24.4,-6.11991285341004));
#36921=CARTESIAN_POINT('Ctrl Pts',(-30.918924746634,24.4,0.));
#36922=CARTESIAN_POINT('Ctrl Pts',(-30.7522580799673,24.4,6.11991285341003));
#36923=CARTESIAN_POINT('Ctrl Pts',(-30.5855914133007,29.7,9.17986928011504));
#36924=CARTESIAN_POINT('Ctrl Pts',(-30.418924746634,35.,12.2398257068201));
#36925=CARTESIAN_POINT('Ctrl Pts',(-30.2522580799673,40.3,9.17986928011504));
#36926=CARTESIAN_POINT('Ctrl Pts',(-30.0855914133007,45.6,6.11991285341004));
#36927=CARTESIAN_POINT('Ctrl Pts',(-29.918924746634,45.6,1.29812560709619E-15));
#36928=CARTESIAN_POINT('Ctrl Pts',(-29.7522580799673,45.6,-6.11991285341003));
#36929=CARTESIAN_POINT('Ctrl Pts',(-29.5855914133007,40.3,-9.17986928011504));
#36930=CARTESIAN_POINT('Ctrl Pts',(-29.418924746634,35.,-12.2398257068201));
#36931=CARTESIAN_POINT('Ctrl Pts',(-29.2522580799673,29.7,-9.17986928011506));
#36932=CARTESIAN_POINT('Ctrl Pts',(-29.0855914133007,24.4,-6.11991285341004));
#36933=CARTESIAN_POINT('Ctrl Pts',(-28.918924746634,24.4,0.));
#36934=CARTESIAN_POINT('Ctrl Pts',(-28.7522580799673,24.4,6.11991285341003));
#36935=CARTESIAN_POINT('Ctrl Pts',(-28.5855914133007,29.7,9.17986928011504));
#36936=CARTESIAN_POINT('Ctrl Pts',(-28.418924746634,35.,12.2398257068201));
#36937=CARTESIAN_POINT('Ctrl Pts',(-28.2522580799673,40.3,9.17986928011504));
#36938=CARTESIAN_POINT('Ctrl Pts',(-28.0855914133007,45.6,6.11991285341004));
#36939=CARTESIAN_POINT('Ctrl Pts',(-27.918924746634,45.6,1.29812560709619E-15));
#36940=CARTESIAN_POINT('Ctrl Pts',(-27.7522580799673,45.6,-6.11991285341003));
#36941=CARTESIAN_POINT('Ctrl Pts',(-27.5855914133007,40.3,-9.17986928011504));
#36942=CARTESIAN_POINT('Ctrl Pts',(-27.418924746634,35.,-12.2398257068201));
#36943=CARTESIAN_POINT('Ctrl Pts',(-27.2522580799673,29.7,-9.17986928011506));
#36944=CARTESIAN_POINT('Ctrl Pts',(-27.0855914133007,24.4,-6.11991285341004));
#36945=CARTESIAN_POINT('Ctrl Pts',(-26.918924746634,24.4,0.));
#36946=CARTESIAN_POINT('Ctrl Pts',(-26.7522580799673,24.4,6.11991285341003));
#36947=CARTESIAN_POINT('Ctrl Pts',(-26.5855914133007,29.7,9.17986928011504));
#36948=CARTESIAN_POINT('Ctrl Pts',(-26.418924746634,35.,12.2398257068201));
#36949=CARTESIAN_POINT('Ctrl Pts',(-26.2522580799673,40.3,9.17986928011504));
#36950=CARTESIAN_POINT('Ctrl Pts',(-26.0855914133007,45.6,6.11991285341004));
#36951=CARTESIAN_POINT('Ctrl Pts',(-25.918924746634,45.6,1.29812560709619E-15));
#36952=CARTESIAN_POINT('Ctrl Pts',(-25.7522580799673,45.6,-6.11991285341003));
#36953=CARTESIAN_POINT('Ctrl Pts',(-25.5855914133007,40.3,-9.17986928011504));
#36954=CARTESIAN_POINT('Ctrl Pts',(-25.418924746634,35.,-12.2398257068201));
#36955=CARTESIAN_POINT('Ctrl Pts',(-25.2522580799673,29.7,-9.17986928011506));
#36956=CARTESIAN_POINT('Ctrl Pts',(-25.0855914133007,24.4,-6.11991285341004));
#36957=CARTESIAN_POINT('Ctrl Pts',(-24.918924746634,24.4,0.));
#36958=CARTESIAN_POINT('Ctrl Pts',(-24.7522580799673,24.4,6.11991285341003));
#36959=CARTESIAN_POINT('Ctrl Pts',(-24.5855914133007,29.7,9.17986928011504));
#36960=CARTESIAN_POINT('Ctrl Pts',(-24.418924746634,35.,12.2398257068201));
#36961=CARTESIAN_POINT('Ctrl Pts',(-24.2522580799673,40.3,9.17986928011504));
#36962=CARTESIAN_POINT('Ctrl Pts',(-24.0855914133007,45.6,6.11991285341004));
#36963=CARTESIAN_POINT('Ctrl Pts',(-23.918924746634,45.6,1.29812560709619E-15));
#36964=CARTESIAN_POINT('Ctrl Pts',(-23.7522580799673,45.6,-6.11991285341003));
#36965=CARTESIAN_POINT('Ctrl Pts',(-23.5855914133007,40.3,-9.17986928011504));
#36966=CARTESIAN_POINT('Ctrl Pts',(-23.418924746634,35.,-12.2398257068201));
#36967=CARTESIAN_POINT('Ctrl Pts',(-23.2522580799673,29.7,-9.17986928011506));
#36968=CARTESIAN_POINT('Ctrl Pts',(-23.0855914133007,24.4,-6.11991285341004));
#36969=CARTESIAN_POINT('Ctrl Pts',(-22.918924746634,24.4,0.));
#36970=CARTESIAN_POINT('Ctrl Pts',(-22.7522580799673,24.4,6.11991285341003));
#36971=CARTESIAN_POINT('Ctrl Pts',(-22.5855914133007,29.7,9.17986928011504));
#36972=CARTESIAN_POINT('Ctrl Pts',(-22.418924746634,35.,12.2398257068201));
#36973=CARTESIAN_POINT('Ctrl Pts',(-22.2522580799673,40.3,9.17986928011504));
#36974=CARTESIAN_POINT('Ctrl Pts',(-22.0855914133007,45.6,6.11991285341004));
#36975=CARTESIAN_POINT('Ctrl Pts',(-21.918924746634,45.6,1.29812560709619E-15));
#36976=CARTESIAN_POINT('Ctrl Pts',(-21.7522580799673,45.6,-6.11991285341003));
#36977=CARTESIAN_POINT('Ctrl Pts',(-21.5855914133007,40.3,-9.17986928011504));
#36978=CARTESIAN_POINT('Ctrl Pts',(-21.418924746634,35.,-12.2398257068201));
#36979=CARTESIAN_POINT('Ctrl Pts',(-21.2522580799673,29.7,-9.17986928011506));
#36980=CARTESIAN_POINT('Ctrl Pts',(-21.0855914133007,24.4,-6.11991285341004));
#36981=CARTESIAN_POINT('Ctrl Pts',(-20.918924746634,24.4,0.));
#36982=CARTESIAN_POINT('Ctrl Pts',(-20.7522580799673,24.4,6.11991285341003));
#36983=CARTESIAN_POINT('Ctrl Pts',(-20.5855914133007,29.7,9.17986928011504));
#36984=CARTESIAN_POINT('Ctrl Pts',(-20.418924746634,35.,12.2398257068201));
#36985=CARTESIAN_POINT('Ctrl Pts',(-20.2522580799673,40.3,9.17986928011504));
#36986=CARTESIAN_POINT('Ctrl Pts',(-20.0855914133007,45.6,6.11991285341004));
#36987=CARTESIAN_POINT('Ctrl Pts',(-19.918924746634,45.6,1.29812560709619E-15));
#36988=CARTESIAN_POINT('Ctrl Pts',(-19.7522580799673,45.6,-6.11991285341003));
#36989=CARTESIAN_POINT('Ctrl Pts',(-19.5855914133007,40.3,-9.17986928011504));
#36990=CARTESIAN_POINT('Ctrl Pts',(-19.418924746634,35.,-12.2398257068201));
#36991=CARTESIAN_POINT('Ctrl Pts',(-19.2522580799673,29.7,-9.17986928011506));
#36992=CARTESIAN_POINT('Ctrl Pts',(-19.0855914133006,24.4,-6.11991285341004));
#36993=CARTESIAN_POINT('Ctrl Pts',(-18.918924746634,24.4,0.));
#36994=CARTESIAN_POINT('Ctrl Pts',(-18.7522580799673,24.4,6.11991285341003));
#36995=CARTESIAN_POINT('Ctrl Pts',(-18.5855914133007,29.7,9.17986928011504));
#36996=CARTESIAN_POINT('Ctrl Pts',(-18.418924746634,35.,12.2398257068201));
#36997=CARTESIAN_POINT('Ctrl Pts',(-18.2522580799673,40.3,9.17986928011504));
#36998=CARTESIAN_POINT('Ctrl Pts',(-18.0855914133007,45.6,6.11991285341004));
#36999=CARTESIAN_POINT('Ctrl Pts',(-17.918924746634,45.6,1.29812560709619E-15));
#37000=CARTESIAN_POINT('Ctrl Pts',(-17.7522580799674,45.6,-6.11991285341003));
#37001=CARTESIAN_POINT('Ctrl Pts',(-17.5855914133007,40.3,-9.17986928011504));
#37002=CARTESIAN_POINT('Ctrl Pts',(-17.418924746634,35.,-12.2398257068201));
#37003=CARTESIAN_POINT('Ctrl Pts',(-17.2522580799674,29.7,-9.17986928011506));
#37004=CARTESIAN_POINT('Ctrl Pts',(-17.0855914133007,24.4,-6.11991285341004));
#37005=CARTESIAN_POINT('Ctrl Pts',(-16.918924746634,24.4,0.));
#37006=CARTESIAN_POINT('Ctrl Pts',(-38.518924746634,24.4,0.));
#37007=CARTESIAN_POINT('Ctrl Pts',(-38.3522580799673,24.4,6.11991285341003));
#37008=CARTESIAN_POINT('Ctrl Pts',(-38.1855914133007,29.7,9.17986928011504));
#37009=CARTESIAN_POINT('Ctrl Pts',(-38.018924746634,35.,12.2398257068201));
#37010=CARTESIAN_POINT('Ctrl Pts',(-37.8522580799673,40.3,9.17986928011504));
#37011=CARTESIAN_POINT('Ctrl Pts',(-37.6855914133007,45.6,6.11991285341004));
#37012=CARTESIAN_POINT('Ctrl Pts',(-37.518924746634,45.6,1.29812560709619E-15));
#37013=CARTESIAN_POINT('Ctrl Pts',(-37.3522580799673,45.6,-6.11991285341003));
#37014=CARTESIAN_POINT('Ctrl Pts',(-37.1855914133007,40.3,-9.17986928011504));
#37015=CARTESIAN_POINT('Ctrl Pts',(-37.018924746634,35.,-12.2398257068201));
#37016=CARTESIAN_POINT('Ctrl Pts',(-36.8522580799673,29.7,-9.17986928011506));
#37017=CARTESIAN_POINT('Ctrl Pts',(-36.6855914133007,24.4,-6.11991285341004));
#37018=CARTESIAN_POINT('Ctrl Pts',(-36.518924746634,24.4,0.));
#37019=CARTESIAN_POINT('Ctrl Pts',(-36.3522580799673,24.4,6.11991285341003));
#37020=CARTESIAN_POINT('Ctrl Pts',(-36.1855914133007,29.7,9.17986928011504));
#37021=CARTESIAN_POINT('Ctrl Pts',(-36.018924746634,35.,12.2398257068201));
#37022=CARTESIAN_POINT('Ctrl Pts',(-35.8522580799673,40.3,9.17986928011504));
#37023=CARTESIAN_POINT('Ctrl Pts',(-35.6855914133007,45.6,6.11991285341004));
#37024=CARTESIAN_POINT('Ctrl Pts',(-35.518924746634,45.6,1.29812560709619E-15));
#37025=CARTESIAN_POINT('Ctrl Pts',(-35.3522580799673,45.6,-6.11991285341003));
#37026=CARTESIAN_POINT('Ctrl Pts',(-35.1855914133007,40.3,-9.17986928011504));
#37027=CARTESIAN_POINT('Ctrl Pts',(-35.018924746634,35.,-12.2398257068201));
#37028=CARTESIAN_POINT('Ctrl Pts',(-34.8522580799673,29.7,-9.17986928011506));
#37029=CARTESIAN_POINT('Ctrl Pts',(-34.6855914133007,24.4,-6.11991285341004));
#37030=CARTESIAN_POINT('Ctrl Pts',(-34.518924746634,24.4,0.));
#37031=CARTESIAN_POINT('Ctrl Pts',(-34.3522580799673,24.4,6.11991285341003));
#37032=CARTESIAN_POINT('Ctrl Pts',(-34.1855914133007,29.7,9.17986928011504));
#37033=CARTESIAN_POINT('Ctrl Pts',(-34.018924746634,35.,12.2398257068201));
#37034=CARTESIAN_POINT('Ctrl Pts',(-33.8522580799673,40.3,9.17986928011504));
#37035=CARTESIAN_POINT('Ctrl Pts',(-33.6855914133007,45.6,6.11991285341004));
#37036=CARTESIAN_POINT('Ctrl Pts',(-33.518924746634,45.6,1.29812560709619E-15));
#37037=CARTESIAN_POINT('Ctrl Pts',(-33.3522580799673,45.6,-6.11991285341003));
#37038=CARTESIAN_POINT('Ctrl Pts',(-33.1855914133007,40.3,-9.17986928011504));
#37039=CARTESIAN_POINT('Ctrl Pts',(-33.018924746634,35.,-12.2398257068201));
#37040=CARTESIAN_POINT('Ctrl Pts',(-32.8522580799673,29.7,-9.17986928011506));
#37041=CARTESIAN_POINT('Ctrl Pts',(-32.6855914133007,24.4,-6.11991285341004));
#37042=CARTESIAN_POINT('Ctrl Pts',(-32.518924746634,24.4,0.));
#37043=CARTESIAN_POINT('Ctrl Pts',(-32.3522580799673,24.4,6.11991285341003));
#37044=CARTESIAN_POINT('Ctrl Pts',(-32.1855914133007,29.7,9.17986928011504));
#37045=CARTESIAN_POINT('Ctrl Pts',(-32.018924746634,35.,12.2398257068201));
#37046=CARTESIAN_POINT('Ctrl Pts',(-31.8522580799674,40.3,9.17986928011504));
#37047=CARTESIAN_POINT('Ctrl Pts',(-31.6855914133007,45.6,6.11991285341004));
#37048=CARTESIAN_POINT('Ctrl Pts',(-31.518924746634,45.6,1.29812560709619E-15));
#37049=CARTESIAN_POINT('Ctrl Pts',(-31.3522580799673,45.6,-6.11991285341003));
#37050=CARTESIAN_POINT('Ctrl Pts',(-31.1855914133007,40.3,-9.17986928011504));
#37051=CARTESIAN_POINT('Ctrl Pts',(-31.018924746634,35.,-12.2398257068201));
#37052=CARTESIAN_POINT('Ctrl Pts',(-30.8522580799673,29.7,-9.17986928011506));
#37053=CARTESIAN_POINT('Ctrl Pts',(-30.6855914133007,24.4,-6.11991285341004));
#37054=CARTESIAN_POINT('Ctrl Pts',(-30.518924746634,24.4,0.));
#37055=CARTESIAN_POINT('Ctrl Pts',(-30.3522580799673,24.4,6.11991285341003));
#37056=CARTESIAN_POINT('Ctrl Pts',(-30.1855914133007,29.7,9.17986928011504));
#37057=CARTESIAN_POINT('Ctrl Pts',(-30.018924746634,35.,12.2398257068201));
#37058=CARTESIAN_POINT('Ctrl Pts',(-29.8522580799673,40.3,9.17986928011504));
#37059=CARTESIAN_POINT('Ctrl Pts',(-29.6855914133007,45.6,6.11991285341004));
#37060=CARTESIAN_POINT('Ctrl Pts',(-29.518924746634,45.6,1.29812560709619E-15));
#37061=CARTESIAN_POINT('Ctrl Pts',(-29.3522580799673,45.6,-6.11991285341003));
#37062=CARTESIAN_POINT('Ctrl Pts',(-29.1855914133007,40.3,-9.17986928011504));
#37063=CARTESIAN_POINT('Ctrl Pts',(-29.018924746634,35.,-12.2398257068201));
#37064=CARTESIAN_POINT('Ctrl Pts',(-28.8522580799673,29.7,-9.17986928011506));
#37065=CARTESIAN_POINT('Ctrl Pts',(-28.6855914133007,24.4,-6.11991285341004));
#37066=CARTESIAN_POINT('Ctrl Pts',(-28.518924746634,24.4,0.));
#37067=CARTESIAN_POINT('Ctrl Pts',(-28.3522580799673,24.4,6.11991285341003));
#37068=CARTESIAN_POINT('Ctrl Pts',(-28.1855914133007,29.7,9.17986928011504));
#37069=CARTESIAN_POINT('Ctrl Pts',(-28.018924746634,35.,12.2398257068201));
#37070=CARTESIAN_POINT('Ctrl Pts',(-27.8522580799673,40.3,9.17986928011504));
#37071=CARTESIAN_POINT('Ctrl Pts',(-27.6855914133007,45.6,6.11991285341004));
#37072=CARTESIAN_POINT('Ctrl Pts',(-27.518924746634,45.6,1.29812560709619E-15));
#37073=CARTESIAN_POINT('Ctrl Pts',(-27.3522580799673,45.6,-6.11991285341003));
#37074=CARTESIAN_POINT('Ctrl Pts',(-27.1855914133007,40.3,-9.17986928011504));
#37075=CARTESIAN_POINT('Ctrl Pts',(-27.018924746634,35.,-12.2398257068201));
#37076=CARTESIAN_POINT('Ctrl Pts',(-26.8522580799673,29.7,-9.17986928011506));
#37077=CARTESIAN_POINT('Ctrl Pts',(-26.6855914133007,24.4,-6.11991285341004));
#37078=CARTESIAN_POINT('Ctrl Pts',(-26.518924746634,24.4,0.));
#37079=CARTESIAN_POINT('Ctrl Pts',(-26.3522580799673,24.4,6.11991285341003));
#37080=CARTESIAN_POINT('Ctrl Pts',(-26.1855914133007,29.7,9.17986928011504));
#37081=CARTESIAN_POINT('Ctrl Pts',(-26.018924746634,35.,12.2398257068201));
#37082=CARTESIAN_POINT('Ctrl Pts',(-25.8522580799673,40.3,9.17986928011504));
#37083=CARTESIAN_POINT('Ctrl Pts',(-25.6855914133007,45.6,6.11991285341004));
#37084=CARTESIAN_POINT('Ctrl Pts',(-25.518924746634,45.6,1.29812560709619E-15));
#37085=CARTESIAN_POINT('Ctrl Pts',(-25.3522580799673,45.6,-6.11991285341003));
#37086=CARTESIAN_POINT('Ctrl Pts',(-25.1855914133007,40.3,-9.17986928011504));
#37087=CARTESIAN_POINT('Ctrl Pts',(-25.018924746634,35.,-12.2398257068201));
#37088=CARTESIAN_POINT('Ctrl Pts',(-24.8522580799673,29.7,-9.17986928011506));
#37089=CARTESIAN_POINT('Ctrl Pts',(-24.6855914133007,24.4,-6.11991285341004));
#37090=CARTESIAN_POINT('Ctrl Pts',(-24.518924746634,24.4,0.));
#37091=CARTESIAN_POINT('Ctrl Pts',(-24.3522580799673,24.4,6.11991285341003));
#37092=CARTESIAN_POINT('Ctrl Pts',(-24.1855914133007,29.7,9.17986928011504));
#37093=CARTESIAN_POINT('Ctrl Pts',(-24.018924746634,35.,12.2398257068201));
#37094=CARTESIAN_POINT('Ctrl Pts',(-23.8522580799674,40.3,9.17986928011504));
#37095=CARTESIAN_POINT('Ctrl Pts',(-23.6855914133007,45.6,6.11991285341004));
#37096=CARTESIAN_POINT('Ctrl Pts',(-23.518924746634,45.6,1.29812560709619E-15));
#37097=CARTESIAN_POINT('Ctrl Pts',(-23.3522580799673,45.6,-6.11991285341003));
#37098=CARTESIAN_POINT('Ctrl Pts',(-23.1855914133007,40.3,-9.17986928011504));
#37099=CARTESIAN_POINT('Ctrl Pts',(-23.018924746634,35.,-12.2398257068201));
#37100=CARTESIAN_POINT('Ctrl Pts',(-22.8522580799673,29.7,-9.17986928011506));
#37101=CARTESIAN_POINT('Ctrl Pts',(-22.6855914133007,24.4,-6.11991285341004));
#37102=CARTESIAN_POINT('Ctrl Pts',(-22.518924746634,24.4,0.));
#37103=CARTESIAN_POINT('Ctrl Pts',(-22.3522580799673,24.4,6.11991285341003));
#37104=CARTESIAN_POINT('Ctrl Pts',(-22.1855914133007,29.7,9.17986928011504));
#37105=CARTESIAN_POINT('Ctrl Pts',(-22.018924746634,35.,12.2398257068201));
#37106=CARTESIAN_POINT('Ctrl Pts',(-21.8522580799673,40.3,9.17986928011504));
#37107=CARTESIAN_POINT('Ctrl Pts',(-21.6855914133007,45.6,6.11991285341004));
#37108=CARTESIAN_POINT('Ctrl Pts',(-21.518924746634,45.6,1.29812560709619E-15));
#37109=CARTESIAN_POINT('Ctrl Pts',(-21.3522580799673,45.6,-6.11991285341003));
#37110=CARTESIAN_POINT('Ctrl Pts',(-21.1855914133007,40.3,-9.17986928011504));
#37111=CARTESIAN_POINT('Ctrl Pts',(-21.018924746634,35.,-12.2398257068201));
#37112=CARTESIAN_POINT('Ctrl Pts',(-20.8522580799674,29.7,-9.17986928011506));
#37113=CARTESIAN_POINT('Ctrl Pts',(-20.6855914133006,24.4,-6.11991285341004));
#37114=CARTESIAN_POINT('Ctrl Pts',(-20.518924746634,24.4,0.));
#37115=CARTESIAN_POINT('Ctrl Pts',(-20.3522580799673,24.4,6.11991285341003));
#37116=CARTESIAN_POINT('Ctrl Pts',(-20.1855914133007,29.7,9.17986928011504));
#37117=CARTESIAN_POINT('Ctrl Pts',(-20.018924746634,35.,12.2398257068201));
#37118=CARTESIAN_POINT('Ctrl Pts',(-19.8522580799673,40.3,9.17986928011504));
#37119=CARTESIAN_POINT('Ctrl Pts',(-19.6855914133007,45.6,6.11991285341004));
#37120=CARTESIAN_POINT('Ctrl Pts',(-19.518924746634,45.6,1.29812560709619E-15));
#37121=CARTESIAN_POINT('Ctrl Pts',(-19.3522580799673,45.6,-6.11991285341003));
#37122=CARTESIAN_POINT('Ctrl Pts',(-19.1855914133007,40.3,-9.17986928011504));
#37123=CARTESIAN_POINT('Ctrl Pts',(-19.018924746634,35.,-12.2398257068201));
#37124=CARTESIAN_POINT('Ctrl Pts',(-18.8522580799673,29.7,-9.17986928011506));
#37125=CARTESIAN_POINT('Ctrl Pts',(-18.6855914133007,24.4,-6.11991285341004));
#37126=CARTESIAN_POINT('Ctrl Pts',(-18.518924746634,24.4,0.));
#37127=CARTESIAN_POINT('Ctrl Pts',(-38.518924746634,26.,0.));
#37128=CARTESIAN_POINT('Ctrl Pts',(-38.3522580799673,26.,5.19615242270663));
#37129=CARTESIAN_POINT('Ctrl Pts',(-38.1855914133007,30.5,7.79422863405995));
#37130=CARTESIAN_POINT('Ctrl Pts',(-38.018924746634,35.,10.3923048454133));
#37131=CARTESIAN_POINT('Ctrl Pts',(-37.8522580799673,39.5,7.79422863405995));
#37132=CARTESIAN_POINT('Ctrl Pts',(-37.6855914133007,44.,5.19615242270663));
#37133=CARTESIAN_POINT('Ctrl Pts',(-37.518924746634,44.,1.10218211923262E-15));
#37134=CARTESIAN_POINT('Ctrl Pts',(-37.3522580799673,44.,-5.19615242270663));
#37135=CARTESIAN_POINT('Ctrl Pts',(-37.1855914133007,39.5,-7.79422863405995));
#37136=CARTESIAN_POINT('Ctrl Pts',(-37.018924746634,35.,-10.3923048454133));
#37137=CARTESIAN_POINT('Ctrl Pts',(-36.8522580799673,30.5,-7.79422863405995));
#37138=CARTESIAN_POINT('Ctrl Pts',(-36.6855914133007,26.,-5.19615242270663));
#37139=CARTESIAN_POINT('Ctrl Pts',(-36.518924746634,26.,0.));
#37140=CARTESIAN_POINT('Ctrl Pts',(-36.3522580799673,26.,5.19615242270663));
#37141=CARTESIAN_POINT('Ctrl Pts',(-36.1855914133007,30.5,7.79422863405995));
#37142=CARTESIAN_POINT('Ctrl Pts',(-36.018924746634,35.,10.3923048454133));
#37143=CARTESIAN_POINT('Ctrl Pts',(-35.8522580799673,39.5,7.79422863405995));
#37144=CARTESIAN_POINT('Ctrl Pts',(-35.6855914133007,44.,5.19615242270663));
#37145=CARTESIAN_POINT('Ctrl Pts',(-35.518924746634,44.,1.10218211923262E-15));
#37146=CARTESIAN_POINT('Ctrl Pts',(-35.3522580799673,44.,-5.19615242270663));
#37147=CARTESIAN_POINT('Ctrl Pts',(-35.1855914133007,39.5,-7.79422863405995));
#37148=CARTESIAN_POINT('Ctrl Pts',(-35.018924746634,35.,-10.3923048454133));
#37149=CARTESIAN_POINT('Ctrl Pts',(-34.8522580799673,30.5,-7.79422863405995));
#37150=CARTESIAN_POINT('Ctrl Pts',(-34.6855914133007,26.,-5.19615242270663));
#37151=CARTESIAN_POINT('Ctrl Pts',(-34.518924746634,26.,0.));
#37152=CARTESIAN_POINT('Ctrl Pts',(-34.3522580799673,26.,5.19615242270663));
#37153=CARTESIAN_POINT('Ctrl Pts',(-34.1855914133007,30.5,7.79422863405995));
#37154=CARTESIAN_POINT('Ctrl Pts',(-34.018924746634,35.,10.3923048454133));
#37155=CARTESIAN_POINT('Ctrl Pts',(-33.8522580799673,39.5,7.79422863405995));
#37156=CARTESIAN_POINT('Ctrl Pts',(-33.6855914133007,44.,5.19615242270663));
#37157=CARTESIAN_POINT('Ctrl Pts',(-33.518924746634,44.,1.10218211923262E-15));
#37158=CARTESIAN_POINT('Ctrl Pts',(-33.3522580799673,44.,-5.19615242270663));
#37159=CARTESIAN_POINT('Ctrl Pts',(-33.1855914133007,39.5,-7.79422863405995));
#37160=CARTESIAN_POINT('Ctrl Pts',(-33.018924746634,35.,-10.3923048454133));
#37161=CARTESIAN_POINT('Ctrl Pts',(-32.8522580799673,30.5,-7.79422863405995));
#37162=CARTESIAN_POINT('Ctrl Pts',(-32.6855914133007,26.,-5.19615242270663));
#37163=CARTESIAN_POINT('Ctrl Pts',(-32.518924746634,26.,0.));
#37164=CARTESIAN_POINT('Ctrl Pts',(-32.3522580799673,26.,5.19615242270663));
#37165=CARTESIAN_POINT('Ctrl Pts',(-32.1855914133007,30.5,7.79422863405995));
#37166=CARTESIAN_POINT('Ctrl Pts',(-32.018924746634,35.,10.3923048454133));
#37167=CARTESIAN_POINT('Ctrl Pts',(-31.8522580799673,39.5,7.79422863405995));
#37168=CARTESIAN_POINT('Ctrl Pts',(-31.6855914133007,44.,5.19615242270663));
#37169=CARTESIAN_POINT('Ctrl Pts',(-31.518924746634,44.,1.10218211923262E-15));
#37170=CARTESIAN_POINT('Ctrl Pts',(-31.3522580799673,44.,-5.19615242270663));
#37171=CARTESIAN_POINT('Ctrl Pts',(-31.1855914133007,39.5,-7.79422863405995));
#37172=CARTESIAN_POINT('Ctrl Pts',(-31.018924746634,35.,-10.3923048454133));
#37173=CARTESIAN_POINT('Ctrl Pts',(-30.8522580799673,30.5,-7.79422863405995));
#37174=CARTESIAN_POINT('Ctrl Pts',(-30.6855914133007,26.,-5.19615242270663));
#37175=CARTESIAN_POINT('Ctrl Pts',(-30.518924746634,26.,0.));
#37176=CARTESIAN_POINT('Ctrl Pts',(-30.3522580799673,26.,5.19615242270663));
#37177=CARTESIAN_POINT('Ctrl Pts',(-30.1855914133007,30.5,7.79422863405995));
#37178=CARTESIAN_POINT('Ctrl Pts',(-30.018924746634,35.,10.3923048454133));
#37179=CARTESIAN_POINT('Ctrl Pts',(-29.8522580799673,39.5,7.79422863405995));
#37180=CARTESIAN_POINT('Ctrl Pts',(-29.6855914133007,44.,5.19615242270663));
#37181=CARTESIAN_POINT('Ctrl Pts',(-29.518924746634,44.,1.10218211923262E-15));
#37182=CARTESIAN_POINT('Ctrl Pts',(-29.3522580799673,44.,-5.19615242270663));
#37183=CARTESIAN_POINT('Ctrl Pts',(-29.1855914133007,39.5,-7.79422863405995));
#37184=CARTESIAN_POINT('Ctrl Pts',(-29.018924746634,35.,-10.3923048454133));
#37185=CARTESIAN_POINT('Ctrl Pts',(-28.8522580799673,30.5,-7.79422863405995));
#37186=CARTESIAN_POINT('Ctrl Pts',(-28.6855914133007,26.,-5.19615242270663));
#37187=CARTESIAN_POINT('Ctrl Pts',(-28.518924746634,26.,0.));
#37188=CARTESIAN_POINT('Ctrl Pts',(-28.3522580799673,26.,5.19615242270663));
#37189=CARTESIAN_POINT('Ctrl Pts',(-28.1855914133007,30.5,7.79422863405995));
#37190=CARTESIAN_POINT('Ctrl Pts',(-28.018924746634,35.,10.3923048454133));
#37191=CARTESIAN_POINT('Ctrl Pts',(-27.8522580799673,39.5,7.79422863405995));
#37192=CARTESIAN_POINT('Ctrl Pts',(-27.6855914133007,44.,5.19615242270663));
#37193=CARTESIAN_POINT('Ctrl Pts',(-27.518924746634,44.,1.10218211923262E-15));
#37194=CARTESIAN_POINT('Ctrl Pts',(-27.3522580799673,44.,-5.19615242270663));
#37195=CARTESIAN_POINT('Ctrl Pts',(-27.1855914133007,39.5,-7.79422863405995));
#37196=CARTESIAN_POINT('Ctrl Pts',(-27.018924746634,35.,-10.3923048454133));
#37197=CARTESIAN_POINT('Ctrl Pts',(-26.8522580799673,30.5,-7.79422863405995));
#37198=CARTESIAN_POINT('Ctrl Pts',(-26.6855914133007,26.,-5.19615242270663));
#37199=CARTESIAN_POINT('Ctrl Pts',(-26.518924746634,26.,0.));
#37200=CARTESIAN_POINT('Ctrl Pts',(-26.3522580799673,26.,5.19615242270663));
#37201=CARTESIAN_POINT('Ctrl Pts',(-26.1855914133007,30.5,7.79422863405995));
#37202=CARTESIAN_POINT('Ctrl Pts',(-26.018924746634,35.,10.3923048454133));
#37203=CARTESIAN_POINT('Ctrl Pts',(-25.8522580799673,39.5,7.79422863405995));
#37204=CARTESIAN_POINT('Ctrl Pts',(-25.6855914133007,44.,5.19615242270663));
#37205=CARTESIAN_POINT('Ctrl Pts',(-25.518924746634,44.,1.10218211923262E-15));
#37206=CARTESIAN_POINT('Ctrl Pts',(-25.3522580799673,44.,-5.19615242270663));
#37207=CARTESIAN_POINT('Ctrl Pts',(-25.1855914133007,39.5,-7.79422863405995));
#37208=CARTESIAN_POINT('Ctrl Pts',(-25.018924746634,35.,-10.3923048454133));
#37209=CARTESIAN_POINT('Ctrl Pts',(-24.8522580799673,30.5,-7.79422863405995));
#37210=CARTESIAN_POINT('Ctrl Pts',(-24.6855914133007,26.,-5.19615242270663));
#37211=CARTESIAN_POINT('Ctrl Pts',(-24.518924746634,26.,0.));
#37212=CARTESIAN_POINT('Ctrl Pts',(-24.3522580799673,26.,5.19615242270663));
#37213=CARTESIAN_POINT('Ctrl Pts',(-24.1855914133007,30.5,7.79422863405995));
#37214=CARTESIAN_POINT('Ctrl Pts',(-24.018924746634,35.,10.3923048454133));
#37215=CARTESIAN_POINT('Ctrl Pts',(-23.8522580799673,39.5,7.79422863405995));
#37216=CARTESIAN_POINT('Ctrl Pts',(-23.6855914133007,44.,5.19615242270663));
#37217=CARTESIAN_POINT('Ctrl Pts',(-23.518924746634,44.,1.10218211923262E-15));
#37218=CARTESIAN_POINT('Ctrl Pts',(-23.3522580799673,44.,-5.19615242270663));
#37219=CARTESIAN_POINT('Ctrl Pts',(-23.1855914133007,39.5,-7.79422863405995));
#37220=CARTESIAN_POINT('Ctrl Pts',(-23.018924746634,35.,-10.3923048454133));
#37221=CARTESIAN_POINT('Ctrl Pts',(-22.8522580799673,30.5,-7.79422863405995));
#37222=CARTESIAN_POINT('Ctrl Pts',(-22.6855914133007,26.,-5.19615242270663));
#37223=CARTESIAN_POINT('Ctrl Pts',(-22.518924746634,26.,0.));
#37224=CARTESIAN_POINT('Ctrl Pts',(-22.3522580799673,26.,5.19615242270663));
#37225=CARTESIAN_POINT('Ctrl Pts',(-22.1855914133007,30.5,7.79422863405995));
#37226=CARTESIAN_POINT('Ctrl Pts',(-22.018924746634,35.,10.3923048454133));
#37227=CARTESIAN_POINT('Ctrl Pts',(-21.8522580799673,39.5,7.79422863405995));
#37228=CARTESIAN_POINT('Ctrl Pts',(-21.6855914133007,44.,5.19615242270663));
#37229=CARTESIAN_POINT('Ctrl Pts',(-21.518924746634,44.,1.10218211923262E-15));
#37230=CARTESIAN_POINT('Ctrl Pts',(-21.3522580799673,44.,-5.19615242270663));
#37231=CARTESIAN_POINT('Ctrl Pts',(-21.1855914133006,39.5,-7.79422863405995));
#37232=CARTESIAN_POINT('Ctrl Pts',(-21.018924746634,35.,-10.3923048454133));
#37233=CARTESIAN_POINT('Ctrl Pts',(-20.8522580799673,30.5,-7.79422863405995));
#37234=CARTESIAN_POINT('Ctrl Pts',(-20.6855914133007,26.,-5.19615242270663));
#37235=CARTESIAN_POINT('Ctrl Pts',(-20.518924746634,26.,0.));
#37236=CARTESIAN_POINT('Ctrl Pts',(-20.3522580799673,26.,5.19615242270663));
#37237=CARTESIAN_POINT('Ctrl Pts',(-20.1855914133006,30.5,7.79422863405995));
#37238=CARTESIAN_POINT('Ctrl Pts',(-20.018924746634,35.,10.3923048454133));
#37239=CARTESIAN_POINT('Ctrl Pts',(-19.8522580799674,39.5,7.79422863405995));
#37240=CARTESIAN_POINT('Ctrl Pts',(-19.6855914133006,44.,5.19615242270663));
#37241=CARTESIAN_POINT('Ctrl Pts',(-19.518924746634,44.,1.10218211923262E-15));
#37242=CARTESIAN_POINT('Ctrl Pts',(-19.3522580799673,44.,-5.19615242270663));
#37243=CARTESIAN_POINT('Ctrl Pts',(-19.1855914133007,39.5,-7.79422863405995));
#37244=CARTESIAN_POINT('Ctrl Pts',(-19.018924746634,35.,-10.3923048454133));
#37245=CARTESIAN_POINT('Ctrl Pts',(-18.8522580799674,30.5,-7.79422863405995));
#37246=CARTESIAN_POINT('Ctrl Pts',(-18.6855914133007,26.,-5.19615242270663));
#37247=CARTESIAN_POINT('Ctrl Pts',(-18.518924746634,26.,0.));
#37248=CARTESIAN_POINT('Ctrl Pts',(-38.518924746634,27.6,0.));
#37249=CARTESIAN_POINT('Ctrl Pts',(-38.3522580799673,27.6,4.27239199200323));
#37250=CARTESIAN_POINT('Ctrl Pts',(-38.1855914133007,31.3,6.40858798800485));
#37251=CARTESIAN_POINT('Ctrl Pts',(-38.018924746634,35.,8.54478398400645));
#37252=CARTESIAN_POINT('Ctrl Pts',(-37.8522580799673,38.7,6.40858798800485));
#37253=CARTESIAN_POINT('Ctrl Pts',(-37.6855914133007,42.4,4.27239199200323));
#37254=CARTESIAN_POINT('Ctrl Pts',(-37.518924746634,42.4,9.06238631369041E-16));
#37255=CARTESIAN_POINT('Ctrl Pts',(-37.3522580799673,42.4,-4.27239199200323));
#37256=CARTESIAN_POINT('Ctrl Pts',(-37.1855914133007,38.7,-6.40858798800485));
#37257=CARTESIAN_POINT('Ctrl Pts',(-37.018924746634,35.,-8.54478398400645));
#37258=CARTESIAN_POINT('Ctrl Pts',(-36.8522580799673,31.3,-6.40858798800485));
#37259=CARTESIAN_POINT('Ctrl Pts',(-36.6855914133007,27.6,-4.27239199200323));
#37260=CARTESIAN_POINT('Ctrl Pts',(-36.518924746634,27.6,0.));
#37261=CARTESIAN_POINT('Ctrl Pts',(-36.3522580799673,27.6,4.27239199200323));
#37262=CARTESIAN_POINT('Ctrl Pts',(-36.1855914133007,31.3,6.40858798800485));
#37263=CARTESIAN_POINT('Ctrl Pts',(-36.018924746634,35.,8.54478398400645));
#37264=CARTESIAN_POINT('Ctrl Pts',(-35.8522580799673,38.7,6.40858798800485));
#37265=CARTESIAN_POINT('Ctrl Pts',(-35.6855914133007,42.4,4.27239199200323));
#37266=CARTESIAN_POINT('Ctrl Pts',(-35.518924746634,42.4,9.06238631369041E-16));
#37267=CARTESIAN_POINT('Ctrl Pts',(-35.3522580799673,42.4,-4.27239199200323));
#37268=CARTESIAN_POINT('Ctrl Pts',(-35.1855914133007,38.7,-6.40858798800485));
#37269=CARTESIAN_POINT('Ctrl Pts',(-35.018924746634,35.,-8.54478398400645));
#37270=CARTESIAN_POINT('Ctrl Pts',(-34.8522580799673,31.3,-6.40858798800485));
#37271=CARTESIAN_POINT('Ctrl Pts',(-34.6855914133007,27.6,-4.27239199200323));
#37272=CARTESIAN_POINT('Ctrl Pts',(-34.518924746634,27.6,0.));
#37273=CARTESIAN_POINT('Ctrl Pts',(-34.3522580799673,27.6,4.27239199200323));
#37274=CARTESIAN_POINT('Ctrl Pts',(-34.1855914133007,31.3,6.40858798800485));
#37275=CARTESIAN_POINT('Ctrl Pts',(-34.018924746634,35.,8.54478398400645));
#37276=CARTESIAN_POINT('Ctrl Pts',(-33.8522580799673,38.7,6.40858798800485));
#37277=CARTESIAN_POINT('Ctrl Pts',(-33.6855914133007,42.4,4.27239199200323));
#37278=CARTESIAN_POINT('Ctrl Pts',(-33.518924746634,42.4,9.06238631369041E-16));
#37279=CARTESIAN_POINT('Ctrl Pts',(-33.3522580799673,42.4,-4.27239199200323));
#37280=CARTESIAN_POINT('Ctrl Pts',(-33.1855914133007,38.7,-6.40858798800485));
#37281=CARTESIAN_POINT('Ctrl Pts',(-33.018924746634,35.,-8.54478398400645));
#37282=CARTESIAN_POINT('Ctrl Pts',(-32.8522580799673,31.3,-6.40858798800485));
#37283=CARTESIAN_POINT('Ctrl Pts',(-32.6855914133007,27.6,-4.27239199200323));
#37284=CARTESIAN_POINT('Ctrl Pts',(-32.518924746634,27.6,0.));
#37285=CARTESIAN_POINT('Ctrl Pts',(-32.3522580799673,27.6,4.27239199200323));
#37286=CARTESIAN_POINT('Ctrl Pts',(-32.1855914133007,31.3,6.40858798800485));
#37287=CARTESIAN_POINT('Ctrl Pts',(-32.018924746634,35.,8.54478398400645));
#37288=CARTESIAN_POINT('Ctrl Pts',(-31.8522580799674,38.7,6.40858798800485));
#37289=CARTESIAN_POINT('Ctrl Pts',(-31.6855914133007,42.4,4.27239199200323));
#37290=CARTESIAN_POINT('Ctrl Pts',(-31.518924746634,42.4,9.06238631369041E-16));
#37291=CARTESIAN_POINT('Ctrl Pts',(-31.3522580799673,42.4,-4.27239199200323));
#37292=CARTESIAN_POINT('Ctrl Pts',(-31.1855914133007,38.7,-6.40858798800485));
#37293=CARTESIAN_POINT('Ctrl Pts',(-31.018924746634,35.,-8.54478398400645));
#37294=CARTESIAN_POINT('Ctrl Pts',(-30.8522580799673,31.3,-6.40858798800485));
#37295=CARTESIAN_POINT('Ctrl Pts',(-30.6855914133007,27.6,-4.27239199200323));
#37296=CARTESIAN_POINT('Ctrl Pts',(-30.518924746634,27.6,0.));
#37297=CARTESIAN_POINT('Ctrl Pts',(-30.3522580799673,27.6,4.27239199200323));
#37298=CARTESIAN_POINT('Ctrl Pts',(-30.1855914133007,31.3,6.40858798800485));
#37299=CARTESIAN_POINT('Ctrl Pts',(-30.018924746634,35.,8.54478398400645));
#37300=CARTESIAN_POINT('Ctrl Pts',(-29.8522580799673,38.7,6.40858798800485));
#37301=CARTESIAN_POINT('Ctrl Pts',(-29.6855914133007,42.4,4.27239199200323));
#37302=CARTESIAN_POINT('Ctrl Pts',(-29.518924746634,42.4,9.06238631369041E-16));
#37303=CARTESIAN_POINT('Ctrl Pts',(-29.3522580799673,42.4,-4.27239199200323));
#37304=CARTESIAN_POINT('Ctrl Pts',(-29.1855914133007,38.7,-6.40858798800485));
#37305=CARTESIAN_POINT('Ctrl Pts',(-29.018924746634,35.,-8.54478398400645));
#37306=CARTESIAN_POINT('Ctrl Pts',(-28.8522580799673,31.3,-6.40858798800485));
#37307=CARTESIAN_POINT('Ctrl Pts',(-28.6855914133007,27.6,-4.27239199200323));
#37308=CARTESIAN_POINT('Ctrl Pts',(-28.518924746634,27.6,0.));
#37309=CARTESIAN_POINT('Ctrl Pts',(-28.3522580799673,27.6,4.27239199200323));
#37310=CARTESIAN_POINT('Ctrl Pts',(-28.1855914133007,31.3,6.40858798800485));
#37311=CARTESIAN_POINT('Ctrl Pts',(-28.018924746634,35.,8.54478398400645));
#37312=CARTESIAN_POINT('Ctrl Pts',(-27.8522580799673,38.7,6.40858798800485));
#37313=CARTESIAN_POINT('Ctrl Pts',(-27.6855914133007,42.4,4.27239199200323));
#37314=CARTESIAN_POINT('Ctrl Pts',(-27.518924746634,42.4,9.06238631369041E-16));
#37315=CARTESIAN_POINT('Ctrl Pts',(-27.3522580799673,42.4,-4.27239199200323));
#37316=CARTESIAN_POINT('Ctrl Pts',(-27.1855914133007,38.7,-6.40858798800485));
#37317=CARTESIAN_POINT('Ctrl Pts',(-27.018924746634,35.,-8.54478398400645));
#37318=CARTESIAN_POINT('Ctrl Pts',(-26.8522580799673,31.3,-6.40858798800485));
#37319=CARTESIAN_POINT('Ctrl Pts',(-26.6855914133007,27.6,-4.27239199200323));
#37320=CARTESIAN_POINT('Ctrl Pts',(-26.518924746634,27.6,0.));
#37321=CARTESIAN_POINT('Ctrl Pts',(-26.3522580799673,27.6,4.27239199200323));
#37322=CARTESIAN_POINT('Ctrl Pts',(-26.1855914133007,31.3,6.40858798800485));
#37323=CARTESIAN_POINT('Ctrl Pts',(-26.018924746634,35.,8.54478398400645));
#37324=CARTESIAN_POINT('Ctrl Pts',(-25.8522580799673,38.7,6.40858798800485));
#37325=CARTESIAN_POINT('Ctrl Pts',(-25.6855914133007,42.4,4.27239199200323));
#37326=CARTESIAN_POINT('Ctrl Pts',(-25.518924746634,42.4,9.06238631369041E-16));
#37327=CARTESIAN_POINT('Ctrl Pts',(-25.3522580799673,42.4,-4.27239199200323));
#37328=CARTESIAN_POINT('Ctrl Pts',(-25.1855914133007,38.7,-6.40858798800485));
#37329=CARTESIAN_POINT('Ctrl Pts',(-25.018924746634,35.,-8.54478398400645));
#37330=CARTESIAN_POINT('Ctrl Pts',(-24.8522580799673,31.3,-6.40858798800485));
#37331=CARTESIAN_POINT('Ctrl Pts',(-24.6855914133007,27.6,-4.27239199200323));
#37332=CARTESIAN_POINT('Ctrl Pts',(-24.518924746634,27.6,0.));
#37333=CARTESIAN_POINT('Ctrl Pts',(-24.3522580799673,27.6,4.27239199200323));
#37334=CARTESIAN_POINT('Ctrl Pts',(-24.1855914133007,31.3,6.40858798800485));
#37335=CARTESIAN_POINT('Ctrl Pts',(-24.018924746634,35.,8.54478398400645));
#37336=CARTESIAN_POINT('Ctrl Pts',(-23.8522580799674,38.7,6.40858798800485));
#37337=CARTESIAN_POINT('Ctrl Pts',(-23.6855914133007,42.4,4.27239199200323));
#37338=CARTESIAN_POINT('Ctrl Pts',(-23.518924746634,42.4,9.06238631369041E-16));
#37339=CARTESIAN_POINT('Ctrl Pts',(-23.3522580799673,42.4,-4.27239199200323));
#37340=CARTESIAN_POINT('Ctrl Pts',(-23.1855914133007,38.7,-6.40858798800485));
#37341=CARTESIAN_POINT('Ctrl Pts',(-23.018924746634,35.,-8.54478398400645));
#37342=CARTESIAN_POINT('Ctrl Pts',(-22.8522580799673,31.3,-6.40858798800485));
#37343=CARTESIAN_POINT('Ctrl Pts',(-22.6855914133007,27.6,-4.27239199200323));
#37344=CARTESIAN_POINT('Ctrl Pts',(-22.518924746634,27.6,0.));
#37345=CARTESIAN_POINT('Ctrl Pts',(-22.3522580799673,27.6,4.27239199200323));
#37346=CARTESIAN_POINT('Ctrl Pts',(-22.1855914133007,31.3,6.40858798800485));
#37347=CARTESIAN_POINT('Ctrl Pts',(-22.018924746634,35.,8.54478398400645));
#37348=CARTESIAN_POINT('Ctrl Pts',(-21.8522580799673,38.7,6.40858798800485));
#37349=CARTESIAN_POINT('Ctrl Pts',(-21.6855914133007,42.4,4.27239199200323));
#37350=CARTESIAN_POINT('Ctrl Pts',(-21.518924746634,42.4,9.06238631369041E-16));
#37351=CARTESIAN_POINT('Ctrl Pts',(-21.3522580799673,42.4,-4.27239199200323));
#37352=CARTESIAN_POINT('Ctrl Pts',(-21.1855914133007,38.7,-6.40858798800485));
#37353=CARTESIAN_POINT('Ctrl Pts',(-21.018924746634,35.,-8.54478398400645));
#37354=CARTESIAN_POINT('Ctrl Pts',(-20.8522580799674,31.3,-6.40858798800485));
#37355=CARTESIAN_POINT('Ctrl Pts',(-20.6855914133006,27.6,-4.27239199200323));
#37356=CARTESIAN_POINT('Ctrl Pts',(-20.518924746634,27.6,0.));
#37357=CARTESIAN_POINT('Ctrl Pts',(-20.3522580799673,27.6,4.27239199200323));
#37358=CARTESIAN_POINT('Ctrl Pts',(-20.1855914133007,31.3,6.40858798800485));
#37359=CARTESIAN_POINT('Ctrl Pts',(-20.018924746634,35.,8.54478398400645));
#37360=CARTESIAN_POINT('Ctrl Pts',(-19.8522580799673,38.7,6.40858798800485));
#37361=CARTESIAN_POINT('Ctrl Pts',(-19.6855914133007,42.4,4.27239199200323));
#37362=CARTESIAN_POINT('Ctrl Pts',(-19.518924746634,42.4,9.06238631369041E-16));
#37363=CARTESIAN_POINT('Ctrl Pts',(-19.3522580799673,42.4,-4.27239199200323));
#37364=CARTESIAN_POINT('Ctrl Pts',(-19.1855914133007,38.7,-6.40858798800485));
#37365=CARTESIAN_POINT('Ctrl Pts',(-19.018924746634,35.,-8.54478398400645));
#37366=CARTESIAN_POINT('Ctrl Pts',(-18.8522580799673,31.3,-6.40858798800485));
#37367=CARTESIAN_POINT('Ctrl Pts',(-18.6855914133007,27.6,-4.27239199200323));
#37368=CARTESIAN_POINT('Ctrl Pts',(-18.518924746634,27.6,0.));
#37369=CARTESIAN_POINT('Ctrl Pts',(-36.918924746634,27.6,0.));
#37370=CARTESIAN_POINT('Ctrl Pts',(-36.7522580799673,27.6,4.27239199200323));
#37371=CARTESIAN_POINT('Ctrl Pts',(-36.5855914133007,31.3,6.40858798800485));
#37372=CARTESIAN_POINT('Ctrl Pts',(-36.418924746634,35.,8.54478398400645));
#37373=CARTESIAN_POINT('Ctrl Pts',(-36.2522580799673,38.7,6.40858798800485));
#37374=CARTESIAN_POINT('Ctrl Pts',(-36.0855914133007,42.4,4.27239199200323));
#37375=CARTESIAN_POINT('Ctrl Pts',(-35.918924746634,42.4,9.06238631369041E-16));
#37376=CARTESIAN_POINT('Ctrl Pts',(-35.7522580799673,42.4,-4.27239199200323));
#37377=CARTESIAN_POINT('Ctrl Pts',(-35.5855914133007,38.7,-6.40858798800485));
#37378=CARTESIAN_POINT('Ctrl Pts',(-35.418924746634,35.,-8.54478398400645));
#37379=CARTESIAN_POINT('Ctrl Pts',(-35.2522580799673,31.3,-6.40858798800485));
#37380=CARTESIAN_POINT('Ctrl Pts',(-35.0855914133007,27.6,-4.27239199200323));
#37381=CARTESIAN_POINT('Ctrl Pts',(-34.918924746634,27.6,0.));
#37382=CARTESIAN_POINT('Ctrl Pts',(-34.7522580799673,27.6,4.27239199200323));
#37383=CARTESIAN_POINT('Ctrl Pts',(-34.5855914133007,31.3,6.40858798800485));
#37384=CARTESIAN_POINT('Ctrl Pts',(-34.418924746634,35.,8.54478398400645));
#37385=CARTESIAN_POINT('Ctrl Pts',(-34.2522580799673,38.7,6.40858798800485));
#37386=CARTESIAN_POINT('Ctrl Pts',(-34.0855914133007,42.4,4.27239199200323));
#37387=CARTESIAN_POINT('Ctrl Pts',(-33.918924746634,42.4,9.06238631369041E-16));
#37388=CARTESIAN_POINT('Ctrl Pts',(-33.7522580799673,42.4,-4.27239199200323));
#37389=CARTESIAN_POINT('Ctrl Pts',(-33.5855914133007,38.7,-6.40858798800485));
#37390=CARTESIAN_POINT('Ctrl Pts',(-33.418924746634,35.,-8.54478398400645));
#37391=CARTESIAN_POINT('Ctrl Pts',(-33.2522580799673,31.3,-6.40858798800485));
#37392=CARTESIAN_POINT('Ctrl Pts',(-33.0855914133007,27.6,-4.27239199200323));
#37393=CARTESIAN_POINT('Ctrl Pts',(-32.918924746634,27.6,0.));
#37394=CARTESIAN_POINT('Ctrl Pts',(-32.7522580799673,27.6,4.27239199200323));
#37395=CARTESIAN_POINT('Ctrl Pts',(-32.5855914133007,31.3,6.40858798800485));
#37396=CARTESIAN_POINT('Ctrl Pts',(-32.418924746634,35.,8.54478398400645));
#37397=CARTESIAN_POINT('Ctrl Pts',(-32.2522580799673,38.7,6.40858798800485));
#37398=CARTESIAN_POINT('Ctrl Pts',(-32.0855914133007,42.4,4.27239199200323));
#37399=CARTESIAN_POINT('Ctrl Pts',(-31.918924746634,42.4,9.06238631369041E-16));
#37400=CARTESIAN_POINT('Ctrl Pts',(-31.7522580799673,42.4,-4.27239199200323));
#37401=CARTESIAN_POINT('Ctrl Pts',(-31.5855914133007,38.7,-6.40858798800485));
#37402=CARTESIAN_POINT('Ctrl Pts',(-31.418924746634,35.,-8.54478398400645));
#37403=CARTESIAN_POINT('Ctrl Pts',(-31.2522580799673,31.3,-6.40858798800485));
#37404=CARTESIAN_POINT('Ctrl Pts',(-31.0855914133007,27.6,-4.27239199200323));
#37405=CARTESIAN_POINT('Ctrl Pts',(-30.918924746634,27.6,0.));
#37406=CARTESIAN_POINT('Ctrl Pts',(-30.7522580799673,27.6,4.27239199200323));
#37407=CARTESIAN_POINT('Ctrl Pts',(-30.5855914133007,31.3,6.40858798800485));
#37408=CARTESIAN_POINT('Ctrl Pts',(-30.418924746634,35.,8.54478398400645));
#37409=CARTESIAN_POINT('Ctrl Pts',(-30.2522580799673,38.7,6.40858798800485));
#37410=CARTESIAN_POINT('Ctrl Pts',(-30.0855914133007,42.4,4.27239199200323));
#37411=CARTESIAN_POINT('Ctrl Pts',(-29.918924746634,42.4,9.06238631369041E-16));
#37412=CARTESIAN_POINT('Ctrl Pts',(-29.7522580799673,42.4,-4.27239199200323));
#37413=CARTESIAN_POINT('Ctrl Pts',(-29.5855914133007,38.7,-6.40858798800485));
#37414=CARTESIAN_POINT('Ctrl Pts',(-29.418924746634,35.,-8.54478398400645));
#37415=CARTESIAN_POINT('Ctrl Pts',(-29.2522580799673,31.3,-6.40858798800485));
#37416=CARTESIAN_POINT('Ctrl Pts',(-29.0855914133007,27.6,-4.27239199200323));
#37417=CARTESIAN_POINT('Ctrl Pts',(-28.918924746634,27.6,0.));
#37418=CARTESIAN_POINT('Ctrl Pts',(-28.7522580799673,27.6,4.27239199200323));
#37419=CARTESIAN_POINT('Ctrl Pts',(-28.5855914133007,31.3,6.40858798800485));
#37420=CARTESIAN_POINT('Ctrl Pts',(-28.418924746634,35.,8.54478398400645));
#37421=CARTESIAN_POINT('Ctrl Pts',(-28.2522580799673,38.7,6.40858798800485));
#37422=CARTESIAN_POINT('Ctrl Pts',(-28.0855914133007,42.4,4.27239199200323));
#37423=CARTESIAN_POINT('Ctrl Pts',(-27.918924746634,42.4,9.06238631369041E-16));
#37424=CARTESIAN_POINT('Ctrl Pts',(-27.7522580799673,42.4,-4.27239199200323));
#37425=CARTESIAN_POINT('Ctrl Pts',(-27.5855914133007,38.7,-6.40858798800485));
#37426=CARTESIAN_POINT('Ctrl Pts',(-27.418924746634,35.,-8.54478398400645));
#37427=CARTESIAN_POINT('Ctrl Pts',(-27.2522580799673,31.3,-6.40858798800485));
#37428=CARTESIAN_POINT('Ctrl Pts',(-27.0855914133007,27.6,-4.27239199200323));
#37429=CARTESIAN_POINT('Ctrl Pts',(-26.918924746634,27.6,0.));
#37430=CARTESIAN_POINT('Ctrl Pts',(-26.7522580799673,27.6,4.27239199200323));
#37431=CARTESIAN_POINT('Ctrl Pts',(-26.5855914133007,31.3,6.40858798800485));
#37432=CARTESIAN_POINT('Ctrl Pts',(-26.418924746634,35.,8.54478398400645));
#37433=CARTESIAN_POINT('Ctrl Pts',(-26.2522580799673,38.7,6.40858798800485));
#37434=CARTESIAN_POINT('Ctrl Pts',(-26.0855914133007,42.4,4.27239199200323));
#37435=CARTESIAN_POINT('Ctrl Pts',(-25.918924746634,42.4,9.06238631369041E-16));
#37436=CARTESIAN_POINT('Ctrl Pts',(-25.7522580799673,42.4,-4.27239199200323));
#37437=CARTESIAN_POINT('Ctrl Pts',(-25.5855914133007,38.7,-6.40858798800485));
#37438=CARTESIAN_POINT('Ctrl Pts',(-25.418924746634,35.,-8.54478398400645));
#37439=CARTESIAN_POINT('Ctrl Pts',(-25.2522580799673,31.3,-6.40858798800485));
#37440=CARTESIAN_POINT('Ctrl Pts',(-25.0855914133007,27.6,-4.27239199200323));
#37441=CARTESIAN_POINT('Ctrl Pts',(-24.918924746634,27.6,0.));
#37442=CARTESIAN_POINT('Ctrl Pts',(-24.7522580799673,27.6,4.27239199200323));
#37443=CARTESIAN_POINT('Ctrl Pts',(-24.5855914133007,31.3,6.40858798800485));
#37444=CARTESIAN_POINT('Ctrl Pts',(-24.418924746634,35.,8.54478398400645));
#37445=CARTESIAN_POINT('Ctrl Pts',(-24.2522580799673,38.7,6.40858798800485));
#37446=CARTESIAN_POINT('Ctrl Pts',(-24.0855914133007,42.4,4.27239199200323));
#37447=CARTESIAN_POINT('Ctrl Pts',(-23.918924746634,42.4,9.06238631369041E-16));
#37448=CARTESIAN_POINT('Ctrl Pts',(-23.7522580799673,42.4,-4.27239199200323));
#37449=CARTESIAN_POINT('Ctrl Pts',(-23.5855914133007,38.7,-6.40858798800485));
#37450=CARTESIAN_POINT('Ctrl Pts',(-23.418924746634,35.,-8.54478398400645));
#37451=CARTESIAN_POINT('Ctrl Pts',(-23.2522580799673,31.3,-6.40858798800485));
#37452=CARTESIAN_POINT('Ctrl Pts',(-23.0855914133007,27.6,-4.27239199200323));
#37453=CARTESIAN_POINT('Ctrl Pts',(-22.918924746634,27.6,0.));
#37454=CARTESIAN_POINT('Ctrl Pts',(-22.7522580799673,27.6,4.27239199200323));
#37455=CARTESIAN_POINT('Ctrl Pts',(-22.5855914133007,31.3,6.40858798800485));
#37456=CARTESIAN_POINT('Ctrl Pts',(-22.418924746634,35.,8.54478398400645));
#37457=CARTESIAN_POINT('Ctrl Pts',(-22.2522580799673,38.7,6.40858798800485));
#37458=CARTESIAN_POINT('Ctrl Pts',(-22.0855914133007,42.4,4.27239199200323));
#37459=CARTESIAN_POINT('Ctrl Pts',(-21.918924746634,42.4,9.06238631369041E-16));
#37460=CARTESIAN_POINT('Ctrl Pts',(-21.7522580799673,42.4,-4.27239199200323));
#37461=CARTESIAN_POINT('Ctrl Pts',(-21.5855914133007,38.7,-6.40858798800485));
#37462=CARTESIAN_POINT('Ctrl Pts',(-21.418924746634,35.,-8.54478398400645));
#37463=CARTESIAN_POINT('Ctrl Pts',(-21.2522580799673,31.3,-6.40858798800485));
#37464=CARTESIAN_POINT('Ctrl Pts',(-21.0855914133007,27.6,-4.27239199200323));
#37465=CARTESIAN_POINT('Ctrl Pts',(-20.918924746634,27.6,0.));
#37466=CARTESIAN_POINT('Ctrl Pts',(-20.7522580799673,27.6,4.27239199200323));
#37467=CARTESIAN_POINT('Ctrl Pts',(-20.5855914133007,31.3,6.40858798800485));
#37468=CARTESIAN_POINT('Ctrl Pts',(-20.418924746634,35.,8.54478398400645));
#37469=CARTESIAN_POINT('Ctrl Pts',(-20.2522580799673,38.7,6.40858798800485));
#37470=CARTESIAN_POINT('Ctrl Pts',(-20.0855914133007,42.4,4.27239199200323));
#37471=CARTESIAN_POINT('Ctrl Pts',(-19.918924746634,42.4,9.06238631369041E-16));
#37472=CARTESIAN_POINT('Ctrl Pts',(-19.7522580799673,42.4,-4.27239199200323));
#37473=CARTESIAN_POINT('Ctrl Pts',(-19.5855914133007,38.7,-6.40858798800485));
#37474=CARTESIAN_POINT('Ctrl Pts',(-19.418924746634,35.,-8.54478398400645));
#37475=CARTESIAN_POINT('Ctrl Pts',(-19.2522580799673,31.3,-6.40858798800485));
#37476=CARTESIAN_POINT('Ctrl Pts',(-19.0855914133006,27.6,-4.27239199200323));
#37477=CARTESIAN_POINT('Ctrl Pts',(-18.918924746634,27.6,0.));
#37478=CARTESIAN_POINT('Ctrl Pts',(-18.7522580799673,27.6,4.27239199200323));
#37479=CARTESIAN_POINT('Ctrl Pts',(-18.5855914133007,31.3,6.40858798800485));
#37480=CARTESIAN_POINT('Ctrl Pts',(-18.418924746634,35.,8.54478398400645));
#37481=CARTESIAN_POINT('Ctrl Pts',(-18.2522580799673,38.7,6.40858798800485));
#37482=CARTESIAN_POINT('Ctrl Pts',(-18.0855914133007,42.4,4.27239199200323));
#37483=CARTESIAN_POINT('Ctrl Pts',(-17.918924746634,42.4,9.06238631369041E-16));
#37484=CARTESIAN_POINT('Ctrl Pts',(-17.7522580799673,42.4,-4.27239199200323));
#37485=CARTESIAN_POINT('Ctrl Pts',(-17.5855914133007,38.7,-6.40858798800485));
#37486=CARTESIAN_POINT('Ctrl Pts',(-17.418924746634,35.,-8.54478398400645));
#37487=CARTESIAN_POINT('Ctrl Pts',(-17.2522580799674,31.3,-6.40858798800485));
#37488=CARTESIAN_POINT('Ctrl Pts',(-17.0855914133007,27.6,-4.27239199200323));
#37489=CARTESIAN_POINT('Ctrl Pts',(-16.918924746634,27.6,0.));
#37490=CARTESIAN_POINT('Ctrl Pts',(-36.918924746634,26.,0.));
#37491=CARTESIAN_POINT('Ctrl Pts',(-36.7522580799673,26.,5.19615242270663));
#37492=CARTESIAN_POINT('Ctrl Pts',(-36.5855914133007,30.5,7.79422863405995));
#37493=CARTESIAN_POINT('Ctrl Pts',(-36.418924746634,35.,10.3923048454133));
#37494=CARTESIAN_POINT('Ctrl Pts',(-36.2522580799673,39.5,7.79422863405995));
#37495=CARTESIAN_POINT('Ctrl Pts',(-36.0855914133007,44.,5.19615242270663));
#37496=CARTESIAN_POINT('Ctrl Pts',(-35.918924746634,44.,1.10218211923262E-15));
#37497=CARTESIAN_POINT('Ctrl Pts',(-35.7522580799673,44.,-5.19615242270663));
#37498=CARTESIAN_POINT('Ctrl Pts',(-35.5855914133007,39.5,-7.79422863405995));
#37499=CARTESIAN_POINT('Ctrl Pts',(-35.418924746634,35.,-10.3923048454133));
#37500=CARTESIAN_POINT('Ctrl Pts',(-35.2522580799673,30.5,-7.79422863405995));
#37501=CARTESIAN_POINT('Ctrl Pts',(-35.0855914133007,26.,-5.19615242270663));
#37502=CARTESIAN_POINT('Ctrl Pts',(-34.918924746634,26.,0.));
#37503=CARTESIAN_POINT('Ctrl Pts',(-34.7522580799673,26.,5.19615242270663));
#37504=CARTESIAN_POINT('Ctrl Pts',(-34.5855914133007,30.5,7.79422863405995));
#37505=CARTESIAN_POINT('Ctrl Pts',(-34.418924746634,35.,10.3923048454133));
#37506=CARTESIAN_POINT('Ctrl Pts',(-34.2522580799673,39.5,7.79422863405995));
#37507=CARTESIAN_POINT('Ctrl Pts',(-34.0855914133007,44.,5.19615242270663));
#37508=CARTESIAN_POINT('Ctrl Pts',(-33.918924746634,44.,1.10218211923262E-15));
#37509=CARTESIAN_POINT('Ctrl Pts',(-33.7522580799673,44.,-5.19615242270663));
#37510=CARTESIAN_POINT('Ctrl Pts',(-33.5855914133007,39.5,-7.79422863405995));
#37511=CARTESIAN_POINT('Ctrl Pts',(-33.418924746634,35.,-10.3923048454133));
#37512=CARTESIAN_POINT('Ctrl Pts',(-33.2522580799673,30.5,-7.79422863405995));
#37513=CARTESIAN_POINT('Ctrl Pts',(-33.0855914133007,26.,-5.19615242270663));
#37514=CARTESIAN_POINT('Ctrl Pts',(-32.918924746634,26.,0.));
#37515=CARTESIAN_POINT('Ctrl Pts',(-32.7522580799673,26.,5.19615242270663));
#37516=CARTESIAN_POINT('Ctrl Pts',(-32.5855914133007,30.5,7.79422863405995));
#37517=CARTESIAN_POINT('Ctrl Pts',(-32.418924746634,35.,10.3923048454133));
#37518=CARTESIAN_POINT('Ctrl Pts',(-32.2522580799673,39.5,7.79422863405995));
#37519=CARTESIAN_POINT('Ctrl Pts',(-32.0855914133007,44.,5.19615242270663));
#37520=CARTESIAN_POINT('Ctrl Pts',(-31.918924746634,44.,1.10218211923262E-15));
#37521=CARTESIAN_POINT('Ctrl Pts',(-31.7522580799673,44.,-5.19615242270663));
#37522=CARTESIAN_POINT('Ctrl Pts',(-31.5855914133007,39.5,-7.79422863405995));
#37523=CARTESIAN_POINT('Ctrl Pts',(-31.418924746634,35.,-10.3923048454133));
#37524=CARTESIAN_POINT('Ctrl Pts',(-31.2522580799673,30.5,-7.79422863405995));
#37525=CARTESIAN_POINT('Ctrl Pts',(-31.0855914133007,26.,-5.19615242270663));
#37526=CARTESIAN_POINT('Ctrl Pts',(-30.918924746634,26.,0.));
#37527=CARTESIAN_POINT('Ctrl Pts',(-30.7522580799673,26.,5.19615242270663));
#37528=CARTESIAN_POINT('Ctrl Pts',(-30.5855914133007,30.5,7.79422863405995));
#37529=CARTESIAN_POINT('Ctrl Pts',(-30.418924746634,35.,10.3923048454133));
#37530=CARTESIAN_POINT('Ctrl Pts',(-30.2522580799673,39.5,7.79422863405995));
#37531=CARTESIAN_POINT('Ctrl Pts',(-30.0855914133007,44.,5.19615242270663));
#37532=CARTESIAN_POINT('Ctrl Pts',(-29.918924746634,44.,1.10218211923262E-15));
#37533=CARTESIAN_POINT('Ctrl Pts',(-29.7522580799673,44.,-5.19615242270663));
#37534=CARTESIAN_POINT('Ctrl Pts',(-29.5855914133007,39.5,-7.79422863405995));
#37535=CARTESIAN_POINT('Ctrl Pts',(-29.418924746634,35.,-10.3923048454133));
#37536=CARTESIAN_POINT('Ctrl Pts',(-29.2522580799673,30.5,-7.79422863405995));
#37537=CARTESIAN_POINT('Ctrl Pts',(-29.0855914133007,26.,-5.19615242270663));
#37538=CARTESIAN_POINT('Ctrl Pts',(-28.918924746634,26.,0.));
#37539=CARTESIAN_POINT('Ctrl Pts',(-28.7522580799673,26.,5.19615242270663));
#37540=CARTESIAN_POINT('Ctrl Pts',(-28.5855914133007,30.5,7.79422863405995));
#37541=CARTESIAN_POINT('Ctrl Pts',(-28.418924746634,35.,10.3923048454133));
#37542=CARTESIAN_POINT('Ctrl Pts',(-28.2522580799673,39.5,7.79422863405995));
#37543=CARTESIAN_POINT('Ctrl Pts',(-28.0855914133007,44.,5.19615242270663));
#37544=CARTESIAN_POINT('Ctrl Pts',(-27.918924746634,44.,1.10218211923262E-15));
#37545=CARTESIAN_POINT('Ctrl Pts',(-27.7522580799673,44.,-5.19615242270663));
#37546=CARTESIAN_POINT('Ctrl Pts',(-27.5855914133007,39.5,-7.79422863405995));
#37547=CARTESIAN_POINT('Ctrl Pts',(-27.418924746634,35.,-10.3923048454133));
#37548=CARTESIAN_POINT('Ctrl Pts',(-27.2522580799673,30.5,-7.79422863405995));
#37549=CARTESIAN_POINT('Ctrl Pts',(-27.0855914133007,26.,-5.19615242270663));
#37550=CARTESIAN_POINT('Ctrl Pts',(-26.918924746634,26.,0.));
#37551=CARTESIAN_POINT('Ctrl Pts',(-26.7522580799673,26.,5.19615242270663));
#37552=CARTESIAN_POINT('Ctrl Pts',(-26.5855914133007,30.5,7.79422863405995));
#37553=CARTESIAN_POINT('Ctrl Pts',(-26.418924746634,35.,10.3923048454133));
#37554=CARTESIAN_POINT('Ctrl Pts',(-26.2522580799673,39.5,7.79422863405995));
#37555=CARTESIAN_POINT('Ctrl Pts',(-26.0855914133007,44.,5.19615242270663));
#37556=CARTESIAN_POINT('Ctrl Pts',(-25.918924746634,44.,1.10218211923262E-15));
#37557=CARTESIAN_POINT('Ctrl Pts',(-25.7522580799673,44.,-5.19615242270663));
#37558=CARTESIAN_POINT('Ctrl Pts',(-25.5855914133007,39.5,-7.79422863405995));
#37559=CARTESIAN_POINT('Ctrl Pts',(-25.418924746634,35.,-10.3923048454133));
#37560=CARTESIAN_POINT('Ctrl Pts',(-25.2522580799673,30.5,-7.79422863405995));
#37561=CARTESIAN_POINT('Ctrl Pts',(-25.0855914133007,26.,-5.19615242270663));
#37562=CARTESIAN_POINT('Ctrl Pts',(-24.918924746634,26.,0.));
#37563=CARTESIAN_POINT('Ctrl Pts',(-24.7522580799673,26.,5.19615242270663));
#37564=CARTESIAN_POINT('Ctrl Pts',(-24.5855914133007,30.5,7.79422863405995));
#37565=CARTESIAN_POINT('Ctrl Pts',(-24.418924746634,35.,10.3923048454133));
#37566=CARTESIAN_POINT('Ctrl Pts',(-24.2522580799673,39.5,7.79422863405995));
#37567=CARTESIAN_POINT('Ctrl Pts',(-24.0855914133007,44.,5.19615242270663));
#37568=CARTESIAN_POINT('Ctrl Pts',(-23.918924746634,44.,1.10218211923262E-15));
#37569=CARTESIAN_POINT('Ctrl Pts',(-23.7522580799673,44.,-5.19615242270663));
#37570=CARTESIAN_POINT('Ctrl Pts',(-23.5855914133007,39.5,-7.79422863405995));
#37571=CARTESIAN_POINT('Ctrl Pts',(-23.418924746634,35.,-10.3923048454133));
#37572=CARTESIAN_POINT('Ctrl Pts',(-23.2522580799673,30.5,-7.79422863405995));
#37573=CARTESIAN_POINT('Ctrl Pts',(-23.0855914133007,26.,-5.19615242270663));
#37574=CARTESIAN_POINT('Ctrl Pts',(-22.918924746634,26.,0.));
#37575=CARTESIAN_POINT('Ctrl Pts',(-22.7522580799673,26.,5.19615242270663));
#37576=CARTESIAN_POINT('Ctrl Pts',(-22.5855914133007,30.5,7.79422863405995));
#37577=CARTESIAN_POINT('Ctrl Pts',(-22.418924746634,35.,10.3923048454133));
#37578=CARTESIAN_POINT('Ctrl Pts',(-22.2522580799674,39.5,7.79422863405995));
#37579=CARTESIAN_POINT('Ctrl Pts',(-22.0855914133007,44.,5.19615242270663));
#37580=CARTESIAN_POINT('Ctrl Pts',(-21.918924746634,44.,1.10218211923262E-15));
#37581=CARTESIAN_POINT('Ctrl Pts',(-21.7522580799673,44.,-5.19615242270663));
#37582=CARTESIAN_POINT('Ctrl Pts',(-21.5855914133006,39.5,-7.79422863405995));
#37583=CARTESIAN_POINT('Ctrl Pts',(-21.418924746634,35.,-10.3923048454133));
#37584=CARTESIAN_POINT('Ctrl Pts',(-21.2522580799673,30.5,-7.79422863405995));
#37585=CARTESIAN_POINT('Ctrl Pts',(-21.0855914133007,26.,-5.19615242270663));
#37586=CARTESIAN_POINT('Ctrl Pts',(-20.918924746634,26.,0.));
#37587=CARTESIAN_POINT('Ctrl Pts',(-20.7522580799673,26.,5.19615242270663));
#37588=CARTESIAN_POINT('Ctrl Pts',(-20.5855914133006,30.5,7.79422863405995));
#37589=CARTESIAN_POINT('Ctrl Pts',(-20.418924746634,35.,10.3923048454133));
#37590=CARTESIAN_POINT('Ctrl Pts',(-20.2522580799673,39.5,7.79422863405995));
#37591=CARTESIAN_POINT('Ctrl Pts',(-20.0855914133007,44.,5.19615242270663));
#37592=CARTESIAN_POINT('Ctrl Pts',(-19.918924746634,44.,1.10218211923262E-15));
#37593=CARTESIAN_POINT('Ctrl Pts',(-19.7522580799674,44.,-5.19615242270663));
#37594=CARTESIAN_POINT('Ctrl Pts',(-19.5855914133006,39.5,-7.79422863405995));
#37595=CARTESIAN_POINT('Ctrl Pts',(-19.418924746634,35.,-10.3923048454133));
#37596=CARTESIAN_POINT('Ctrl Pts',(-19.2522580799674,30.5,-7.79422863405995));
#37597=CARTESIAN_POINT('Ctrl Pts',(-19.0855914133007,26.,-5.19615242270663));
#37598=CARTESIAN_POINT('Ctrl Pts',(-18.918924746634,26.,0.));
#37599=CARTESIAN_POINT('Ctrl Pts',(-18.7522580799673,26.,5.19615242270663));
#37600=CARTESIAN_POINT('Ctrl Pts',(-18.5855914133006,30.5,7.79422863405995));
#37601=CARTESIAN_POINT('Ctrl Pts',(-18.418924746634,35.,10.3923048454133));
#37602=CARTESIAN_POINT('Ctrl Pts',(-18.2522580799673,39.5,7.79422863405995));
#37603=CARTESIAN_POINT('Ctrl Pts',(-18.0855914133006,44.,5.19615242270663));
#37604=CARTESIAN_POINT('Ctrl Pts',(-17.918924746634,44.,1.10218211923262E-15));
#37605=CARTESIAN_POINT('Ctrl Pts',(-17.7522580799673,44.,-5.19615242270663));
#37606=CARTESIAN_POINT('Ctrl Pts',(-17.5855914133006,39.5,-7.79422863405995));
#37607=CARTESIAN_POINT('Ctrl Pts',(-17.418924746634,35.,-10.3923048454133));
#37608=CARTESIAN_POINT('Ctrl Pts',(-17.2522580799673,30.5,-7.79422863405995));
#37609=CARTESIAN_POINT('Ctrl Pts',(-17.0855914133007,26.,-5.19615242270663));
#37610=CARTESIAN_POINT('Ctrl Pts',(-16.918924746634,26.,0.));
#37611=CARTESIAN_POINT('Ctrl Pts',(-38.518924746634,26.,0.));
#37612=CARTESIAN_POINT('Ctrl Pts',(-38.3522580799673,26.,5.19615242270663));
#37613=CARTESIAN_POINT('Ctrl Pts',(-38.1855914133007,30.5,7.79422863405995));
#37614=CARTESIAN_POINT('Ctrl Pts',(-38.018924746634,35.,10.3923048454133));
#37615=CARTESIAN_POINT('Ctrl Pts',(-37.8522580799673,39.5,7.79422863405995));
#37616=CARTESIAN_POINT('Ctrl Pts',(-37.6855914133007,44.,5.19615242270663));
#37617=CARTESIAN_POINT('Ctrl Pts',(-37.518924746634,44.,1.10218211923262E-15));
#37618=CARTESIAN_POINT('Ctrl Pts',(-37.3522580799673,44.,-5.19615242270663));
#37619=CARTESIAN_POINT('Ctrl Pts',(-37.1855914133007,39.5,-7.79422863405995));
#37620=CARTESIAN_POINT('Ctrl Pts',(-37.018924746634,35.,-10.3923048454133));
#37621=CARTESIAN_POINT('Ctrl Pts',(-36.8522580799673,30.5,-7.79422863405995));
#37622=CARTESIAN_POINT('Ctrl Pts',(-36.6855914133007,26.,-5.19615242270663));
#37623=CARTESIAN_POINT('Ctrl Pts',(-36.518924746634,26.,0.));
#37624=CARTESIAN_POINT('Ctrl Pts',(-36.3522580799673,26.,5.19615242270663));
#37625=CARTESIAN_POINT('Ctrl Pts',(-36.1855914133007,30.5,7.79422863405995));
#37626=CARTESIAN_POINT('Ctrl Pts',(-36.018924746634,35.,10.3923048454133));
#37627=CARTESIAN_POINT('Ctrl Pts',(-35.8522580799673,39.5,7.79422863405995));
#37628=CARTESIAN_POINT('Ctrl Pts',(-35.6855914133007,44.,5.19615242270663));
#37629=CARTESIAN_POINT('Ctrl Pts',(-35.518924746634,44.,1.10218211923262E-15));
#37630=CARTESIAN_POINT('Ctrl Pts',(-35.3522580799673,44.,-5.19615242270663));
#37631=CARTESIAN_POINT('Ctrl Pts',(-35.1855914133007,39.5,-7.79422863405995));
#37632=CARTESIAN_POINT('Ctrl Pts',(-35.018924746634,35.,-10.3923048454133));
#37633=CARTESIAN_POINT('Ctrl Pts',(-34.8522580799673,30.5,-7.79422863405995));
#37634=CARTESIAN_POINT('Ctrl Pts',(-34.6855914133007,26.,-5.19615242270663));
#37635=CARTESIAN_POINT('Ctrl Pts',(-34.518924746634,26.,0.));
#37636=CARTESIAN_POINT('Ctrl Pts',(-34.3522580799673,26.,5.19615242270663));
#37637=CARTESIAN_POINT('Ctrl Pts',(-34.1855914133007,30.5,7.79422863405995));
#37638=CARTESIAN_POINT('Ctrl Pts',(-34.018924746634,35.,10.3923048454133));
#37639=CARTESIAN_POINT('Ctrl Pts',(-33.8522580799673,39.5,7.79422863405995));
#37640=CARTESIAN_POINT('Ctrl Pts',(-33.6855914133007,44.,5.19615242270663));
#37641=CARTESIAN_POINT('Ctrl Pts',(-33.518924746634,44.,1.10218211923262E-15));
#37642=CARTESIAN_POINT('Ctrl Pts',(-33.3522580799673,44.,-5.19615242270663));
#37643=CARTESIAN_POINT('Ctrl Pts',(-33.1855914133007,39.5,-7.79422863405995));
#37644=CARTESIAN_POINT('Ctrl Pts',(-33.018924746634,35.,-10.3923048454133));
#37645=CARTESIAN_POINT('Ctrl Pts',(-32.8522580799673,30.5,-7.79422863405995));
#37646=CARTESIAN_POINT('Ctrl Pts',(-32.6855914133007,26.,-5.19615242270663));
#37647=CARTESIAN_POINT('Ctrl Pts',(-32.518924746634,26.,0.));
#37648=CARTESIAN_POINT('Ctrl Pts',(-32.3522580799673,26.,5.19615242270663));
#37649=CARTESIAN_POINT('Ctrl Pts',(-32.1855914133007,30.5,7.79422863405995));
#37650=CARTESIAN_POINT('Ctrl Pts',(-32.018924746634,35.,10.3923048454133));
#37651=CARTESIAN_POINT('Ctrl Pts',(-31.8522580799673,39.5,7.79422863405995));
#37652=CARTESIAN_POINT('Ctrl Pts',(-31.6855914133007,44.,5.19615242270663));
#37653=CARTESIAN_POINT('Ctrl Pts',(-31.518924746634,44.,1.10218211923262E-15));
#37654=CARTESIAN_POINT('Ctrl Pts',(-31.3522580799673,44.,-5.19615242270663));
#37655=CARTESIAN_POINT('Ctrl Pts',(-31.1855914133007,39.5,-7.79422863405995));
#37656=CARTESIAN_POINT('Ctrl Pts',(-31.018924746634,35.,-10.3923048454133));
#37657=CARTESIAN_POINT('Ctrl Pts',(-30.8522580799673,30.5,-7.79422863405995));
#37658=CARTESIAN_POINT('Ctrl Pts',(-30.6855914133007,26.,-5.19615242270663));
#37659=CARTESIAN_POINT('Ctrl Pts',(-30.518924746634,26.,0.));
#37660=CARTESIAN_POINT('Ctrl Pts',(-30.3522580799673,26.,5.19615242270663));
#37661=CARTESIAN_POINT('Ctrl Pts',(-30.1855914133007,30.5,7.79422863405995));
#37662=CARTESIAN_POINT('Ctrl Pts',(-30.018924746634,35.,10.3923048454133));
#37663=CARTESIAN_POINT('Ctrl Pts',(-29.8522580799673,39.5,7.79422863405995));
#37664=CARTESIAN_POINT('Ctrl Pts',(-29.6855914133007,44.,5.19615242270663));
#37665=CARTESIAN_POINT('Ctrl Pts',(-29.518924746634,44.,1.10218211923262E-15));
#37666=CARTESIAN_POINT('Ctrl Pts',(-29.3522580799673,44.,-5.19615242270663));
#37667=CARTESIAN_POINT('Ctrl Pts',(-29.1855914133007,39.5,-7.79422863405995));
#37668=CARTESIAN_POINT('Ctrl Pts',(-29.018924746634,35.,-10.3923048454133));
#37669=CARTESIAN_POINT('Ctrl Pts',(-28.8522580799673,30.5,-7.79422863405995));
#37670=CARTESIAN_POINT('Ctrl Pts',(-28.6855914133007,26.,-5.19615242270663));
#37671=CARTESIAN_POINT('Ctrl Pts',(-28.518924746634,26.,0.));
#37672=CARTESIAN_POINT('Ctrl Pts',(-28.3522580799673,26.,5.19615242270663));
#37673=CARTESIAN_POINT('Ctrl Pts',(-28.1855914133007,30.5,7.79422863405995));
#37674=CARTESIAN_POINT('Ctrl Pts',(-28.018924746634,35.,10.3923048454133));
#37675=CARTESIAN_POINT('Ctrl Pts',(-27.8522580799673,39.5,7.79422863405995));
#37676=CARTESIAN_POINT('Ctrl Pts',(-27.6855914133007,44.,5.19615242270663));
#37677=CARTESIAN_POINT('Ctrl Pts',(-27.518924746634,44.,1.10218211923262E-15));
#37678=CARTESIAN_POINT('Ctrl Pts',(-27.3522580799673,44.,-5.19615242270663));
#37679=CARTESIAN_POINT('Ctrl Pts',(-27.1855914133007,39.5,-7.79422863405995));
#37680=CARTESIAN_POINT('Ctrl Pts',(-27.018924746634,35.,-10.3923048454133));
#37681=CARTESIAN_POINT('Ctrl Pts',(-26.8522580799673,30.5,-7.79422863405995));
#37682=CARTESIAN_POINT('Ctrl Pts',(-26.6855914133007,26.,-5.19615242270663));
#37683=CARTESIAN_POINT('Ctrl Pts',(-26.518924746634,26.,0.));
#37684=CARTESIAN_POINT('Ctrl Pts',(-26.3522580799673,26.,5.19615242270663));
#37685=CARTESIAN_POINT('Ctrl Pts',(-26.1855914133007,30.5,7.79422863405995));
#37686=CARTESIAN_POINT('Ctrl Pts',(-26.018924746634,35.,10.3923048454133));
#37687=CARTESIAN_POINT('Ctrl Pts',(-25.8522580799673,39.5,7.79422863405995));
#37688=CARTESIAN_POINT('Ctrl Pts',(-25.6855914133007,44.,5.19615242270663));
#37689=CARTESIAN_POINT('Ctrl Pts',(-25.518924746634,44.,1.10218211923262E-15));
#37690=CARTESIAN_POINT('Ctrl Pts',(-25.3522580799673,44.,-5.19615242270663));
#37691=CARTESIAN_POINT('Ctrl Pts',(-25.1855914133007,39.5,-7.79422863405995));
#37692=CARTESIAN_POINT('Ctrl Pts',(-25.018924746634,35.,-10.3923048454133));
#37693=CARTESIAN_POINT('Ctrl Pts',(-24.8522580799673,30.5,-7.79422863405995));
#37694=CARTESIAN_POINT('Ctrl Pts',(-24.6855914133007,26.,-5.19615242270663));
#37695=CARTESIAN_POINT('Ctrl Pts',(-24.518924746634,26.,0.));
#37696=CARTESIAN_POINT('Ctrl Pts',(-24.3522580799673,26.,5.19615242270663));
#37697=CARTESIAN_POINT('Ctrl Pts',(-24.1855914133007,30.5,7.79422863405995));
#37698=CARTESIAN_POINT('Ctrl Pts',(-24.018924746634,35.,10.3923048454133));
#37699=CARTESIAN_POINT('Ctrl Pts',(-23.8522580799673,39.5,7.79422863405995));
#37700=CARTESIAN_POINT('Ctrl Pts',(-23.6855914133007,44.,5.19615242270663));
#37701=CARTESIAN_POINT('Ctrl Pts',(-23.518924746634,44.,1.10218211923262E-15));
#37702=CARTESIAN_POINT('Ctrl Pts',(-23.3522580799673,44.,-5.19615242270663));
#37703=CARTESIAN_POINT('Ctrl Pts',(-23.1855914133007,39.5,-7.79422863405995));
#37704=CARTESIAN_POINT('Ctrl Pts',(-23.018924746634,35.,-10.3923048454133));
#37705=CARTESIAN_POINT('Ctrl Pts',(-22.8522580799673,30.5,-7.79422863405995));
#37706=CARTESIAN_POINT('Ctrl Pts',(-22.6855914133007,26.,-5.19615242270663));
#37707=CARTESIAN_POINT('Ctrl Pts',(-22.518924746634,26.,0.));
#37708=CARTESIAN_POINT('Ctrl Pts',(-22.3522580799673,26.,5.19615242270663));
#37709=CARTESIAN_POINT('Ctrl Pts',(-22.1855914133007,30.5,7.79422863405995));
#37710=CARTESIAN_POINT('Ctrl Pts',(-22.018924746634,35.,10.3923048454133));
#37711=CARTESIAN_POINT('Ctrl Pts',(-21.8522580799673,39.5,7.79422863405995));
#37712=CARTESIAN_POINT('Ctrl Pts',(-21.6855914133007,44.,5.19615242270663));
#37713=CARTESIAN_POINT('Ctrl Pts',(-21.518924746634,44.,1.10218211923262E-15));
#37714=CARTESIAN_POINT('Ctrl Pts',(-21.3522580799673,44.,-5.19615242270663));
#37715=CARTESIAN_POINT('Ctrl Pts',(-21.1855914133006,39.5,-7.79422863405995));
#37716=CARTESIAN_POINT('Ctrl Pts',(-21.018924746634,35.,-10.3923048454133));
#37717=CARTESIAN_POINT('Ctrl Pts',(-20.8522580799673,30.5,-7.79422863405995));
#37718=CARTESIAN_POINT('Ctrl Pts',(-20.6855914133007,26.,-5.19615242270663));
#37719=CARTESIAN_POINT('Ctrl Pts',(-20.518924746634,26.,0.));
#37720=CARTESIAN_POINT('Ctrl Pts',(-20.3522580799673,26.,5.19615242270663));
#37721=CARTESIAN_POINT('Ctrl Pts',(-20.1855914133006,30.5,7.79422863405995));
#37722=CARTESIAN_POINT('Ctrl Pts',(-20.018924746634,35.,10.3923048454133));
#37723=CARTESIAN_POINT('Ctrl Pts',(-19.8522580799674,39.5,7.79422863405995));
#37724=CARTESIAN_POINT('Ctrl Pts',(-19.6855914133006,44.,5.19615242270663));
#37725=CARTESIAN_POINT('Ctrl Pts',(-19.518924746634,44.,1.10218211923262E-15));
#37726=CARTESIAN_POINT('Ctrl Pts',(-19.3522580799673,44.,-5.19615242270663));
#37727=CARTESIAN_POINT('Ctrl Pts',(-19.1855914133007,39.5,-7.79422863405995));
#37728=CARTESIAN_POINT('Ctrl Pts',(-19.018924746634,35.,-10.3923048454133));
#37729=CARTESIAN_POINT('Ctrl Pts',(-18.8522580799674,30.5,-7.79422863405995));
#37730=CARTESIAN_POINT('Ctrl Pts',(-18.6855914133007,26.,-5.19615242270663));
#37731=CARTESIAN_POINT('Ctrl Pts',(-18.518924746634,26.,-2.20436423846523E-14));
#37732=CARTESIAN_POINT('Ctrl Pts',(-36.918924746634,26.,0.));
#37733=CARTESIAN_POINT('Ctrl Pts',(-36.7522580799673,26.,5.19615242270663));
#37734=CARTESIAN_POINT('Ctrl Pts',(-36.5855914133007,30.5,7.79422863405995));
#37735=CARTESIAN_POINT('Ctrl Pts',(-36.418924746634,35.,10.3923048454133));
#37736=CARTESIAN_POINT('Ctrl Pts',(-36.2522580799673,39.5,7.79422863405995));
#37737=CARTESIAN_POINT('Ctrl Pts',(-36.0855914133007,44.,5.19615242270663));
#37738=CARTESIAN_POINT('Ctrl Pts',(-35.918924746634,44.,1.10218211923262E-15));
#37739=CARTESIAN_POINT('Ctrl Pts',(-35.7522580799673,44.,-5.19615242270663));
#37740=CARTESIAN_POINT('Ctrl Pts',(-35.5855914133007,39.5,-7.79422863405995));
#37741=CARTESIAN_POINT('Ctrl Pts',(-35.418924746634,35.,-10.3923048454133));
#37742=CARTESIAN_POINT('Ctrl Pts',(-35.2522580799673,30.5,-7.79422863405995));
#37743=CARTESIAN_POINT('Ctrl Pts',(-35.0855914133007,26.,-5.19615242270663));
#37744=CARTESIAN_POINT('Ctrl Pts',(-34.918924746634,26.,0.));
#37745=CARTESIAN_POINT('Ctrl Pts',(-34.7522580799673,26.,5.19615242270663));
#37746=CARTESIAN_POINT('Ctrl Pts',(-34.5855914133007,30.5,7.79422863405995));
#37747=CARTESIAN_POINT('Ctrl Pts',(-34.418924746634,35.,10.3923048454133));
#37748=CARTESIAN_POINT('Ctrl Pts',(-34.2522580799673,39.5,7.79422863405995));
#37749=CARTESIAN_POINT('Ctrl Pts',(-34.0855914133007,44.,5.19615242270663));
#37750=CARTESIAN_POINT('Ctrl Pts',(-33.918924746634,44.,1.10218211923262E-15));
#37751=CARTESIAN_POINT('Ctrl Pts',(-33.7522580799673,44.,-5.19615242270663));
#37752=CARTESIAN_POINT('Ctrl Pts',(-33.5855914133007,39.5,-7.79422863405995));
#37753=CARTESIAN_POINT('Ctrl Pts',(-33.418924746634,35.,-10.3923048454133));
#37754=CARTESIAN_POINT('Ctrl Pts',(-33.2522580799673,30.5,-7.79422863405995));
#37755=CARTESIAN_POINT('Ctrl Pts',(-33.0855914133007,26.,-5.19615242270663));
#37756=CARTESIAN_POINT('Ctrl Pts',(-32.918924746634,26.,0.));
#37757=CARTESIAN_POINT('Ctrl Pts',(-32.7522580799673,26.,5.19615242270663));
#37758=CARTESIAN_POINT('Ctrl Pts',(-32.5855914133007,30.5,7.79422863405995));
#37759=CARTESIAN_POINT('Ctrl Pts',(-32.418924746634,35.,10.3923048454133));
#37760=CARTESIAN_POINT('Ctrl Pts',(-32.2522580799673,39.5,7.79422863405995));
#37761=CARTESIAN_POINT('Ctrl Pts',(-32.0855914133007,44.,5.19615242270663));
#37762=CARTESIAN_POINT('Ctrl Pts',(-31.918924746634,44.,1.10218211923262E-15));
#37763=CARTESIAN_POINT('Ctrl Pts',(-31.7522580799673,44.,-5.19615242270663));
#37764=CARTESIAN_POINT('Ctrl Pts',(-31.5855914133007,39.5,-7.79422863405995));
#37765=CARTESIAN_POINT('Ctrl Pts',(-31.418924746634,35.,-10.3923048454133));
#37766=CARTESIAN_POINT('Ctrl Pts',(-31.2522580799673,30.5,-7.79422863405995));
#37767=CARTESIAN_POINT('Ctrl Pts',(-31.0855914133007,26.,-5.19615242270663));
#37768=CARTESIAN_POINT('Ctrl Pts',(-30.918924746634,26.,0.));
#37769=CARTESIAN_POINT('Ctrl Pts',(-30.7522580799673,26.,5.19615242270663));
#37770=CARTESIAN_POINT('Ctrl Pts',(-30.5855914133007,30.5,7.79422863405995));
#37771=CARTESIAN_POINT('Ctrl Pts',(-30.418924746634,35.,10.3923048454133));
#37772=CARTESIAN_POINT('Ctrl Pts',(-30.2522580799673,39.5,7.79422863405995));
#37773=CARTESIAN_POINT('Ctrl Pts',(-30.0855914133007,44.,5.19615242270663));
#37774=CARTESIAN_POINT('Ctrl Pts',(-29.918924746634,44.,1.10218211923262E-15));
#37775=CARTESIAN_POINT('Ctrl Pts',(-29.7522580799673,44.,-5.19615242270663));
#37776=CARTESIAN_POINT('Ctrl Pts',(-29.5855914133007,39.5,-7.79422863405995));
#37777=CARTESIAN_POINT('Ctrl Pts',(-29.418924746634,35.,-10.3923048454133));
#37778=CARTESIAN_POINT('Ctrl Pts',(-29.2522580799673,30.5,-7.79422863405995));
#37779=CARTESIAN_POINT('Ctrl Pts',(-29.0855914133007,26.,-5.19615242270663));
#37780=CARTESIAN_POINT('Ctrl Pts',(-28.918924746634,26.,0.));
#37781=CARTESIAN_POINT('Ctrl Pts',(-28.7522580799673,26.,5.19615242270663));
#37782=CARTESIAN_POINT('Ctrl Pts',(-28.5855914133007,30.5,7.79422863405995));
#37783=CARTESIAN_POINT('Ctrl Pts',(-28.418924746634,35.,10.3923048454133));
#37784=CARTESIAN_POINT('Ctrl Pts',(-28.2522580799673,39.5,7.79422863405995));
#37785=CARTESIAN_POINT('Ctrl Pts',(-28.0855914133007,44.,5.19615242270663));
#37786=CARTESIAN_POINT('Ctrl Pts',(-27.918924746634,44.,1.10218211923262E-15));
#37787=CARTESIAN_POINT('Ctrl Pts',(-27.7522580799673,44.,-5.19615242270663));
#37788=CARTESIAN_POINT('Ctrl Pts',(-27.5855914133007,39.5,-7.79422863405995));
#37789=CARTESIAN_POINT('Ctrl Pts',(-27.418924746634,35.,-10.3923048454133));
#37790=CARTESIAN_POINT('Ctrl Pts',(-27.2522580799673,30.5,-7.79422863405995));
#37791=CARTESIAN_POINT('Ctrl Pts',(-27.0855914133007,26.,-5.19615242270663));
#37792=CARTESIAN_POINT('Ctrl Pts',(-26.918924746634,26.,0.));
#37793=CARTESIAN_POINT('Ctrl Pts',(-26.7522580799673,26.,5.19615242270663));
#37794=CARTESIAN_POINT('Ctrl Pts',(-26.5855914133007,30.5,7.79422863405995));
#37795=CARTESIAN_POINT('Ctrl Pts',(-26.418924746634,35.,10.3923048454133));
#37796=CARTESIAN_POINT('Ctrl Pts',(-26.2522580799673,39.5,7.79422863405995));
#37797=CARTESIAN_POINT('Ctrl Pts',(-26.0855914133007,44.,5.19615242270663));
#37798=CARTESIAN_POINT('Ctrl Pts',(-25.918924746634,44.,1.10218211923262E-15));
#37799=CARTESIAN_POINT('Ctrl Pts',(-25.7522580799673,44.,-5.19615242270663));
#37800=CARTESIAN_POINT('Ctrl Pts',(-25.5855914133007,39.5,-7.79422863405995));
#37801=CARTESIAN_POINT('Ctrl Pts',(-25.418924746634,35.,-10.3923048454133));
#37802=CARTESIAN_POINT('Ctrl Pts',(-25.2522580799673,30.5,-7.79422863405995));
#37803=CARTESIAN_POINT('Ctrl Pts',(-25.0855914133007,26.,-5.19615242270663));
#37804=CARTESIAN_POINT('Ctrl Pts',(-24.918924746634,26.,0.));
#37805=CARTESIAN_POINT('Ctrl Pts',(-24.7522580799673,26.,5.19615242270663));
#37806=CARTESIAN_POINT('Ctrl Pts',(-24.5855914133007,30.5,7.79422863405995));
#37807=CARTESIAN_POINT('Ctrl Pts',(-24.418924746634,35.,10.3923048454133));
#37808=CARTESIAN_POINT('Ctrl Pts',(-24.2522580799673,39.5,7.79422863405995));
#37809=CARTESIAN_POINT('Ctrl Pts',(-24.0855914133007,44.,5.19615242270663));
#37810=CARTESIAN_POINT('Ctrl Pts',(-23.918924746634,44.,1.10218211923262E-15));
#37811=CARTESIAN_POINT('Ctrl Pts',(-23.7522580799673,44.,-5.19615242270663));
#37812=CARTESIAN_POINT('Ctrl Pts',(-23.5855914133007,39.5,-7.79422863405995));
#37813=CARTESIAN_POINT('Ctrl Pts',(-23.418924746634,35.,-10.3923048454133));
#37814=CARTESIAN_POINT('Ctrl Pts',(-23.2522580799673,30.5,-7.79422863405995));
#37815=CARTESIAN_POINT('Ctrl Pts',(-23.0855914133007,26.,-5.19615242270663));
#37816=CARTESIAN_POINT('Ctrl Pts',(-22.918924746634,26.,0.));
#37817=CARTESIAN_POINT('Ctrl Pts',(-22.7522580799673,26.,5.19615242270663));
#37818=CARTESIAN_POINT('Ctrl Pts',(-22.5855914133007,30.5,7.79422863405995));
#37819=CARTESIAN_POINT('Ctrl Pts',(-22.418924746634,35.,10.3923048454133));
#37820=CARTESIAN_POINT('Ctrl Pts',(-22.2522580799674,39.5,7.79422863405995));
#37821=CARTESIAN_POINT('Ctrl Pts',(-22.0855914133007,44.,5.19615242270663));
#37822=CARTESIAN_POINT('Ctrl Pts',(-21.918924746634,44.,1.10218211923262E-15));
#37823=CARTESIAN_POINT('Ctrl Pts',(-21.7522580799673,44.,-5.19615242270663));
#37824=CARTESIAN_POINT('Ctrl Pts',(-21.5855914133006,39.5,-7.79422863405995));
#37825=CARTESIAN_POINT('Ctrl Pts',(-21.418924746634,35.,-10.3923048454133));
#37826=CARTESIAN_POINT('Ctrl Pts',(-21.2522580799673,30.5,-7.79422863405995));
#37827=CARTESIAN_POINT('Ctrl Pts',(-21.0855914133007,26.,-5.19615242270663));
#37828=CARTESIAN_POINT('Ctrl Pts',(-20.918924746634,26.,0.));
#37829=CARTESIAN_POINT('Ctrl Pts',(-20.7522580799673,26.,5.19615242270663));
#37830=CARTESIAN_POINT('Ctrl Pts',(-20.5855914133006,30.5,7.79422863405995));
#37831=CARTESIAN_POINT('Ctrl Pts',(-20.418924746634,35.,10.3923048454133));
#37832=CARTESIAN_POINT('Ctrl Pts',(-20.2522580799673,39.5,7.79422863405995));
#37833=CARTESIAN_POINT('Ctrl Pts',(-20.0855914133007,44.,5.19615242270663));
#37834=CARTESIAN_POINT('Ctrl Pts',(-19.918924746634,44.,1.10218211923262E-15));
#37835=CARTESIAN_POINT('Ctrl Pts',(-19.7522580799674,44.,-5.19615242270663));
#37836=CARTESIAN_POINT('Ctrl Pts',(-19.5855914133006,39.5,-7.79422863405995));
#37837=CARTESIAN_POINT('Ctrl Pts',(-19.418924746634,35.,-10.3923048454133));
#37838=CARTESIAN_POINT('Ctrl Pts',(-19.2522580799674,30.5,-7.79422863405995));
#37839=CARTESIAN_POINT('Ctrl Pts',(-19.0855914133007,26.,-5.19615242270663));
#37840=CARTESIAN_POINT('Ctrl Pts',(-18.918924746634,26.,0.));
#37841=CARTESIAN_POINT('Ctrl Pts',(-18.7522580799673,26.,5.19615242270663));
#37842=CARTESIAN_POINT('Ctrl Pts',(-18.5855914133006,30.5,7.79422863405995));
#37843=CARTESIAN_POINT('Ctrl Pts',(-18.418924746634,35.,10.3923048454133));
#37844=CARTESIAN_POINT('Ctrl Pts',(-18.2522580799673,39.5,7.79422863405995));
#37845=CARTESIAN_POINT('Ctrl Pts',(-18.0855914133006,44.,5.19615242270663));
#37846=CARTESIAN_POINT('Ctrl Pts',(-17.918924746634,44.,1.10218211923262E-15));
#37847=CARTESIAN_POINT('Ctrl Pts',(-17.7522580799673,44.,-5.19615242270663));
#37848=CARTESIAN_POINT('Ctrl Pts',(-17.5855914133006,39.5,-7.79422863405995));
#37849=CARTESIAN_POINT('Ctrl Pts',(-17.418924746634,35.,-10.3923048454133));
#37850=CARTESIAN_POINT('Ctrl Pts',(-17.2522580799673,30.5,-7.79422863405995));
#37851=CARTESIAN_POINT('Ctrl Pts',(-17.0855914133007,26.,-5.19615242270663));
#37852=CARTESIAN_POINT('Ctrl Pts',(-16.918924746634,26.,-2.20436423846523E-14));
#37853=CARTESIAN_POINT('Ctrl Pts',(-16.9340264307573,17.163528852123,6.73969634090002));
#37854=CARTESIAN_POINT('Ctrl Pts',(-16.9457712867961,17.2557485214382,6.26075296190838));
#37855=CARTESIAN_POINT('Ctrl Pts',(-17.4245878781802,17.16390605946,6.24262002709426));
#37856=CARTESIAN_POINT('Ctrl Pts',(-16.9238487697737,17.1121753468508,6.73379116642023));
#37857=CARTESIAN_POINT('Ctrl Pts',(-16.9318068964855,17.2064962780678,6.25102883540689));
#37858=CARTESIAN_POINT('Ctrl Pts',(-17.420771254245,17.144754794966,6.23883889336594));
#37859=CARTESIAN_POINT('Ctrl Pts',(-16.9188836705717,17.0606673879271,6.72780634103384));
#37860=CARTESIAN_POINT('Ctrl Pts',(-16.9228736444101,17.1565405083055,6.24116580803177));
#37861=CARTESIAN_POINT('Ctrl Pts',(-17.4189093402838,17.1255458393,6.23504636936957));
#37862=CARTESIAN_POINT('Ctrl Pts',(-16.9189456649685,16.983243156343,6.7187202593339));
#37863=CARTESIAN_POINT('Ctrl Pts',(-16.9168638503772,17.0804387429173,6.22614064079103));
#37864=CARTESIAN_POINT('Ctrl Pts',(-17.4189325924229,17.0966716564302,6.22934558931084));
#37865=CARTESIAN_POINT('Ctrl Pts',(-16.9202265012116,16.9574044014087,6.7156730067294));
#37866=CARTESIAN_POINT('Ctrl Pts',(-16.9161095341114,17.0547943482532,6.22107753461143));
#37867=CARTESIAN_POINT('Ctrl Pts',(-17.4194128979399,17.0870354499882,6.22744306296841));
#37868=CARTESIAN_POINT('Ctrl Pts',(-16.9240802930149,16.9185992377109,6.71107449121992));
#37869=CARTESIAN_POINT('Ctrl Pts',(-16.9169275550253,17.0160227636108,6.21342265905803));
#37870=CARTESIAN_POINT('Ctrl Pts',(-17.4208580798572,17.0725635360787,6.22458579775681));
#37871=CARTESIAN_POINT('Ctrl Pts',(-16.9256893119182,16.905644695499,6.70953565876855));
#37872=CARTESIAN_POINT('Ctrl Pts',(-16.9175289419495,17.0030164596971,6.21085475684852));
#37873=CARTESIAN_POINT('Ctrl Pts',(-17.4214614628586,17.0677322859808,6.22363193892933));
#37874=CARTESIAN_POINT('Ctrl Pts',(-16.9295597285367,16.8797683534593,6.70645460032402));
#37875=CARTESIAN_POINT('Ctrl Pts',(-16.919402781573,16.9769365576265,6.20570566617719));
#37876=CARTESIAN_POINT('Ctrl Pts',(-17.4229128606045,17.0580819710591,6.22172662707637));
#37877=CARTESIAN_POINT('Ctrl Pts',(-16.9318080465975,16.8669299669448,6.70492231261218));
#37878=CARTESIAN_POINT('Ctrl Pts',(-16.9206699203638,16.9639474234362,6.20314115387546));
#37879=CARTESIAN_POINT('Ctrl Pts',(-17.4237559870977,17.0532940171532,6.2207813164412));
#37880=CARTESIAN_POINT('Ctrl Pts',(-16.9445834894833,16.8032276683107,6.69730199287355));
#37881=CARTESIAN_POINT('Ctrl Pts',(-16.928658984358,16.8990583262999,6.1903297620293));
#37882=CARTESIAN_POINT('Ctrl Pts',(-17.4285467632928,17.0295367820529,6.2160908019868));
#37883=CARTESIAN_POINT('Ctrl Pts',(-16.9596689585237,16.7538180319705,6.69133567597977));
#37884=CARTESIAN_POINT('Ctrl Pts',(-16.9402496119177,16.8481169540716,6.18027214203455));
#37885=CARTESIAN_POINT('Ctrl Pts',(-17.4342038179283,17.0111096783419,6.21245264308723));
#37886=CARTESIAN_POINT('Ctrl Pts',(-16.9845527746887,16.6939788697473,6.6840528001532));
#37887=CARTESIAN_POINT('Ctrl Pts',(-16.9613133035777,16.7857105312913,6.16795091749546));
#37888=CARTESIAN_POINT('Ctrl Pts',(-17.4435352591956,16.9887926775086,6.20804648157282));
#37889=CARTESIAN_POINT('Ctrl Pts',(-16.9898335783274,16.6821080424272,6.68260507125331));
#37890=CARTESIAN_POINT('Ctrl Pts',(-16.9658750845434,16.7732516839765,6.16549110248884));
#37891=CARTESIAN_POINT('Ctrl Pts',(-17.4455155553034,16.984365439009,6.2071723888559));
#37892=CARTESIAN_POINT('Ctrl Pts',(-17.0010129029441,16.6585634598165,6.6797280266418));
#37893=CARTESIAN_POINT('Ctrl Pts',(-16.9756875213553,16.7484542773758,6.16059522156661));
#37894=CARTESIAN_POINT('Ctrl Pts',(-17.4497078084659,16.9755844415616,6.20543871087201));
#37895=CARTESIAN_POINT('Ctrl Pts',(-17.0069205341199,16.6468728289804,6.67829663781084));
#37896=CARTESIAN_POINT('Ctrl Pts',(-16.9809474116785,16.7360985023473,6.15815575665741));
#37897=CARTESIAN_POINT('Ctrl Pts',(-17.4519231707424,16.9712243839561,6.20457788202832));
#37898=CARTESIAN_POINT('Ctrl Pts',(-17.0255319975721,16.6122139276746,6.67404499554267));
#37899=CARTESIAN_POINT('Ctrl Pts',(-16.9977536936298,16.6993085573344,6.15089212651984));
#37900=CARTESIAN_POINT('Ctrl Pts',(-17.4589024581334,16.9582981905475,6.20202579645239));
#37901=CARTESIAN_POINT('Ctrl Pts',(-17.0389887268156,16.5898976324254,6.67129663775293));
#37902=CARTESIAN_POINT('Ctrl Pts',(-17.0101778412151,16.6754791025347,6.14618735335466));
#37903=CARTESIAN_POINT('Ctrl Pts',(-17.4639487418597,16.9499751842962,6.20038254205175));
#37904=CARTESIAN_POINT('Ctrl Pts',(-17.0824066515609,16.5252426617237,6.66330736417787));
#37905=CARTESIAN_POINT('Ctrl Pts',(-17.051127346388,16.6058793480108,6.13244591192685));
#37906=CARTESIAN_POINT('Ctrl Pts',(-17.4802304556663,16.925861531581,6.19562165821438));
#37907=CARTESIAN_POINT('Ctrl Pts',(-17.1153868669716,16.4851763244393,6.65831969837799));
#37908=CARTESIAN_POINT('Ctrl Pts',(-17.0831880908469,16.5622697417389,6.12383584060727));
#37909=CARTESIAN_POINT('Ctrl Pts',(-17.4925980312227,16.9109182299925,6.19267132448229));
#37910=CARTESIAN_POINT('Ctrl Pts',(-17.1571321085461,16.443595731894,6.65311644401699));
#37911=CARTESIAN_POINT('Ctrl Pts',(-17.1247289364465,16.5166242121387,6.11482380635895));
#37912=CARTESIAN_POINT('Ctrl Pts',(-17.5082525086683,16.8954100189695,6.18960945774325));
#37913=CARTESIAN_POINT('Ctrl Pts',(-17.1618355598308,16.4390246579602,6.6525440228328));
#37914=CARTESIAN_POINT('Ctrl Pts',(-17.1294344256378,16.5115867952363,6.11382924294728));
#37915=CARTESIAN_POINT('Ctrl Pts',(-17.5100163000558,16.8937051501344,6.18927285662447));
#37916=CARTESIAN_POINT('Ctrl Pts',(-17.171374097915,16.4299815745484,6.65141081135807));
#37917=CARTESIAN_POINT('Ctrl Pts',(-17.1390037634447,16.5016077877741,6.11185903561698));
#37918=CARTESIAN_POINT('Ctrl Pts',(-17.5135932548913,16.8903323645726,6.18860695003381));
#37919=CARTESIAN_POINT('Ctrl Pts',(-17.1762161790489,16.425503359408,6.65084924015553));
#37920=CARTESIAN_POINT('Ctrl Pts',(-17.1438746821593,16.4966594486413,6.11088205929252));
#37921=CARTESIAN_POINT('Ctrl Pts',(-17.5154090352215,16.8886621272269,6.18827718639005));
#37922=CARTESIAN_POINT('Ctrl Pts',(-17.190879548413,16.4122753689571,6.64918933918175));
#37923=CARTESIAN_POINT('Ctrl Pts',(-17.1586695817608,16.4820186331741,6.10799144696816));
#37924=CARTESIAN_POINT('Ctrl Pts',(-17.5209077944372,16.8837284797184,6.18730311070934));
#37925=CARTESIAN_POINT('Ctrl Pts',(-17.2008371206551,16.4037311294511,6.64811568767107));
#37926=CARTESIAN_POINT('Ctrl Pts',(-17.1687645001098,16.4725403371964,6.10612009770977));
#37927=CARTESIAN_POINT('Ctrl Pts',(-17.5246418887157,16.8805417313108,6.18667393440136));
#37928=CARTESIAN_POINT('Ctrl Pts',(-17.2312453506019,16.3789058423747,6.64499241842953));
#37929=CARTESIAN_POINT('Ctrl Pts',(-17.1997603324787,16.4449156410009,6.100666010302));
#37930=CARTESIAN_POINT('Ctrl Pts',(-17.5360449694744,16.8712825880367,6.18484585360074));
#37931=CARTESIAN_POINT('Ctrl Pts',(-17.2522302391352,16.3634303224513,6.64304026443391));
#37932=CARTESIAN_POINT('Ctrl Pts',(-17.2213294853766,16.4276216694408,6.09725157157484));
#37933=CARTESIAN_POINT('Ctrl Pts',(-17.5439143065422,16.8655106243265,6.18370626479344));
#37934=CARTESIAN_POINT('Ctrl Pts',(-17.2956019395641,16.3345930464113,6.63939537781673));
#37935=CARTESIAN_POINT('Ctrl Pts',(-17.2662656597083,16.3952572162235,6.09086168929334));
#37936=CARTESIAN_POINT('Ctrl Pts',(-17.5601786937626,16.8547550179788,6.18158272950716));
#37937=CARTESIAN_POINT('Ctrl Pts',(-17.3179887637184,16.3212313140015,6.63770263755943));
#37938=CARTESIAN_POINT('Ctrl Pts',(-17.2896291828443,16.3801970928505,6.08788829082891));
#37939=CARTESIAN_POINT('Ctrl Pts',(-17.5685737507052,16.8497713855231,6.18059878503843));
#37940=CARTESIAN_POINT('Ctrl Pts',(-17.3526333624528,16.3027934739649,6.63536298725943));
#37941=CARTESIAN_POINT('Ctrl Pts',(-17.3260026650614,16.3593493456032,6.08377221168955));
#37942=CARTESIAN_POINT('Ctrl Pts',(-17.5815654787338,16.8428944620486,6.17924103827948));
#37943=CARTESIAN_POINT('Ctrl Pts',(-17.364359267792,16.296915463442,6.63461640073939));
#37944=CARTESIAN_POINT('Ctrl Pts',(-17.3383566078206,16.3526877545169,6.08245697912365));
#37945=CARTESIAN_POINT('Ctrl Pts',(-17.5859626904173,16.8407020762296,6.17880818414767));
#37946=CARTESIAN_POINT('Ctrl Pts',(-17.3822192836592,16.2885072643732,6.6335476194421));
#37947=CARTESIAN_POINT('Ctrl Pts',(-17.3572223204219,16.3431449083558,6.08057288538689));
#37948=CARTESIAN_POINT('Ctrl Pts',(-17.5926601988439,16.8375659857744,6.17818900950262));
#37949=CARTESIAN_POINT('Ctrl Pts',(-17.3882178337638,16.285772701414,6.63319987789834));
#37950=CARTESIAN_POINT('Ctrl Pts',(-17.3635686188785,16.3400380551801,6.07995948320997));
#37951=CARTESIAN_POINT('Ctrl Pts',(-17.5949096533811,16.8365460418669,6.17798763667366));
#37952=CARTESIAN_POINT('Ctrl Pts',(-17.4003064009864,16.2804414700918,6.6325216769544));
#37953=CARTESIAN_POINT('Ctrl Pts',(-17.3763747964082,16.3339762671101,6.07876267287232));
#37954=CARTESIAN_POINT('Ctrl Pts',(-17.5994428679428,16.8345575960637,6.17759504747957));
#37955=CARTESIAN_POINT('Ctrl Pts',(-17.4064014619839,16.2778429556048,6.63219098038768));
#37956=CARTESIAN_POINT('Ctrl Pts',(-17.3828399484087,16.3310193192068,6.07817886727278));
#37957=CARTESIAN_POINT('Ctrl Pts',(-17.6017285156952,16.8335883975106,6.17740369356977));
#37958=CARTESIAN_POINT('Ctrl Pts',(-17.4613673391331,16.2552073371804,6.6293092707837));
#37959=CARTESIAN_POINT('Ctrl Pts',(-17.4412943532773,16.305207075037,6.07308262169252));
#37960=CARTESIAN_POINT('Ctrl Pts',(-17.6223407123812,16.8251457010694,6.17573680811258));
#37961=CARTESIAN_POINT('Ctrl Pts',(-17.5114824250486,16.2401548090555,6.62738600694331));
#37962=CARTESIAN_POINT('Ctrl Pts',(-17.4949832638486,16.2879639917577,6.06967823010323));
#37963=CARTESIAN_POINT('Ctrl Pts',(-17.6411338750825,16.8195313396363,6.17462833554231));
#37964=CARTESIAN_POINT('Ctrl Pts',(-17.5884810370651,16.2249404862174,6.62544067878907));
#37965=CARTESIAN_POINT('Ctrl Pts',(-17.5778953266643,16.270488978075,6.06622804728844));
#37966=CARTESIAN_POINT('Ctrl Pts',(-17.6700083560242,16.8138566171136,6.17350794556827));
#37967=CARTESIAN_POINT('Ctrl Pts',(-17.61445379365,16.2211054438284,6.6249498806517));
#37968=CARTESIAN_POINT('Ctrl Pts',(-17.6059331605785,16.2660757431219,6.06535671936452));
#37969=CARTESIAN_POINT('Ctrl Pts',(-17.6797481384879,16.8124261864561,6.17322552820585));
#37970=CARTESIAN_POINT('Ctrl Pts',(-17.6538857988551,16.217259998137,6.62445766257136));
#37971=CARTESIAN_POINT('Ctrl Pts',(-17.6485546296303,16.2616476106312,6.06448245014227));
#37972=CARTESIAN_POINT('Ctrl Pts',(-17.6945351416054,16.8109918968226,6.17294234894575));
#37973=CARTESIAN_POINT('Ctrl Pts',(-17.6671432193907,16.2162960247729,6.6243342451152));
#37974=CARTESIAN_POINT('Ctrl Pts',(-17.6628934486627,16.2605370299517,6.06426318242413));
#37975=CARTESIAN_POINT('Ctrl Pts',(-17.6995066741152,16.810632347174,6.1728713611891));
#37976=CARTESIAN_POINT('Ctrl Pts',(-17.6935540371893,16.2150298143844,6.62417212417057));
#37977=CARTESIAN_POINT('Ctrl Pts',(-17.691468213857,16.2590779435578,6.06397510741069));
#37978=CARTESIAN_POINT('Ctrl Pts',(-17.7094107303948,16.8101600586753,6.17277811481509));
#37979=CARTESIAN_POINT('Ctrl Pts',(-17.7067266210675,16.2147239146772,6.62413295366647));
#37980=CARTESIAN_POINT('Ctrl Pts',(-17.7057234775305,16.2587254085436,6.06390550458979));
#37981=CARTESIAN_POINT('Ctrl Pts',(-17.7143504495434,16.8100459686567,6.1727555894295));
#37982=CARTESIAN_POINT('Ctrl Pts',(-17.7724284272708,16.2148007635293,6.6241427921321));
#37983=CARTESIAN_POINT('Ctrl Pts',(-17.7768280969853,16.2588139364961,6.06392298312376));
#37984=CARTESIAN_POINT('Ctrl Pts',(-17.7389886268855,16.8100746189498,6.17276124600583));
#37985=CARTESIAN_POINT('Ctrl Pts',(-17.8244788813812,16.2199564028495,6.62480342778294));
#37986=CARTESIAN_POINT('Ctrl Pts',(-17.8331128420917,16.2647554475499,6.06509604654469));
#37987=CARTESIAN_POINT('Ctrl Pts',(-17.7585075492867,16.8119976109921,6.17314091232356));
#37988=CARTESIAN_POINT('Ctrl Pts',(-17.8889031485325,16.2327695523612,6.62644171019872));
#37989=CARTESIAN_POINT('Ctrl Pts',(-17.90254892953,16.2794864647711,6.06800446787037));
#37990=CARTESIAN_POINT('Ctrl Pts',(-17.7826666468153,16.816776749508,6.17408448249046));
#37991=CARTESIAN_POINT('Ctrl Pts',(-17.9017557691567,16.2356534961519,6.62681033151498));
#37992=CARTESIAN_POINT('Ctrl Pts',(-17.9163762099596,16.2827975605751,6.06865819473137));
#37993=CARTESIAN_POINT('Ctrl Pts',(-17.7874863810826,16.81785241274,6.1742968562754));
#37994=CARTESIAN_POINT('Ctrl Pts',(-17.9273953632276,16.2420759339317,6.62763082558797));
#37995=CARTESIAN_POINT('Ctrl Pts',(-17.9439205439042,16.2901643089726,6.07011265017177));
#37996=CARTESIAN_POINT('Ctrl Pts',(-17.797101226854,16.82024789507,6.17476980880739));
#37997=CARTESIAN_POINT('Ctrl Pts',(-17.9401902056257,16.2456190784938,6.62808328938417));
#37998=CARTESIAN_POINT('Ctrl Pts',(-17.9576446533942,16.294224513599,6.07091427748269));
#37999=CARTESIAN_POINT('Ctrl Pts',(-17.8018992926118,16.8215694340713,6.17503072712393));
#38000=CARTESIAN_POINT('Ctrl Pts',(-17.9780466892305,16.2571128882123,6.62955018787334));
#38001=CARTESIAN_POINT('Ctrl Pts',(-17.9981679747951,16.3073767581212,6.07351099350535));
#38002=CARTESIAN_POINT('Ctrl Pts',(-17.8160954773958,16.8258564334959,6.17587713171108));
#38003=CARTESIAN_POINT('Ctrl Pts',(-18.0027258637711,16.2659587403489,6.63067809312904));
#38004=CARTESIAN_POINT('Ctrl Pts',(-18.0244924260245,16.317478878484,6.07550550765576));
#38005=CARTESIAN_POINT('Ctrl Pts',(-17.825350164657,16.8291557994221,6.17652854268134));
#38006=CARTESIAN_POINT('Ctrl Pts',(-18.0751331263037,16.2959506337827,6.63449608491444));
#38007=CARTESIAN_POINT('Ctrl Pts',(-18.1013159720922,16.3516027063543,6.08224275242306));
#38008=CARTESIAN_POINT('Ctrl Pts',(-17.852502890817,16.8403422289135,6.17873713762098));
#38009=CARTESIAN_POINT('Ctrl Pts',(-18.1212467327399,16.3205175212379,6.63761658916437));
#38010=CARTESIAN_POINT('Ctrl Pts',(-18.1497601127687,16.3794086658638,6.0877326275894));
#38011=CARTESIAN_POINT('Ctrl Pts',(-17.8697955008785,16.8495051762018,6.18054622594794));
#38012=CARTESIAN_POINT('Ctrl Pts',(-18.1706160636699,16.3534706885993,6.6417813765152));
#38013=CARTESIAN_POINT('Ctrl Pts',(-18.2009972681976,16.4164599843371,6.09504786204832));
#38014=CARTESIAN_POINT('Ctrl Pts',(-17.8883089893406,16.8617959232122,6.18297285203741));
#38015=CARTESIAN_POINT('Ctrl Pts',(-18.1760670536863,16.3572075290665,6.64225340483513));
#38016=CARTESIAN_POINT('Ctrl Pts',(-18.2066322253776,16.4206486705888,6.09587485615456));
#38017=CARTESIAN_POINT('Ctrl Pts',(-17.8903531105129,16.863189672331,6.18324802717289));
#38018=CARTESIAN_POINT('Ctrl Pts',(-18.1868377701863,16.3647884998207,6.64321046159106));
#38019=CARTESIAN_POINT('Ctrl Pts',(-18.2177440408947,16.4291367290659,6.09755069767437));
#38020=CARTESIAN_POINT('Ctrl Pts',(-17.8943921317318,16.8660171798007,6.18380627667459));
#38021=CARTESIAN_POINT('Ctrl Pts',(-18.1921652410117,16.3686376965469,6.64369613249193));
#38022=CARTESIAN_POINT('Ctrl Pts',(-18.2232288896621,16.4334416698043,6.09840064450838));
#38023=CARTESIAN_POINT('Ctrl Pts',(-17.8963899309271,16.8674528346187,6.18408972547016));
#38024=CARTESIAN_POINT('Ctrl Pts',(-18.2079758853082,16.380359521441,6.64517424754474));
#38025=CARTESIAN_POINT('Ctrl Pts',(-18.2394674114616,16.4465321648978,6.10098516902028));
#38026=CARTESIAN_POINT('Ctrl Pts',(-17.902318925834,16.8718247643677,6.18495289829289));
#38027=CARTESIAN_POINT('Ctrl Pts',(-18.2182873888224,16.3884062672933,6.64618778634462));
#38028=CARTESIAN_POINT('Ctrl Pts',(-18.250014828929,16.4555003709746,6.10275580857727));
#38029=CARTESIAN_POINT('Ctrl Pts',(-17.9061857359879,16.8748259873231,6.18554544534619));
#38030=CARTESIAN_POINT('Ctrl Pts',(-18.2485461467234,16.4132319441657,6.6493107176117));
#38031=CARTESIAN_POINT('Ctrl Pts',(-18.2808046004885,16.4830834508249,6.10820167945361));
#38032=CARTESIAN_POINT('Ctrl Pts',(-17.917532774601,16.884085261647,6.18737355202065));
#38033=CARTESIAN_POINT('Ctrl Pts',(-18.2678192302634,16.4306946934602,6.65150224599118));
#38034=CARTESIAN_POINT('Ctrl Pts',(-18.3002353052696,16.5024028462849,6.11201600815278));
#38035=CARTESIAN_POINT('Ctrl Pts',(-17.9247601784908,16.8905983462382,6.18865946417705));
#38036=CARTESIAN_POINT('Ctrl Pts',(-18.304585320563,16.4674258171909,6.65609825686814));
#38037=CARTESIAN_POINT('Ctrl Pts',(-18.3369000788844,16.5428190986578,6.11999559900783));
#38038=CARTESIAN_POINT('Ctrl Pts',(-17.9385474613616,16.9042978717687,6.19136423273484));
#38039=CARTESIAN_POINT('Ctrl Pts',(-18.32207835827,16.4866941560064,6.65850274672427));
#38040=CARTESIAN_POINT('Ctrl Pts',(-18.3541350222299,16.5639050113827,6.12415870039582));
#38041=CARTESIAN_POINT('Ctrl Pts',(-17.9451073556682,16.9114842972485,6.19278308608398));
#38042=CARTESIAN_POINT('Ctrl Pts',(-18.3469582555341,16.5169758809527,6.6622690907101));
#38043=CARTESIAN_POINT('Ctrl Pts',(-18.3783360711151,16.5968717741023,6.13066749977414));
#38044=CARTESIAN_POINT('Ctrl Pts',(-17.9544373101362,16.9227782767883,6.1950129151889));
#38045=CARTESIAN_POINT('Ctrl Pts',(-18.3550268290823,16.5273031516405,6.66355157018222));
#38046=CARTESIAN_POINT('Ctrl Pts',(-18.3861205298441,16.6080723020181,6.13287887823903));
#38047=CARTESIAN_POINT('Ctrl Pts',(-17.9574630272311,16.9266299573578,6.19577337251102));
#38048=CARTESIAN_POINT('Ctrl Pts',(-18.3706915223259,16.5484153134749,6.66616886023153));
#38049=CARTESIAN_POINT('Ctrl Pts',(-18.4011144492354,16.6308981776041,6.13738550954182));
#38050=CARTESIAN_POINT('Ctrl Pts',(-17.9633372878401,16.934503971749,6.19732798011414));
#38051=CARTESIAN_POINT('Ctrl Pts',(-18.3782309891514,16.5591238170816,6.66749420161781));
#38052=CARTESIAN_POINT('Ctrl Pts',(-18.4082702147513,16.6424396756498,6.13966420751237));
#38053=CARTESIAN_POINT('Ctrl Pts',(-17.9661645847443,16.9384978169065,6.19811650573006));
#38054=CARTESIAN_POINT('Ctrl Pts',(-18.4144652239087,16.6133698763481,6.67419609590586));
#38055=CARTESIAN_POINT('Ctrl Pts',(-18.4422698693699,16.7005708871118,6.15114135485145));
#38056=CARTESIAN_POINT('Ctrl Pts',(-17.9797524369468,16.9587293525346,6.20211092300537));
#38057=CARTESIAN_POINT('Ctrl Pts',(-18.4388454391431,16.6590429087733,6.67980148969806));
#38058=CARTESIAN_POINT('Ctrl Pts',(-18.4642277040733,16.7490077862942,6.16070450371041));
#38059=CARTESIAN_POINT('Ctrl Pts',(-17.9888950132745,16.975763316277,6.20547402703715));
#38060=CARTESIAN_POINT('Ctrl Pts',(-18.4636539969267,16.7189339970101,6.68708985334279));
#38061=CARTESIAN_POINT('Ctrl Pts',(-18.4853233274594,16.811806410725,6.17310316266067));
#38062=CARTESIAN_POINT('Ctrl Pts',(-17.9981982137564,16.9980996869273,6.20988401283525));
#38063=CARTESIAN_POINT('Ctrl Pts',(-18.4683298236966,16.7310534611065,6.68856175184365));
#38064=CARTESIAN_POINT('Ctrl Pts',(-18.4892098083346,16.8244336013383,6.17559621456002));
#38065=CARTESIAN_POINT('Ctrl Pts',(-17.9999516535622,17.0026196231967,6.21077640735487));
#38066=CARTESIAN_POINT('Ctrl Pts',(-18.4771016880877,16.7555788545222,6.69153398968095));
#38067=CARTESIAN_POINT('Ctrl Pts',(-18.4963362162636,16.8498937457125,6.18062294324687));
#38068=CARTESIAN_POINT('Ctrl Pts',(-18.0032410966494,17.0117663114213,6.21258228557033));
#38069=CARTESIAN_POINT('Ctrl Pts',(-18.4812032176816,16.768003161379,6.69303654757409));
#38070=CARTESIAN_POINT('Ctrl Pts',(-18.4995813969772,16.8627446305905,6.18316016026802));
#38071=CARTESIAN_POINT('Ctrl Pts',(-18.0047791706222,17.0163999130041,6.21349712162379));
#38072=CARTESIAN_POINT('Ctrl Pts',(-18.4925821723103,16.8055904468549,6.69757219653477));
#38073=CARTESIAN_POINT('Ctrl Pts',(-18.5082993306589,16.9014403837458,6.19080006401661));
#38074=CARTESIAN_POINT('Ctrl Pts',(-18.0090462865719,17.030417917443,6.21626476912844));
#38075=CARTESIAN_POINT('Ctrl Pts',(-18.4988883625265,16.8308948943173,6.70061244451219));
#38076=CARTESIAN_POINT('Ctrl Pts',(-18.5127456724536,16.9273229004005,6.19591018385897));
#38077=CARTESIAN_POINT('Ctrl Pts',(-18.0114111023906,17.0398550445677,6.21812799020613));
#38078=CARTESIAN_POINT('Ctrl Pts',(-18.5089809331914,16.8819886542203,6.70672283022605));
#38079=CARTESIAN_POINT('Ctrl Pts',(-18.5189743166287,16.979189821447,6.20615053976939));
#38080=CARTESIAN_POINT('Ctrl Pts',(-18.0151958167961,17.0589100232433,6.22189011372466));
#38081=CARTESIAN_POINT('Ctrl Pts',(-18.5127673002267,16.9077779664103,6.70979297341625));
#38082=CARTESIAN_POINT('Ctrl Pts',(-18.5207667892184,17.0051710504343,6.21128014890083));
#38083=CARTESIAN_POINT('Ctrl Pts',(-18.0166157093195,17.0685278759537,6.22378901639444));
#38084=CARTESIAN_POINT('Ctrl Pts',(-18.51653149759,16.9468304737568,6.71441949514766));
#38085=CARTESIAN_POINT('Ctrl Pts',(-18.5214756795303,17.0442515895124,6.21899602293492));
#38086=CARTESIAN_POINT('Ctrl Pts',(-18.0180272756984,17.0830920314624,6.22666449334457));
#38087=CARTESIAN_POINT('Ctrl Pts',(-18.5174610536025,16.9598642331123,6.71595985693076));
#38088=CARTESIAN_POINT('Ctrl Pts',(-18.5213812087045,17.0572310011096,6.22155861565454));
#38089=CARTESIAN_POINT('Ctrl Pts',(-18.0183758583191,17.0879528012551,6.22762418039891));
#38090=CARTESIAN_POINT('Ctrl Pts',(-18.5186722537819,16.9858429775025,6.71902258829226));
#38091=CARTESIAN_POINT('Ctrl Pts',(-18.5205481857505,17.0830017716537,6.22664667288122));
#38092=CARTESIAN_POINT('Ctrl Pts',(-18.0188300652425,17.0976412129467,6.22953701389521));
#38093=CARTESIAN_POINT('Ctrl Pts',(-18.5189557766232,16.9988067822409,6.7205471885435));
#38094=CARTESIAN_POINT('Ctrl Pts',(-18.5198112791957,17.0958122032461,6.22917590299987));
#38095=CARTESIAN_POINT('Ctrl Pts',(-18.0189363807851,17.1024758738013,6.23049154612614));
#38096=CARTESIAN_POINT('Ctrl Pts',(-18.5187872011184,17.0634999017462,6.72813660661715));
#38097=CARTESIAN_POINT('Ctrl Pts',(-18.5145769287806,17.1593013447143,6.24171089431925));
#38098=CARTESIAN_POINT('Ctrl Pts',(-18.0188731754452,17.1266021766945,6.23525492755391));
#38099=CARTESIAN_POINT('Ctrl Pts',(-18.5136215290469,17.1148550403912,6.73410108134611));
#38100=CARTESIAN_POINT('Ctrl Pts',(-18.5054607669974,17.2090806073982,6.25153907298411));
#38101=CARTESIAN_POINT('Ctrl Pts',(-18.0169360523498,17.1457541379813,6.23903619885366));
#38102=CARTESIAN_POINT('Ctrl Pts',(-18.5008049385582,17.178543935026,6.74142244098528));
#38103=CARTESIAN_POINT('Ctrl Pts',(-18.4879750956344,17.2700726310465,6.26358104534826));
#38104=CARTESIAN_POINT('Ctrl Pts',(-18.0121298155278,17.1695056335805,6.24372558012852));
#38105=CARTESIAN_POINT('Ctrl Pts',(-18.4979208133035,17.1912562328885,6.74287997549926));
#38106=CARTESIAN_POINT('Ctrl Pts',(-18.4841868810595,17.2821639022754,6.26596828789697));
#38107=CARTESIAN_POINT('Ctrl Pts',(-18.0110482760138,17.1742464268863,6.24466157960121));
#38108=CARTESIAN_POINT('Ctrl Pts',(-18.4914973495927,17.2166287983916,6.74578145608233));
#38109=CARTESIAN_POINT('Ctrl Pts',(-18.4759981394833,17.3062060478485,6.27071505370745));
#38110=CARTESIAN_POINT('Ctrl Pts',(-18.0086394683647,17.1837085953516,6.24652974472097));
#38111=CARTESIAN_POINT('Ctrl Pts',(-18.4879753251126,17.2292171975606,6.74721717444261));
#38112=CARTESIAN_POINT('Ctrl Pts',(-18.4716211015665,17.3180893500614,6.27306123585199));
#38113=CARTESIAN_POINT('Ctrl Pts',(-18.0073187104683,17.1884031726981,6.24745661953651));
#38114=CARTESIAN_POINT('Ctrl Pts',(-18.4765353931923,17.2665465103297,6.75146357848355));
#38115=CARTESIAN_POINT('Ctrl Pts',(-18.4577271501903,17.3531629274733,6.27998599460963));
#38116=CARTESIAN_POINT('Ctrl Pts',(-18.0030287452838,17.2023243430448,6.25020514858282));
#38117=CARTESIAN_POINT('Ctrl Pts',(-18.4677297456344,17.2909162449736,6.75422091139731));
#38118=CARTESIAN_POINT('Ctrl Pts',(-18.4474068235007,17.3759132514684,6.28447770936899));
#38119=CARTESIAN_POINT('Ctrl Pts',(-17.9997266201643,17.2114124977806,6.25199947022725));
#38120=CARTESIAN_POINT('Ctrl Pts',(-18.4378487844442,17.3625079863937,6.76228026019661));
#38121=CARTESIAN_POINT('Ctrl Pts',(-18.4134691558281,17.4421491186173,6.29755500102144));
#38122=CARTESIAN_POINT('Ctrl Pts',(-17.9885212630024,17.2381110500616,6.25727070422638));
#38123=CARTESIAN_POINT('Ctrl Pts',(-18.413342249397,17.4082296127105,6.76737146292247));
#38124=CARTESIAN_POINT('Ctrl Pts',(-18.3868137642132,17.483931249389,6.30580426435083));
#38125=CARTESIAN_POINT('Ctrl Pts',(-17.979331323364,17.2551619032087,6.26063714282115));
#38126=CARTESIAN_POINT('Ctrl Pts',(-18.3693951615143,17.4736551525738,6.77458729194665));
#38127=CARTESIAN_POINT('Ctrl Pts',(-18.3405991802905,17.5430486220348,6.31747611462008));
#38128=CARTESIAN_POINT('Ctrl Pts',(-17.9628511456172,17.279560906992,6.26545436500358));
#38129=CARTESIAN_POINT('Ctrl Pts',(-18.3537632469114,17.4945975063259,6.77688492238546));
#38130=CARTESIAN_POINT('Ctrl Pts',(-18.3244286783927,17.5618163081471,6.32118151647404));
#38131=CARTESIAN_POINT('Ctrl Pts',(-17.9569891815114,17.2873709068913,6.26699633389272));
#38132=CARTESIAN_POINT('Ctrl Pts',(-18.3206591277799,17.5347184100098,6.78126667754031));
#38133=CARTESIAN_POINT('Ctrl Pts',(-18.2906282613387,17.5975559035035,6.32823777061752));
#38134=CARTESIAN_POINT('Ctrl Pts',(-17.9445751422903,17.3023331556006,6.26995040845338));
#38135=CARTESIAN_POINT('Ctrl Pts',(-18.3031766385638,17.5539118752031,6.78335243318941));
#38136=CARTESIAN_POINT('Ctrl Pts',(-18.2729880315817,17.6145513152006,6.33159326311853));
#38137=CARTESIAN_POINT('Ctrl Pts',(-17.9380192073362,17.3094909634119,6.27136361166745));
#38138=CARTESIAN_POINT('Ctrl Pts',(-18.2663596953146,17.590573120573,6.78731950209393));
#38139=CARTESIAN_POINT('Ctrl Pts',(-18.2362359266378,17.6468363652653,6.33796746842275));
#38140=CARTESIAN_POINT('Ctrl Pts',(-17.9242128511607,17.3231630449985,6.2740629618247));
#38141=CARTESIAN_POINT('Ctrl Pts',(-18.2470253297619,17.6080409781332,6.78920081264864));
#38142=CARTESIAN_POINT('Ctrl Pts',(-18.2171237375768,17.6621351487866,6.3409879868012));
#38143=CARTESIAN_POINT('Ctrl Pts',(-17.9169624698265,17.3296773557345,6.27534911606522));
#38144=CARTESIAN_POINT('Ctrl Pts',(-18.2166010903152,17.6329170950227,6.79186951328928));
#38145=CARTESIAN_POINT('Ctrl Pts',(-18.1872989485619,17.683828532514,6.34527102434781));
#38146=CARTESIAN_POINT('Ctrl Pts',(-17.9055533732547,17.3389544402554,6.27718073909949));
#38147=CARTESIAN_POINT('Ctrl Pts',(-18.2062168750825,17.6409916724233,6.79273390499216));
#38148=CARTESIAN_POINT('Ctrl Pts',(-18.1771687996823,17.6908479022576,6.34665689501433));
#38149=CARTESIAN_POINT('Ctrl Pts',(-17.9016592934025,17.3419657104848,6.27777526983833));
#38150=CARTESIAN_POINT('Ctrl Pts',(-18.1849835178449,17.656672005178,6.79440927725295));
#38151=CARTESIAN_POINT('Ctrl Pts',(-18.1565384222284,17.7044471017748,6.34934185568567));
#38152=CARTESIAN_POINT('Ctrl Pts',(-17.8936967872377,17.3478134207786,6.27892981368751));
#38153=CARTESIAN_POINT('Ctrl Pts',(-18.1742117514745,17.6642209160496,6.79521418404731));
#38154=CARTESIAN_POINT('Ctrl Pts',(-18.1461128939455,17.7109787537895,6.35063143370503));
#38155=CARTESIAN_POINT('Ctrl Pts',(-17.8896573717566,17.3506286544074,6.27948563990098));
#38156=CARTESIAN_POINT('Ctrl Pts',(-18.1196129973381,17.7005236924937,6.7990781174034));
#38157=CARTESIAN_POINT('Ctrl Pts',(-18.0935526247991,17.7422665507531,6.35680874614416));
#38158=CARTESIAN_POINT('Ctrl Pts',(-17.8691828474184,17.3641671857882,6.2821586225467));
#38159=CARTESIAN_POINT('Ctrl Pts',(-18.073566038191,17.7250092175285,6.8016618385873));
#38160=CARTESIAN_POINT('Ctrl Pts',(-18.0497217046225,17.7632251779753,6.36094671689349));
#38161=CARTESIAN_POINT('Ctrl Pts',(-17.8519152345038,17.3732987063331,6.2839615061283));
#38162=CARTESIAN_POINT('Ctrl Pts',(-18.0130701585827,17.7499642230801,6.80428434438707));
#38163=CARTESIAN_POINT('Ctrl Pts',(-17.9926453915806,17.7844819967742,6.36514356115633));
#38164=CARTESIAN_POINT('Ctrl Pts',(-17.8292292752308,17.3826053354479,6.28579896230536));
#38165=CARTESIAN_POINT('Ctrl Pts',(-18.0008227990897,17.7546700742571,6.80477818859267));
#38166=CARTESIAN_POINT('Ctrl Pts',(-17.9811297306172,17.7884796711135,6.36593284278751));
#38167=CARTESIAN_POINT('Ctrl Pts',(-17.8246365175473,17.3843603279786,6.28614545960597));
#38168=CARTESIAN_POINT('Ctrl Pts',(-17.9760268452319,17.7635021372388,6.80570402970065));
#38169=CARTESIAN_POINT('Ctrl Pts',(-17.9578627436139,17.7959726092415,6.36741221252255));
#38170=CARTESIAN_POINT('Ctrl Pts',(-17.8153380323659,17.3876541288755,6.28679577184356));
#38171=CARTESIAN_POINT('Ctrl Pts',(-17.9634548231814,17.7676353220123,6.80613675524105));
#38172=CARTESIAN_POINT('Ctrl Pts',(-17.9460886325703,17.7994744891973,6.36810360689066));
#38173=CARTESIAN_POINT('Ctrl Pts',(-17.8106235240595,17.3891955494437,6.28710010252115));
#38174=CARTESIAN_POINT('Ctrl Pts',(-17.9254344120959,17.7790973746866,6.80733565050496));
#38175=CARTESIAN_POINT('Ctrl Pts',(-17.9105547741728,17.8091716890774,6.37001817548471));
#38176=CARTESIAN_POINT('Ctrl Pts',(-17.7963658737417,17.3934701994542,6.28794406889925));
#38177=CARTESIAN_POINT('Ctrl Pts',(-17.8999087430931,17.7854283478246,6.80799626184293));
#38178=CARTESIAN_POINT('Ctrl Pts',(-17.886766663715,17.8145173455381,6.37107359623513));
#38179=CARTESIAN_POINT('Ctrl Pts',(-17.7867937446671,17.3958312544259,6.28841022425892));
#38180=CARTESIAN_POINT('Ctrl Pts',(-17.8228126864582,17.8006160211639,6.80957942969772));
#38181=CARTESIAN_POINT('Ctrl Pts',(-17.8151219476809,17.8273163816643,6.37360057648762));
#38182=CARTESIAN_POINT('Ctrl Pts',(-17.7578827253461,17.4014953443393,6.28952851498163));
#38183=CARTESIAN_POINT('Ctrl Pts',(-17.7707282072719,17.8057036316249,6.81010758629701));
#38184=CARTESIAN_POINT('Ctrl Pts',(-17.7668735570122,17.8315930628393,6.37444494388912));
#38185=CARTESIAN_POINT('Ctrl Pts',(-17.7383510443547,17.4033927296949,6.28990312563806));
#38186=CARTESIAN_POINT('Ctrl Pts',(-17.7113425373793,17.8056309224566,6.81010002580354));
#38187=CARTESIAN_POINT('Ctrl Pts',(-17.7119066821582,17.8315319119423,6.37443287054956));
#38188=CARTESIAN_POINT('Ctrl Pts',(-17.7160814181658,17.4033655966885,6.28989776862753));
#38189=CARTESIAN_POINT('Ctrl Pts',(-17.7047330456674,17.8055415663399,6.81009073748399));
#38190=CARTESIAN_POINT('Ctrl Pts',(-17.7057888706203,17.8314568157848,6.37441804392472));
#38191=CARTESIAN_POINT('Ctrl Pts',(-17.7136028587132,17.4033322762928,6.28989119000853));
#38192=CARTESIAN_POINT('Ctrl Pts',(-17.6914916361947,17.8051984797874,6.81005506963536));
#38193=CARTESIAN_POINT('Ctrl Pts',(-17.6935317272033,17.8311684204133,6.37436110452697));
#38194=CARTESIAN_POINT('Ctrl Pts',(-17.7086373302776,17.4032043210795,6.28986592714545));
#38195=CARTESIAN_POINT('Ctrl Pts',(-17.6848569462331,17.8049443436771,6.81002864903746));
#38196=CARTESIAN_POINT('Ctrl Pts',(-17.6873896796574,17.8309547927005,6.37431892689686));
#38197=CARTESIAN_POINT('Ctrl Pts',(-17.7061493215936,17.4031095435898,6.28984721473285));
#38198=CARTESIAN_POINT('Ctrl Pts',(-17.6650316986901,17.8039394480878,6.80992416632294));
#38199=CARTESIAN_POINT('Ctrl Pts',(-17.669033565516,17.8301099792034,6.37415213097543));
#38200=CARTESIAN_POINT('Ctrl Pts',(-17.6987148534351,17.402734784112,6.28977322402055));
#38201=CARTESIAN_POINT('Ctrl Pts',(-17.65188297285,17.8029458235526,6.80982084423287));
#38202=CARTESIAN_POINT('Ctrl Pts',(-17.6568553794863,17.8292744610696,6.37398717028588));
#38203=CARTESIAN_POINT('Ctrl Pts',(-17.6937840817574,17.4023642144883,6.28970006053293));
#38204=CARTESIAN_POINT('Ctrl Pts',(-17.6126371335032,17.7990126660086,6.80941167670247));
#38205=CARTESIAN_POINT('Ctrl Pts',(-17.6204837103719,17.825965596934,6.37333388403476));
#38206=CARTESIAN_POINT('Ctrl Pts',(-17.6790668911251,17.4008973914905,6.28941045804156));
#38207=CARTESIAN_POINT('Ctrl Pts',(-17.5867398984557,17.7951231176127,6.80900689352775));
#38208=CARTESIAN_POINT('Ctrl Pts',(-17.596453210412,17.8226910680451,6.37268737676991));
#38209=CARTESIAN_POINT('Ctrl Pts',(-17.6693554286528,17.3994468177432,6.28912406372419));
#38210=CARTESIAN_POINT('Ctrl Pts',(-17.5354697949089,17.7848516081068,6.80793609188225));
#38211=CARTESIAN_POINT('Ctrl Pts',(-17.5487818608033,17.8140306147149,6.37097749843788));
#38212=CARTESIAN_POINT('Ctrl Pts',(-17.6501291396514,17.3956161693061,6.28836775888534));
#38213=CARTESIAN_POINT('Ctrl Pts',(-17.5100969352081,17.7784696191355,6.80727007507948));
#38214=CARTESIAN_POINT('Ctrl Pts',(-17.5251318472474,17.8086411999732,6.36991343826254));
#38215=CARTESIAN_POINT('Ctrl Pts',(-17.6406143159052,17.3932360814621,6.28789784576675));
#38216=CARTESIAN_POINT('Ctrl Pts',(-17.4724356982661,17.7670045961486,6.80607073498154));
#38217=CARTESIAN_POINT('Ctrl Pts',(-17.4899271035391,17.7989402787506,6.36799813494449));
#38218=CARTESIAN_POINT('Ctrl Pts',(-17.6264913542181,17.3889603296644,6.28705366185705));
#38219=CARTESIAN_POINT('Ctrl Pts',(-17.4599484159706,17.7628670210704,6.80563750504227));
#38220=CARTESIAN_POINT('Ctrl Pts',(-17.4782302202683,17.7954342534171,6.36730592213287));
#38221=CARTESIAN_POINT('Ctrl Pts',(-17.6218086213275,17.3874172771144,6.28674900896883));
#38222=CARTESIAN_POINT('Ctrl Pts',(-17.4351090516651,17.7539492007634,6.8047025599668));
#38223=CARTESIAN_POINT('Ctrl Pts',(-17.454917776984,17.7878675018479,6.36581197902636));
#38224=CARTESIAN_POINT('Ctrl Pts',(-17.6124938623285,17.384091480323,6.28609237961543));
#38225=CARTESIAN_POINT('Ctrl Pts',(-17.4227335316578,17.7491576061505,6.804199652638));
#38226=CARTESIAN_POINT('Ctrl Pts',(-17.4432789672747,17.7837963825994,6.36500819678485));
#38227=CARTESIAN_POINT('Ctrl Pts',(-17.6078530426073,17.38230451645,6.28573957004644));
#38228=CARTESIAN_POINT('Ctrl Pts',(-17.3618547466598,17.7238403969658,6.8015386718093));
#38229=CARTESIAN_POINT('Ctrl Pts',(-17.3858250678238,17.7622268875734,6.36074961922872));
#38230=CARTESIAN_POINT('Ctrl Pts',(-17.5850234902864,17.3728628177143,6.28387544637182));
#38231=CARTESIAN_POINT('Ctrl Pts',(-17.3158627238175,17.6991343295047,6.79893094285691));
#38232=CARTESIAN_POINT('Ctrl Pts',(-17.3420267744581,17.7410737731548,6.35657324986094));
#38233=CARTESIAN_POINT('Ctrl Pts',(-17.5677764852266,17.3636490384775,6.28205632202897));
#38234=CARTESIAN_POINT('Ctrl Pts',(-17.2508193911024,17.6555966201116,6.7942958684358));
#38235=CARTESIAN_POINT('Ctrl Pts',(-17.2793471455071,17.7035182827478,6.34915847411566));
#38236=CARTESIAN_POINT('Ctrl Pts',(-17.5433852397352,17.3474123674201,6.27885063163761));
#38237=CARTESIAN_POINT('Ctrl Pts',(-17.2298005184759,17.6399964301089,6.79262936990691));
#38238=CARTESIAN_POINT('Ctrl Pts',(-17.2589173832124,17.6899870750125,6.34648693741537));
#38239=CARTESIAN_POINT('Ctrl Pts',(-17.5355031559793,17.3415945569023,6.27770199105668));
#38240=CARTESIAN_POINT('Ctrl Pts',(-17.204378613571,17.619097401045,6.79038682430432));
#38241=CARTESIAN_POINT('Ctrl Pts',(-17.2340263963876,17.6717874399427,6.34289368883238));
#38242=CARTESIAN_POINT('Ctrl Pts',(-17.5259699480092,17.3338006396197,6.27616319744218));
#38243=CARTESIAN_POINT('Ctrl Pts',(-17.1993309492766,17.6148421450605,6.78992974985876));
#38244=CARTESIAN_POINT('Ctrl Pts',(-17.2290682897225,17.6680734413416,6.34216041477718));
#38245=CARTESIAN_POINT('Ctrl Pts',(-17.5240770741103,17.3322137206402,6.27584988377669));
#38246=CARTESIAN_POINT('Ctrl Pts',(-17.1893716918988,17.6062334486389,6.78900404892269));
#38247=CARTESIAN_POINT('Ctrl Pts',(-17.2192636543449,17.6605500551435,6.34067503352136));
#38248=CARTESIAN_POINT('Ctrl Pts',(-17.5203423496229,17.3290032721058,6.27521602822943));
#38249=CARTESIAN_POINT('Ctrl Pts',(-17.1844557566987,17.6018767026284,6.78853506940883));
#38250=CARTESIAN_POINT('Ctrl Pts',(-17.2144128912708,17.6567376554324,6.33992233162338));
#38251=CARTESIAN_POINT('Ctrl Pts',(-17.5184988766973,17.3273785031339,6.27489524164313));
#38252=CARTESIAN_POINT('Ctrl Pts',(-17.169896855944,17.5886510409319,6.78710983089398));
#38253=CARTESIAN_POINT('Ctrl Pts',(-17.2000081285538,17.6451450983018,6.33763355279219));
#38254=CARTESIAN_POINT('Ctrl Pts',(-17.5130392850471,17.3224462500153,6.27392144126411));
#38255=CARTESIAN_POINT('Ctrl Pts',(-17.1604426857215,17.5796268087842,6.78613528430944));
#38256=CARTESIAN_POINT('Ctrl Pts',(-17.1906117770433,17.6372170607117,6.33606827910802));
#38257=CARTESIAN_POINT('Ctrl Pts',(-17.5094939755331,17.3190808343234,6.27325698974518));
#38258=CARTESIAN_POINT('Ctrl Pts',(-17.1144092624932,17.5334875838914,6.78114111890133));
#38259=CARTESIAN_POINT('Ctrl Pts',(-17.1445255959529,17.5964801911601,6.32802538713625));
#38260=CARTESIAN_POINT('Ctrl Pts',(-17.4922314331161,17.3018741366695,6.26985978195909));
#38261=CARTESIAN_POINT('Ctrl Pts',(-17.0815070486393,17.4933474524288,6.77676052830464));
#38262=CARTESIAN_POINT('Ctrl Pts',(-17.1109009441881,17.5607248183131,6.32096601796079));
#38263=CARTESIAN_POINT('Ctrl Pts',(-17.4798931004167,17.2869047271829,6.26690429360894));
#38264=CARTESIAN_POINT('Ctrl Pts',(-17.0453050933139,17.4391198002594,6.77077798629523));
#38265=CARTESIAN_POINT('Ctrl Pts',(-17.0729618602987,17.5119192000139,6.31133007096938));
#38266=CARTESIAN_POINT('Ctrl Pts',(-17.4663173790063,17.2666817095338,6.26291155808251));
#38267=CARTESIAN_POINT('Ctrl Pts',(-17.0383132060228,17.4280698300166,6.76955593094628));
#38268=CARTESIAN_POINT('Ctrl Pts',(-17.065556626733,17.5019159878677,6.30935508478244));
#38269=CARTESIAN_POINT('Ctrl Pts',(-17.4636954152817,17.2625608716606,6.2620979596344));
#38270=CARTESIAN_POINT('Ctrl Pts',(-17.0248360913008,17.4055530530904,6.76705920363801));
#38271=CARTESIAN_POINT('Ctrl Pts',(-17.0511605700457,17.4814635711966,6.30531705781432));
#38272=CARTESIAN_POINT('Ctrl Pts',(-17.4586415045071,17.2541637364834,6.26044006957447));
#38273=CARTESIAN_POINT('Ctrl Pts',(-17.018385745669,17.3941425328792,6.76579076471037));
#38274=CARTESIAN_POINT('Ctrl Pts',(-17.044207273457,17.4710642956499,6.30326387477087));
#38275=CARTESIAN_POINT('Ctrl Pts',(-17.4562226243632,17.2499084384684,6.25959992396146));
#38276=CARTESIAN_POINT('Ctrl Pts',(-16.9999748915757,17.3596229038005,6.76194338591157));
#38277=CARTESIAN_POINT('Ctrl Pts',(-17.0241507155953,17.4394666729185,6.29702539181943));
#38278=CARTESIAN_POINT('Ctrl Pts',(-17.449318544805,17.237035119937,6.25705827774745));
#38279=CARTESIAN_POINT('Ctrl Pts',(-16.9889119861745,17.3361594967524,6.75931504519851));
#38280=CARTESIAN_POINT('Ctrl Pts',(-17.0118468913603,17.4178612762011,6.29275972600569));
#38281=CARTESIAN_POINT('Ctrl Pts',(-17.4451699630122,17.2282849645212,6.25533068906623));
#38282=CARTESIAN_POINT('Ctrl Pts',(-16.969151536231,17.2883531218114,6.75393133468145));
#38283=CARTESIAN_POINT('Ctrl Pts',(-16.9893185039968,17.3735255531602,6.28400629367688));
#38284=CARTESIAN_POINT('Ctrl Pts',(-17.4377597911824,17.2104566385494,6.25181074996914));
#38285=CARTESIAN_POINT('Ctrl Pts',(-16.9604540998271,17.2640101175317,6.75117596780138));
#38286=CARTESIAN_POINT('Ctrl Pts',(-16.979100694343,17.3507885344851,6.27951720585606));
#38287=CARTESIAN_POINT('Ctrl Pts',(-17.4344982506951,17.2013784496697,6.25001839593549));
#38288=CARTESIAN_POINT('Ctrl Pts',(-16.9454368141968,17.2144400485736,6.74553518479638));
#38289=CARTESIAN_POINT('Ctrl Pts',(-16.9607944578447,17.3041453864073,6.27030820660447));
#38290=CARTESIAN_POINT('Ctrl Pts',(-17.4288667753564,17.1828923505283,6.24636858926135));
#38291=CARTESIAN_POINT('Ctrl Pts',(-16.9391152612491,17.1892056047591,6.74264892813991));
#38292=CARTESIAN_POINT('Ctrl Pts',(-16.9527111071462,17.2802251876746,6.26558551739275));
#38293=CARTESIAN_POINT('Ctrl Pts',(-17.4264961901478,17.173481691707,6.24451059395842));
#38294=CARTESIAN_POINT('Ctrl Pts',(-16.9340264307573,17.163528852123,6.73969634090002));
#38295=CARTESIAN_POINT('Ctrl Pts',(-16.9457712867961,17.2557485214382,6.26075296190838));
#38296=CARTESIAN_POINT('Ctrl Pts',(-17.4245878781802,17.16390605946,6.24262002709426));
#38297=CARTESIAN_POINT('',(-18.0133068931633,17.0493818775139,6.22000892237058));
#38298=CARTESIAN_POINT('Origin',(-18.0133034595933,16.9525344893951,6.71053984230837));
#38299=CARTESIAN_POINT('',(-17.424587878778,17.1639060593454,6.24262002707162));
#38300=CARTESIAN_POINT('Ctrl Pts',(-17.4245878781802,17.16390605946,6.24262002709426));
#38301=CARTESIAN_POINT('Ctrl Pts',(-17.4239963526266,17.1609378701589,6.24203400204708));
#38302=CARTESIAN_POINT('Ctrl Pts',(-17.423450686133,17.1579624057897,6.24144654064541));
#38303=CARTESIAN_POINT('Ctrl Pts',(-17.4229521590767,17.1549871578456,6.24085912197364));
#38304=CARTESIAN_POINT('Ctrl Pts',(-17.4217671914954,17.1479151798734,6.23946286459101));
#38305=CARTESIAN_POINT('Ctrl Pts',(-17.4208459359997,17.140831572302,6.23806431111613));
#38306=CARTESIAN_POINT('Ctrl Pts',(-17.4201854095159,17.1337362792114,6.23666345050844));
#38307=CARTESIAN_POINT('Ctrl Pts',(-17.4193357250156,17.1246090743057,6.23486141898593));
#38308=CARTESIAN_POINT('Ctrl Pts',(-17.418917461125,17.115461497848,6.23305536540196));
#38309=CARTESIAN_POINT('Ctrl Pts',(-17.4189248391062,17.1062963840515,6.23124584933002));
#38310=CARTESIAN_POINT('Ctrl Pts',(-17.4189325800007,17.0966804501252,6.22934732549576));
#38311=CARTESIAN_POINT('Ctrl Pts',(-17.4194120469241,17.0870438617571,6.22744472374767));
#38312=CARTESIAN_POINT('Ctrl Pts',(-17.4203763301195,17.0773875052259,6.22553821906834));
#38313=CARTESIAN_POINT('Ctrl Pts',(-17.4204307036815,17.0768430069889,6.22543071595024));
#38314=CARTESIAN_POINT('Ctrl Pts',(-17.4204866297116,17.0762983905452,6.22532318949395));
#38315=CARTESIAN_POINT('Ctrl Pts',(-17.42054410957,17.0757536753193,6.22521564353459));
#38316=CARTESIAN_POINT('Ctrl Pts',(-17.4209972115288,17.0714597966854,6.22436788074937));
#38317=CARTESIAN_POINT('Ctrl Pts',(-17.4215449020002,17.0671774008785,6.2235223850784));
#38318=CARTESIAN_POINT('Ctrl Pts',(-17.4221870883531,17.0629071178979,6.22267928090569));
#38319=CARTESIAN_POINT('Ctrl Pts',(-17.4222707183068,17.0623510120782,6.22256948604217));
#38320=CARTESIAN_POINT('Ctrl Pts',(-17.4223558880511,17.0617955245123,6.2224598132437));
#38321=CARTESIAN_POINT('Ctrl Pts',(-17.4224425947226,17.0612406342997,6.22235025838381));
#38322=CARTESIAN_POINT('Ctrl Pts',(-17.42310851407,17.0569789999625,6.22150886175776));
#38323=CARTESIAN_POINT('Ctrl Pts',(-17.4238662074175,17.0527464735124,6.2206732120532));
#38324=CARTESIAN_POINT('Ctrl Pts',(-17.4247139972883,17.0485425419806,6.21984320799205));
#38325=CARTESIAN_POINT('Ctrl Pts',(-17.4248242481398,17.0479958416164,6.2197352700965));
#38326=CARTESIAN_POINT('Ctrl Pts',(-17.4249360094247,17.0474496203497,6.21962742679168));
#38327=CARTESIAN_POINT('Ctrl Pts',(-17.4250492807261,17.0469038779886,6.21951967803966));
#38328=CARTESIAN_POINT('Ctrl Pts',(-17.4270178554423,17.0374192636091,6.21764708130632));
#38329=CARTESIAN_POINT('Ctrl Pts',(-17.4294421208925,17.0280792618812,6.21580303620074));
#38330=CARTESIAN_POINT('Ctrl Pts',(-17.4323202517924,17.0188829947148,6.21398736935701));
#38331=CARTESIAN_POINT('Ctrl Pts',(-17.4350337261126,17.0102128418741,6.21227557600019));
#38332=CARTESIAN_POINT('Ctrl Pts',(-17.4381502171147,17.0016706838313,6.21058905332191));
#38333=CARTESIAN_POINT('Ctrl Pts',(-17.4416688286559,16.9932560204131,6.20892770257016));
#38334=CARTESIAN_POINT('Ctrl Pts',(-17.4418823418398,16.992745409464,6.2088268899955));
#38335=CARTESIAN_POINT('Ctrl Pts',(-17.4420973488182,16.9922352722248,6.20872617094784));
#38336=CARTESIAN_POINT('Ctrl Pts',(-17.4423138525004,16.9917256096056,6.20862554560688));
#38337=CARTESIAN_POINT('Ctrl Pts',(-17.4439898422823,16.9877802294007,6.20784658867852));
#38338=CARTESIAN_POINT('Ctrl Pts',(-17.4457556853019,16.9838624646562,6.20707308401416));
#38339=CARTESIAN_POINT('Ctrl Pts',(-17.4476116630671,16.9799749316384,6.20630554815676));
#38340=CARTESIAN_POINT('Ctrl Pts',(-17.4478510911231,16.9794734253754,6.20620653316761));
#38341=CARTESIAN_POINT('Ctrl Pts',(-17.4480920630631,16.9789723398839,6.20610760125357));
#38342=CARTESIAN_POINT('Ctrl Pts',(-17.4483345640874,16.978471710916,6.20600875947336));
#38343=CARTESIAN_POINT('Ctrl Pts',(-17.4502147381132,16.974590203261,6.20524241323467));
#38344=CARTESIAN_POINT('Ctrl Pts',(-17.4521887529142,16.9707323959116,6.20448074627054));
#38345=CARTESIAN_POINT('Ctrl Pts',(-17.4542495612884,16.9669156327685,6.20372718287749));
#38346=CARTESIAN_POINT('Ctrl Pts',(-17.4545149485985,16.966424116664,6.20363014029728));
#38347=CARTESIAN_POINT('Ctrl Pts',(-17.4547816091611,16.9659335710049,6.20353328931717));
#38348=CARTESIAN_POINT('Ctrl Pts',(-17.4550495371491,16.9654439997817,6.20343663072499));
#38349=CARTESIAN_POINT('Ctrl Pts',(-17.4594793107355,16.9573496991847,6.20183853087085));
#38350=CARTESIAN_POINT('Ctrl Pts',(-17.4642582686348,16.9495167468061,6.20029203035437));
#38351=CARTESIAN_POINT('Ctrl Pts',(-17.4693759748133,16.9419372968202,6.19879558013341));
#38352=CARTESIAN_POINT('Ctrl Pts',(-17.4751109733341,16.9334436215403,6.19711862965902));
#38353=CARTESIAN_POINT('Ctrl Pts',(-17.4812683755285,16.9252660518675,6.19550408955828));
#38354=CARTESIAN_POINT('Ctrl Pts',(-17.4878532971521,16.9174083701159,6.1939527065931));
#38355=CARTESIAN_POINT('Ctrl Pts',(-17.4937314913045,16.9103940149625,6.19256782598321));
#38356=CARTESIAN_POINT('Ctrl Pts',(-17.4999501245273,16.9036348244842,6.19123332386186));
#38357=CARTESIAN_POINT('Ctrl Pts',(-17.5065131208216,16.8971331521054,6.1899496648779));
#38358=CARTESIAN_POINT('Ctrl Pts',(-17.5069065081345,16.8967434405603,6.1898727221012));
#38359=CARTESIAN_POINT('Ctrl Pts',(-17.5073011442382,16.8963546628821,6.18979596370271));
#38360=CARTESIAN_POINT('Ctrl Pts',(-17.5076970324673,16.8959668214413,6.18971939015042));
#38361=CARTESIAN_POINT('Ctrl Pts',(-17.5090515851221,16.8946398013009,6.18945738966409));
#38362=CARTESIAN_POINT('Ctrl Pts',(-17.5104207888425,16.8933237461276,6.18919755404825));
#38363=CARTESIAN_POINT('Ctrl Pts',(-17.5118047748885,16.8920187547148,6.18893990280817));
#38364=CARTESIAN_POINT('Ctrl Pts',(-17.5135932512801,16.8903323603036,6.18860694919096));
#38365=CARTESIAN_POINT('Ctrl Pts',(-17.5154090302819,16.8886621211746,6.18827718519512));
#38366=CARTESIAN_POINT('Ctrl Pts',(-17.5172419503642,16.8870175731272,6.1879524935231));
#38367=CARTESIAN_POINT('Ctrl Pts',(-17.5176558878116,16.8866461766722,6.18787916678986));
#38368=CARTESIAN_POINT('Ctrl Pts',(-17.5180706956164,16.8862760853643,6.18780609773861));
#38369=CARTESIAN_POINT('Ctrl Pts',(-17.5184863718957,16.8859072963858,6.18773328581301));
#38370=CARTESIAN_POINT('Ctrl Pts',(-17.5217519345969,16.8830100814304,6.18716127359994));
#38371=CARTESIAN_POINT('Ctrl Pts',(-17.5250710692817,16.8801931952623,6.18660512111705));
#38372=CARTESIAN_POINT('Ctrl Pts',(-17.5284428907987,16.8774553207796,6.18606456832203));
#38373=CARTESIAN_POINT('Ctrl Pts',(-17.5288714663989,16.8771073230598,6.18599586132275));
#38374=CARTESIAN_POINT('Ctrl Pts',(-17.5293008917546,16.8767605997055,6.18592740592809));
#38375=CARTESIAN_POINT('Ctrl Pts',(-17.5297311661369,16.876415149672,6.18585920193176));
#38376=CARTESIAN_POINT('Ctrl Pts',(-17.5369330750402,16.870633026045,6.18471760719924));
#38377=CARTESIAN_POINT('Ctrl Pts',(-17.5443727527964,16.8652074307487,6.18364640370889));
#38378=CARTESIAN_POINT('Ctrl Pts',(-17.5520464878964,16.8601328033148,6.18264449362848));
#38379=CARTESIAN_POINT('Ctrl Pts',(-17.5601786799816,16.8547549990883,6.18158272577751));
#38380=CARTESIAN_POINT('Ctrl Pts',(-17.5685737386504,16.8497713618965,6.18059878037371));
#38381=CARTESIAN_POINT('Ctrl Pts',(-17.5772348972466,16.8451867599133,6.17969361856599));
#38382=CARTESIAN_POINT('Ctrl Pts',(-17.5777203263771,16.8449298082215,6.17964288725742));
#38383=CARTESIAN_POINT('Ctrl Pts',(-17.5782065927925,16.8446741120996,6.17959240384255));
#38384=CARTESIAN_POINT('Ctrl Pts',(-17.5786936981234,16.8444196739979,6.17954216880515));
#38385=CARTESIAN_POINT('Ctrl Pts',(-17.582552127317,16.8424042343437,6.17914425007471));
#38386=CARTESIAN_POINT('Ctrl Pts',(-17.586463186836,16.8404677179035,6.17876191356478));
#38387=CARTESIAN_POINT('Ctrl Pts',(-17.5904276953827,16.8386113479185,6.17839540078621));
#38388=CARTESIAN_POINT('Ctrl Pts',(-17.5909274567178,16.8383773360778,6.17834919861174));
#38389=CARTESIAN_POINT('Ctrl Pts',(-17.5914280675634,16.8381445980764,6.17830324793798));
#38390=CARTESIAN_POINT('Ctrl Pts',(-17.5919295301886,16.8379131373121,6.17825754943576));
#38391=CARTESIAN_POINT('Ctrl Pts',(-17.5936681678983,16.8371106320145,6.17809910664215));
#38392=CARTESIAN_POINT('Ctrl Pts',(-17.5954170352532,16.8363234502043,6.17794368924433));
#38393=CARTESIAN_POINT('Ctrl Pts',(-17.5971762338363,16.8355517601033,6.1777913304552));
#38394=CARTESIAN_POINT('Ctrl Pts',(-17.5994428292503,16.8345574952939,6.17759502758407));
#38395=CARTESIAN_POINT('Ctrl Pts',(-17.6017284628056,16.8335882506517,6.17740366457469));
#38396=CARTESIAN_POINT('Ctrl Pts',(-17.6040187012687,16.8326501826568,6.17721845693285));
#38397=CARTESIAN_POINT('Ctrl Pts',(-17.6045306328368,16.8324404985443,6.17717705790824));
#38398=CARTESIAN_POINT('Ctrl Pts',(-17.6050429326839,16.8322322929262,6.17713595079046));
#38399=CARTESIAN_POINT('Ctrl Pts',(-17.6055556005716,16.8320255651881,6.17709513545823));
#38400=CARTESIAN_POINT('Ctrl Pts',(-17.6147282126709,16.8283268093328,6.17636487085756));
#38401=CARTESIAN_POINT('Ctrl Pts',(-17.6240182691166,16.8250999643395,6.17572777807219));
#38402=CARTESIAN_POINT('Ctrl Pts',(-17.6334245013524,16.8223376299444,6.17518239602947));
#38403=CARTESIAN_POINT('Ctrl Pts',(-17.6423072352983,16.8197290316356,6.17466736690166));
#38404=CARTESIAN_POINT('Ctrl Pts',(-17.6512948852706,16.8175343889948,6.17423406719378));
#38405=CARTESIAN_POINT('Ctrl Pts',(-17.6603835260784,16.815748176766,6.17388140602583));
#38406=CARTESIAN_POINT('Ctrl Pts',(-17.6700101964278,16.8138562243097,6.17350786801496));
#38407=CARTESIAN_POINT('Ctrl Pts',(-17.6797510047685,16.8124258453062,6.17322546085085));
#38408=CARTESIAN_POINT('Ctrl Pts',(-17.6896061275879,16.8114698645862,6.17303671660658));
#38409=CARTESIAN_POINT('Ctrl Pts',(-17.6901520189626,16.8114169112502,6.17302626175413));
#38410=CARTESIAN_POINT('Ctrl Pts',(-17.6906984201744,16.8113654130281,6.17301609419237));
#38411=CARTESIAN_POINT('Ctrl Pts',(-17.691245246391,16.81131537637,6.17300621519479));
#38412=CARTESIAN_POINT('Ctrl Pts',(-17.6956341166443,16.8109137782137,6.17292692558263));
#38413=CARTESIAN_POINT('Ctrl Pts',(-17.7000547883742,16.8106061648172,6.17286619187026));
#38414=CARTESIAN_POINT('Ctrl Pts',(-17.704458698247,16.8103961220267,6.17282472203));
#38415=CARTESIAN_POINT('Ctrl Pts',(-17.7050064698865,16.8103699962687,6.17281956388575));
#38416=CARTESIAN_POINT('Ctrl Pts',(-17.7055540701931,16.8103453624145,6.17281470029583));
#38417=CARTESIAN_POINT('Ctrl Pts',(-17.7061014900395,16.8103222168314,6.17281013054302));
#38418=CARTESIAN_POINT('Ctrl Pts',(-17.7105033630717,16.8101361002363,6.17277338457593));
#38419=CARTESIAN_POINT('Ctrl Pts',(-17.7148955099544,16.8100464048699,6.17275567555338));
#38420=CARTESIAN_POINT('Ctrl Pts',(-17.7192780851963,16.8100515461297,6.17275669061902));
#38421=CARTESIAN_POINT('Ctrl Pts',(-17.7198223171621,16.8100521845758,6.17275681667074));
#38422=CARTESIAN_POINT('Ctrl Pts',(-17.7203664028382,16.8100542724886,6.17275722889823));
#38423=CARTESIAN_POINT('Ctrl Pts',(-17.7209103422184,16.8100578098489,6.17275792729767));
#38424=CARTESIAN_POINT('Ctrl Pts',(-17.7307586592126,16.810121855673,6.17277057219769));
#38425=CARTESIAN_POINT('Ctrl Pts',(-17.740559079287,16.8106606220985,6.17287694365447));
#38426=CARTESIAN_POINT('Ctrl Pts',(-17.7503117673952,16.8116743046869,6.17307708027865));
#38427=CARTESIAN_POINT('Ctrl Pts',(-17.7595290142826,16.8126323341633,6.17326622901958));
#38428=CARTESIAN_POINT('Ctrl Pts',(-17.7687032606477,16.8140145017524,6.17353911755344));
#38429=CARTESIAN_POINT('Ctrl Pts',(-17.7778348290988,16.8158209130995,6.17389576673834));
#38430=CARTESIAN_POINT('Ctrl Pts',(-17.7783652931537,16.8159258497589,6.17391648492863));
#38431=CARTESIAN_POINT('Ctrl Pts',(-17.7788956118845,16.8160322309445,6.17393748831926));
#38432=CARTESIAN_POINT('Ctrl Pts',(-17.7794257850525,16.8161400596518,6.1739587775016));
#38433=CARTESIAN_POINT('Ctrl Pts',(-17.7837247873403,16.8170144076703,6.17413140457718));
#38434=CARTESIAN_POINT('Ctrl Pts',(-17.7880141653873,16.8179839070022,6.17432281787131));
#38435=CARTESIAN_POINT('Ctrl Pts',(-17.7922938185966,16.8190500973935,6.17453332138404));
#38436=CARTESIAN_POINT('Ctrl Pts',(-17.7928208008302,16.819181384525,6.17455924208506));
#38437=CARTESIAN_POINT('Ctrl Pts',(-17.793347671119,16.8193141584276,6.17458545632702));
#38438=CARTESIAN_POINT('Ctrl Pts',(-17.7938743549672,16.8194483975145,6.17461195984794));
#38439=CARTESIAN_POINT('Ctrl Pts',(-17.7981523653082,16.8205387597953,6.17482723574251));
#38440=CARTESIAN_POINT('Ctrl Pts',(-17.8024180418494,16.8217260125767,6.17506164123241));
#38441=CARTESIAN_POINT('Ctrl Pts',(-17.8066313677461,16.822998390726,6.17531285346629));
#38442=CARTESIAN_POINT('Ctrl Pts',(-17.8071493194822,16.8231548064621,6.17534373543837));
#38443=CARTESIAN_POINT('Ctrl Pts',(-17.8076666436156,16.8233125431413,6.17537487821111));
#38444=CARTESIAN_POINT('Ctrl Pts',(-17.8081833410617,16.8234715983733,6.17540628131259));
#38445=CARTESIAN_POINT('Ctrl Pts',(-17.8171078324416,16.8262188289972,6.17594868133921));
#38446=CARTESIAN_POINT('Ctrl Pts',(-17.8258454839216,16.829359850349,6.17656882951683));
#38447=CARTESIAN_POINT('Ctrl Pts',(-17.8344010756028,16.8328846040527,6.17726473996791));
#38448=CARTESIAN_POINT('Ctrl Pts',(-17.8439443772991,16.8368162769577,6.17804099059274));
#38449=CARTESIAN_POINT('Ctrl Pts',(-17.8532627983433,16.8412219375003,6.17891082306143));
#38450=CARTESIAN_POINT('Ctrl Pts',(-17.8623523860865,16.8461099313546,6.17987588510378));
#38451=CARTESIAN_POINT('Ctrl Pts',(-17.8705041290683,16.8504935921676,6.18074137405146));
#38452=CARTESIAN_POINT('Ctrl Pts',(-17.8784700287685,16.8552640274904,6.18168322590168));
#38453=CARTESIAN_POINT('Ctrl Pts',(-17.8862519595826,16.8604302491132,6.18270321989906));
#38454=CARTESIAN_POINT('Ctrl Pts',(-17.8866982213105,16.8607265106765,6.18276171235995));
#38455=CARTESIAN_POINT('Ctrl Pts',(-17.8871438840282,16.8610241014696,6.1828204672576));
#38456=CARTESIAN_POINT('Ctrl Pts',(-17.8875888292958,16.8613229394795,6.18287946839972));
#38457=CARTESIAN_POINT('Ctrl Pts',(-17.8891949126272,16.8624016311327,6.18309244010161));
#38458=CARTESIAN_POINT('Ctrl Pts',(-17.8907913791061,16.8634963971031,6.18330858543951));
#38459=CARTESIAN_POINT('Ctrl Pts',(-17.8923726652077,16.8646033654539,6.18352713995682));
#38460=CARTESIAN_POINT('Ctrl Pts',(-17.8943923022893,16.8660171983633,6.18380628033951));
#38461=CARTESIAN_POINT('Ctrl Pts',(-17.8963900764334,16.867452833543,6.1840897252578));
#38462=CARTESIAN_POINT('Ctrl Pts',(-17.8983663167529,16.8689100738024,6.18437743577929));
#38463=CARTESIAN_POINT('Ctrl Pts',(-17.9023190460032,16.8718247376421,6.18495289301631));
#38464=CARTESIAN_POINT('Ctrl Pts',(-17.9061856528232,16.874825808707,6.1855454100811));
#38465=CARTESIAN_POINT('Ctrl Pts',(-17.9099681280811,16.8779123579719,6.18615480355134));
#38466=CARTESIAN_POINT('Ctrl Pts',(-17.9103771355834,16.8782461134415,6.18622069862909));
#38467=CARTESIAN_POINT('Ctrl Pts',(-17.9107851609273,16.8785808668023,6.1862867907257));
#38468=CARTESIAN_POINT('Ctrl Pts',(-17.9111922053572,16.8789166181642,6.18635307986288));
#38469=CARTESIAN_POINT('Ctrl Pts',(-17.9183132823679,16.8847904519018,6.18751278139937));
#38470=CARTESIAN_POINT('Ctrl Pts',(-17.9251329124577,16.8909686819571,6.18873258148364));
#38471=CARTESIAN_POINT('Ctrl Pts',(-17.9316538269046,16.8974481022438,6.19001184712136));
#38472=CARTESIAN_POINT('Ctrl Pts',(-17.9385476266958,16.9042980351151,6.19136426498516));
#38473=CARTESIAN_POINT('Ctrl Pts',(-17.9451075853853,16.9114845746872,6.19278314086014));
#38474=CARTESIAN_POINT('Ctrl Pts',(-17.9513273259246,16.9190136164559,6.19426963872467));
#38475=CARTESIAN_POINT('Ctrl Pts',(-17.9516615723884,16.9194182242641,6.19434952254805));
#38476=CARTESIAN_POINT('Ctrl Pts',(-17.9519948445867,16.919823836157,6.19442960461311));
#38477=CARTESIAN_POINT('Ctrl Pts',(-17.9523271371351,16.9202304499703,6.1945098844925));
#38478=CARTESIAN_POINT('Ctrl Pts',(-17.9550864843114,16.9236069586604,6.19517652615973));
#38479=CARTESIAN_POINT('Ctrl Pts',(-17.9577784017783,16.9270526915071,6.19585683511218));
#38480=CARTESIAN_POINT('Ctrl Pts',(-17.9604002187094,16.9305669206281,6.19655066764019));
#38481=CARTESIAN_POINT('Ctrl Pts',(-17.9607154832163,16.9309894946446,6.19663409862548));
#38482=CARTESIAN_POINT('Ctrl Pts',(-17.9610294892565,16.9314127309544,6.19671766037079));
#38483=CARTESIAN_POINT('Ctrl Pts',(-17.9613422375567,16.931836625018,6.19680135197987));
#38484=CARTESIAN_POINT('Ctrl Pts',(-17.963943627082,16.9353625069371,6.19749748518041));
#38485=CARTESIAN_POINT('Ctrl Pts',(-17.9664564881878,16.938932118167,6.19820225208616));
#38486=CARTESIAN_POINT('Ctrl Pts',(-17.9688822689746,16.9425440504763,6.19891537466263));
#38487=CARTESIAN_POINT('Ctrl Pts',(-17.9691734405987,16.9429775983889,6.19900097228131));
#38488=CARTESIAN_POINT('Ctrl Pts',(-17.9694633772217,16.9434117629754,6.1990866916531));
#38489=CARTESIAN_POINT('Ctrl Pts',(-17.9697520814202,16.9438465470988,6.19917253334329));
#38490=CARTESIAN_POINT('Ctrl Pts',(-17.9751399386372,16.9519605779618,6.2007745286464));
#38491=CARTESIAN_POINT('Ctrl Pts',(-17.9800962739498,16.9602865087157,6.20241836044683));
#38492=CARTESIAN_POINT('Ctrl Pts',(-17.9846245725303,16.9688229597914,6.204103756369));
#38493=CARTESIAN_POINT('Ctrl Pts',(-17.9889117260424,16.976904820022,6.20569940005691));
#38494=CARTESIAN_POINT('Ctrl Pts',(-17.9928153343569,16.9851749215112,6.20733220919538));
#38495=CARTESIAN_POINT('Ctrl Pts',(-17.9963377138694,16.9936323565903,6.20900200457843));
#38496=CARTESIAN_POINT('Ctrl Pts',(-17.9965358417055,16.9941080728797,6.20909592771898));
#38497=CARTESIAN_POINT('Ctrl Pts',(-17.9967327525697,16.9945843870955,6.20918996891125));
#38498=CARTESIAN_POINT('Ctrl Pts',(-17.996928444502,16.9950613002111,6.20928412834743));
#38499=CARTESIAN_POINT('Ctrl Pts',(-17.9985704225849,16.9990629004521,6.21007418508978));
#38500=CARTESIAN_POINT('Ctrl Pts',(-18.000127055299,17.003107344624,6.21087270073222));
#38501=CARTESIAN_POINT('Ctrl Pts',(-18.0015963946161,17.0071929605557,6.21167934512926));
#38502=CARTESIAN_POINT('Ctrl Pts',(-18.0017712541485,17.0076791715238,6.2117753402888));
#38503=CARTESIAN_POINT('Ctrl Pts',(-18.0019449012453,17.0081660427692,6.21187146581032));
#38504=CARTESIAN_POINT('Ctrl Pts',(-18.0021173239188,17.0086535449126,6.21196771589332));
#38505=CARTESIAN_POINT('Ctrl Pts',(-18.00356647107,17.0127508154623,6.2127766613222));
#38506=CARTESIAN_POINT('Ctrl Pts',(-18.004930376233,17.0168964776297,6.21359516095978));
#38507=CARTESIAN_POINT('Ctrl Pts',(-18.0062015761076,17.0210725713349,6.21441966885408));
#38508=CARTESIAN_POINT('Ctrl Pts',(-18.0063525764999,17.0215686316325,6.21451760861796));
#38509=CARTESIAN_POINT('Ctrl Pts',(-18.0065022211477,17.0220649394007,6.21461559724126));
#38510=CARTESIAN_POINT('Ctrl Pts',(-18.0066505099709,17.0225614895283,6.21471363371481));
#38511=CARTESIAN_POINT('Ctrl Pts',(-18.0092960000388,17.0314200022727,6.21646261594682));
#38512=CARTESIAN_POINT('Ctrl Pts',(-18.011514751731,17.0403601479657,6.21822771540715));
#38513=CARTESIAN_POINT('Ctrl Pts',(-18.0133068931633,17.0493818775115,6.22000892238259));
#38514=CARTESIAN_POINT('Origin',(-17.4245878781802,17.0670580149496,6.73315081743725));
#38515=CARTESIAN_POINT('Ctrl Pts',(-36.918942728626,17.5305480494939,-3.00047863991406));
#38516=CARTESIAN_POINT('Ctrl Pts',(-36.9184636408495,17.5305448701384,-2.5));
#38517=CARTESIAN_POINT('Ctrl Pts',(-37.418931489881,17.5338661095488,-2.5));
#38518=CARTESIAN_POINT('Ctrl Pts',(-36.918766523927,17.5567617326884,-2.99813492793641));
#38519=CARTESIAN_POINT('Ctrl Pts',(-36.9206303865991,17.5567282897711,-2.5));
#38520=CARTESIAN_POINT('Ctrl Pts',(-37.4188654127938,17.5438230235078,-2.5));
#38521=CARTESIAN_POINT('Ctrl Pts',(-36.9198840261816,17.5827769733229,-2.99578898700793));
#38522=CARTESIAN_POINT('Ctrl Pts',(-36.9240615386413,17.5825477668969,-2.5));
#38523=CARTESIAN_POINT('Ctrl Pts',(-37.4192844801969,17.5537061882809,-2.5));
#38524=CARTESIAN_POINT('Ctrl Pts',(-36.9246169309371,17.6343825999131,-2.99109602673912));
#38525=CARTESIAN_POINT('Ctrl Pts',(-36.9333093941054,17.6333273268776,-2.5));
#38526=CARTESIAN_POINT('Ctrl Pts',(-37.4210593120151,17.5733143538484,-2.5));
#38527=CARTESIAN_POINT('Ctrl Pts',(-36.9282325359345,17.6599800335755,-2.98874837352374));
#38528=CARTESIAN_POINT('Ctrl Pts',(-36.9391161778231,17.6582989890867,-2.5));
#38529=CARTESIAN_POINT('Ctrl Pts',(-37.4224151662337,17.5830420307807,-2.5));
#38530=CARTESIAN_POINT('Ctrl Pts',(-36.9379460863992,17.710766834452,-2.98405135826386));
#38531=CARTESIAN_POINT('Ctrl Pts',(-36.9530417639778,17.7074272412772,-2.5));
#38532=CARTESIAN_POINT('Ctrl Pts',(-37.4260577504339,17.6023455517275,-2.5));
#38533=CARTESIAN_POINT('Ctrl Pts',(-36.9440439356691,17.7359562130125,-2.98170199150478));
#38534=CARTESIAN_POINT('Ctrl Pts',(-36.961150208635,17.7315882072703,-2.5));
#38535=CARTESIAN_POINT('Ctrl Pts',(-37.4283444361295,17.6119214029654,-2.5));
#38536=CARTESIAN_POINT('Ctrl Pts',(-36.9550940181883,17.7734276473997,-2.97817796458518));
#38537=CARTESIAN_POINT('Ctrl Pts',(-36.9750602300798,17.7672721065816,-2.5));
#38538=CARTESIAN_POINT('Ctrl Pts',(-37.4324882266632,17.6261687598122,-2.5));
#38539=CARTESIAN_POINT('Ctrl Pts',(-36.9590977423692,17.7858733013829,-2.97700260220075));
#38540=CARTESIAN_POINT('Ctrl Pts',(-36.9799820522302,17.7790613692586,-2.5));
#38541=CARTESIAN_POINT('Ctrl Pts',(-37.4339896230655,17.6309012462933,-2.5));
#38542=CARTESIAN_POINT('Ctrl Pts',(-36.9677444087214,17.8106277669609,-2.97465510692309));
#38543=CARTESIAN_POINT('Ctrl Pts',(-36.9903966889781,17.8024136686443,-2.5));
#38544=CARTESIAN_POINT('Ctrl Pts',(-37.437232116886,17.6403150006157,-2.5));
#38545=CARTESIAN_POINT('Ctrl Pts',(-36.9723569013568,17.8228504435788,-2.97349114599914));
#38546=CARTESIAN_POINT('Ctrl Pts',(-36.9958519245572,17.8138964486576,-2.5));
#38547=CARTESIAN_POINT('Ctrl Pts',(-37.4389618074377,17.6449635078328,-2.5));
#38548=CARTESIAN_POINT('Ctrl Pts',(-36.9968316404772,17.8831937506765,-2.96772154502321));
#38549=CARTESIAN_POINT('Ctrl Pts',(-37.0242345246282,17.8701746208594,-2.5));
#38550=CARTESIAN_POINT('Ctrl Pts',(-37.4481398206947,17.6679151360551,-2.5));
#38551=CARTESIAN_POINT('Ctrl Pts',(-37.0208955392833,17.9290397288272,-2.96326313438592));
#38552=CARTESIAN_POINT('Ctrl Pts',(-37.0507916007085,17.9123870158746,-2.5));
#38553=CARTESIAN_POINT('Ctrl Pts',(-37.4571637864037,17.6853590086553,-2.5));
#38554=CARTESIAN_POINT('Ctrl Pts',(-37.0636620936595,17.9942014163556,-2.95683590040463));
#38555=CARTESIAN_POINT('Ctrl Pts',(-37.0962159645972,17.9716354404605,-2.5));
#38556=CARTESIAN_POINT('Ctrl Pts',(-37.4732012555054,17.7101600273524,-2.5));
#38557=CARTESIAN_POINT('Ctrl Pts',(-37.0790511866489,18.0153339916105,-2.95473552840589));
#38558=CARTESIAN_POINT('Ctrl Pts',(-37.1122588011471,17.9906733177174,-2.5));
#38559=CARTESIAN_POINT('Ctrl Pts',(-37.4789721679196,17.7182046074472,-2.5));
#38560=CARTESIAN_POINT('Ctrl Pts',(-37.1121011063091,18.0562700748877,-2.95063882870761));
#38561=CARTESIAN_POINT('Ctrl Pts',(-37.1461872334036,18.0272996809472,-2.5));
#38562=CARTESIAN_POINT('Ctrl Pts',(-37.4913658752322,17.733790264152,-2.5));
#38563=CARTESIAN_POINT('Ctrl Pts',(-37.1295103581676,18.0757653348942,-2.94867340342006));
#38564=CARTESIAN_POINT('Ctrl Pts',(-37.1638134804818,18.0446236356694,-2.5));
#38565=CARTESIAN_POINT('Ctrl Pts',(-37.4978943532022,17.7412139562433,-2.5));
#38566=CARTESIAN_POINT('Ctrl Pts',(-37.1843057553075,18.1314233942583,-2.94302770433399));
#38567=CARTESIAN_POINT('Ctrl Pts',(-37.2185148052678,18.0936922878623,-2.5));
#38568=CARTESIAN_POINT('Ctrl Pts',(-37.5184426204004,17.7624112761694,-2.5));
#38569=CARTESIAN_POINT('Ctrl Pts',(-37.2242361969918,18.1647864737446,-2.93959528754205));
#38570=CARTESIAN_POINT('Ctrl Pts',(-37.2575873678388,18.1227938260313,-2.5));
#38571=CARTESIAN_POINT('Ctrl Pts',(-37.5334165320212,17.7751217694643,-2.5));
#38572=CARTESIAN_POINT('Ctrl Pts',(-37.278501267837,18.2017080527822,-2.93576187067611));
#38573=CARTESIAN_POINT('Ctrl Pts',(-37.3098415222596,18.154743770369,-2.5));
#38574=CARTESIAN_POINT('Ctrl Pts',(-37.5537659442094,17.7891910078983,-2.5));
#38575=CARTESIAN_POINT('Ctrl Pts',(-37.2895908939828,18.2088614252754,-2.9350171685076));
#38576=CARTESIAN_POINT('Ctrl Pts',(-37.3204553852497,18.1609059986669,-2.5));
#38577=CARTESIAN_POINT('Ctrl Pts',(-37.5579245541323,17.7919170308987,-2.5));
#38578=CARTESIAN_POINT('Ctrl Pts',(-37.3121456740118,18.222628713375,-2.93358056573866));
#38579=CARTESIAN_POINT('Ctrl Pts',(-37.3419594345533,18.1727383129417,-2.5));
#38580=CARTESIAN_POINT('Ctrl Pts',(-37.5663825921581,17.7971638038772,-2.5));
#38581=CARTESIAN_POINT('Ctrl Pts',(-37.3235504689819,18.2292070024891,-2.93289238561845));
#38582=CARTESIAN_POINT('Ctrl Pts',(-37.3527929576584,18.1783789941509,-2.5));
#38583=CARTESIAN_POINT('Ctrl Pts',(-37.5706593939047,17.7996709619125,-2.5));
#38584=CARTESIAN_POINT('Ctrl Pts',(-37.3581397345302,18.2480437180578,-2.93091764257171));
#38585=CARTESIAN_POINT('Ctrl Pts',(-37.3855178350711,18.1944875128524,-2.5));
#38586=CARTESIAN_POINT('Ctrl Pts',(-37.5836303643146,17.8068505202015,-2.5));
#38587=CARTESIAN_POINT('Ctrl Pts',(-37.3816981781207,18.2594061256977,-2.92972067272748));
#38588=CARTESIAN_POINT('Ctrl Pts',(-37.4076765730136,18.2041692805068,-2.5));
#38589=CARTESIAN_POINT('Ctrl Pts',(-37.5924647836065,17.811181769741,-2.5));
#38590=CARTESIAN_POINT('Ctrl Pts',(-37.4297964715305,18.2797809159781,-2.92756741754469));
#38591=CARTESIAN_POINT('Ctrl Pts',(-37.4526661261266,18.2214705311287,-2.5));
#38592=CARTESIAN_POINT('Ctrl Pts',(-37.6105016433052,17.8189490809156,-2.5));
#38593=CARTESIAN_POINT('Ctrl Pts',(-37.4543363298823,18.2887932678948,-2.92661112217483));
#38594=CARTESIAN_POINT('Ctrl Pts',(-37.4755052012686,18.2290974806186,-2.5));
#38595=CARTESIAN_POINT('Ctrl Pts',(-37.6197040888717,17.8223851300001,-2.5));
#38596=CARTESIAN_POINT('Ctrl Pts',(-37.4918913116176,18.3005282374446,-2.92536297515959));
#38597=CARTESIAN_POINT('Ctrl Pts',(-37.5103223388011,18.2390056374751,-2.5));
#38598=CARTESIAN_POINT('Ctrl Pts',(-37.633787209243,17.8268594543971,-2.5));
#38599=CARTESIAN_POINT('Ctrl Pts',(-37.5045340558524,18.3041421023044,-2.92497802297482));
#38600=CARTESIAN_POINT('Ctrl Pts',(-37.5220166849113,18.2420518473036,-2.5));
#38601=CARTESIAN_POINT('Ctrl Pts',(-37.6385282366181,17.8282374131812,-2.5));
#38602=CARTESIAN_POINT('Ctrl Pts',(-37.5236880380742,18.3091085696021,-2.92444842107095));
#38603=CARTESIAN_POINT('Ctrl Pts',(-37.5397059345923,18.2462341178242,-2.5));
#38604=CARTESIAN_POINT('Ctrl Pts',(-37.6457109814105,17.8301311528227,-2.5));
#38605=CARTESIAN_POINT('Ctrl Pts',(-37.530104354971,18.310688300037,-2.92427986194296));
#38606=CARTESIAN_POINT('Ctrl Pts',(-37.5456258343898,18.2475634797771,-2.5));
#38607=CARTESIAN_POINT('Ctrl Pts',(-37.6481170992389,17.8307335274115,-2.5));
#38608=CARTESIAN_POINT('Ctrl Pts',(-37.5430010389201,18.3136945178689,-2.9239589307846));
#38609=CARTESIAN_POINT('Ctrl Pts',(-37.5575155990342,18.2500919427414,-2.5));
#38610=CARTESIAN_POINT('Ctrl Pts',(-37.6529533567628,17.8318798449285,-2.5));
#38611=CARTESIAN_POINT('Ctrl Pts',(-37.5494894557846,18.3151225191071,-2.92380639706833));
#38612=CARTESIAN_POINT('Ctrl Pts',(-37.5634930070409,18.2512923999885,-2.5));
#38613=CARTESIAN_POINT('Ctrl Pts',(-37.6553865130038,17.8324243739287,-2.5));
#38614=CARTESIAN_POINT('Ctrl Pts',(-37.6078715508142,18.3272151542962,-2.92251412976417));
#38615=CARTESIAN_POINT('Ctrl Pts',(-37.6171933811497,18.261444733944,-2.5));
#38616=CARTESIAN_POINT('Ctrl Pts',(-37.6772797946946,17.8370356375276,-2.5));
#38617=CARTESIAN_POINT('Ctrl Pts',(-37.6600314084477,18.3327140130362,-2.92192313396902));
#38618=CARTESIAN_POINT('Ctrl Pts',(-37.6650031743221,18.2660494018553,-2.5));
#38619=CARTESIAN_POINT('Ctrl Pts',(-37.6968397447769,17.8391327868468,-2.5));
#38620=CARTESIAN_POINT('Ctrl Pts',(-37.7386551922739,18.3333477986367,-2.92185513454714));
#38621=CARTESIAN_POINT('Ctrl Pts',(-37.7369884997638,18.2665799642824,-2.5));
#38622=CARTESIAN_POINT('Ctrl Pts',(-37.7263236637676,17.8393744833388,-2.5));
#38623=CARTESIAN_POINT('Ctrl Pts',(-37.7649275847458,18.332280602678,-2.92196969819476));
#38624=CARTESIAN_POINT('Ctrl Pts',(-37.7610453062294,18.2656866234871,-2.5));
#38625=CARTESIAN_POINT('Ctrl Pts',(-37.7361758116312,17.8389674969796,-2.5));
#38626=CARTESIAN_POINT('Ctrl Pts',(-37.8044355425913,18.3287092953001,-2.9223525645861));
#38627=CARTESIAN_POINT('Ctrl Pts',(-37.7972513234411,18.2626950729203,-2.5));
#38628=CARTESIAN_POINT('Ctrl Pts',(-37.7509912947654,17.8376055413245,-2.5));
#38629=CARTESIAN_POINT('Ctrl Pts',(-37.8176556209491,18.3271839572083,-2.92251604054704));
#38630=CARTESIAN_POINT('Ctrl Pts',(-37.8093757241164,18.2614166995762,-2.5));
#38631=CARTESIAN_POINT('Ctrl Pts',(-37.7559488239131,17.8370238468006,-2.5));
#38632=CARTESIAN_POINT('Ctrl Pts',(-37.8438653515097,18.3235000632348,-2.92291055095015));
#38633=CARTESIAN_POINT('Ctrl Pts',(-37.8334337540048,18.2583273875558,-2.5));
#38634=CARTESIAN_POINT('Ctrl Pts',(-37.7657774740514,17.8356190137894,-2.5));
#38635=CARTESIAN_POINT('Ctrl Pts',(-37.8568746743686,18.321341537448,-2.92314158144293));
#38636=CARTESIAN_POINT('Ctrl Pts',(-37.8453867146324,18.256516085823,-2.5));
#38637=CARTESIAN_POINT('Ctrl Pts',(-37.7706559690046,17.8347958710238,-2.5));
#38638=CARTESIAN_POINT('Ctrl Pts',(-37.9214525991908,18.3089956020391,-2.92446167772975));
#38639=CARTESIAN_POINT('Ctrl Pts',(-37.9048311581349,18.2461405986857,-2.5));
#38640=CARTESIAN_POINT('Ctrl Pts',(-37.7948726934621,17.8300879827949,-2.5));
#38641=CARTESIAN_POINT('Ctrl Pts',(-37.971628515283,18.2941930137726,-2.92604160841261));
#38642=CARTESIAN_POINT('Ctrl Pts',(-37.951260778169,18.233665691823,-2.5));
#38643=CARTESIAN_POINT('Ctrl Pts',(-37.8136886637651,17.8244435332827,-2.5));
#38644=CARTESIAN_POINT('Ctrl Pts',(-38.0324952429552,18.2695437413729,-2.9286496092432));
#38645=CARTESIAN_POINT('Ctrl Pts',(-38.0080199920834,18.2127861786537,-2.5));
#38646=CARTESIAN_POINT('Ctrl Pts',(-37.8365136817825,17.8150464189915,-2.5));
#38647=CARTESIAN_POINT('Ctrl Pts',(-38.044575088039,18.264303794869,-2.92920311231327));
#38648=CARTESIAN_POINT('Ctrl Pts',(-38.0193295823946,18.208334158798,-2.5));
#38649=CARTESIAN_POINT('Ctrl Pts',(-37.8410436263355,17.8130488679072,-2.5));
#38650=CARTESIAN_POINT('Ctrl Pts',(-38.0685444585904,18.2531925029883,-2.93037437162195));
#38651=CARTESIAN_POINT('Ctrl Pts',(-38.0418344218168,18.1988760473144,-2.5));
#38652=CARTESIAN_POINT('Ctrl Pts',(-37.850032136943,17.8088132624928,-2.5));
#38653=CARTESIAN_POINT('Ctrl Pts',(-38.0804306041699,18.2473200654554,-2.93099223718261));
#38654=CARTESIAN_POINT('Ctrl Pts',(-38.0530277696176,18.1938679552602,-2.5));
#38655=CARTESIAN_POINT('Ctrl Pts',(-37.8544894413598,17.8065748058377,-2.5));
#38656=CARTESIAN_POINT('Ctrl Pts',(-38.1154058739446,18.2289535054552,-2.93292028761117));
#38657=CARTESIAN_POINT('Ctrl Pts',(-38.0860884329982,18.1781636427194,-2.5));
#38658=CARTESIAN_POINT('Ctrl Pts',(-37.8676051730758,17.7995742349009,-2.5));
#38659=CARTESIAN_POINT('Ctrl Pts',(-38.1379498775984,18.2156512801827,-2.93431116406502));
#38660=CARTESIAN_POINT('Ctrl Pts',(-38.107532686332,18.1667488029368,-2.5));
#38661=CARTESIAN_POINT('Ctrl Pts',(-37.8760591693826,17.7945044510302,-2.5));
#38662=CARTESIAN_POINT('Ctrl Pts',(-38.2033280576451,18.17265741314,-2.93878236806526));
#38663=CARTESIAN_POINT('Ctrl Pts',(-38.1702794467489,18.1296291178422,-2.5));
#38664=CARTESIAN_POINT('Ctrl Pts',(-37.9005759909892,17.7781206666248,-2.5));
#38665=CARTESIAN_POINT('Ctrl Pts',(-38.2439301407294,18.1399084455847,-2.94215865140722));
#38666=CARTESIAN_POINT('Ctrl Pts',(-38.2098765411374,18.1011163150348,-2.5));
#38667=CARTESIAN_POINT('Ctrl Pts',(-37.9158017810326,17.7656435334912,-2.5));
#38668=CARTESIAN_POINT('Ctrl Pts',(-38.2908370693989,18.0936969886663,-2.94685549765066));
#38669=CARTESIAN_POINT('Ctrl Pts',(-38.2564928085569,18.0604885105553,-2.5));
#38670=CARTESIAN_POINT('Ctrl Pts',(-37.9333918647676,17.7480431201017,-2.5));
#38671=CARTESIAN_POINT('Ctrl Pts',(-38.2999735282245,18.0842373184233,-2.94781393656573));
#38672=CARTESIAN_POINT('Ctrl Pts',(-38.2656503724343,18.0521248196139,-2.5));
#38673=CARTESIAN_POINT('Ctrl Pts',(-37.9368180370691,17.744440511481,-2.5));
#38674=CARTESIAN_POINT('Ctrl Pts',(-38.3176873507553,18.0649722522993,-2.94975921175979));
#38675=CARTESIAN_POINT('Ctrl Pts',(-38.2835158468797,18.035036707545,-2.5));
#38676=CARTESIAN_POINT('Ctrl Pts',(-37.9434607258409,17.7371042069719,-2.5));
#38677=CARTESIAN_POINT('Ctrl Pts',(-38.3262776360071,18.0551541758763,-2.95074733976652));
#38678=CARTESIAN_POINT('Ctrl Pts',(-38.292236426,18.0262999067001,-2.5));
#38679=CARTESIAN_POINT('Ctrl Pts',(-37.9466820784148,17.7333656728621,-2.5));
#38680=CARTESIAN_POINT('Ctrl Pts',(-38.3512613834271,18.0251519219321,-2.95375629684687));
#38681=CARTESIAN_POINT('Ctrl Pts',(-38.3177954315766,17.9994877930366,-2.5));
#38682=CARTESIAN_POINT('Ctrl Pts',(-37.9560509888996,17.721942323421,-2.5));
#38683=CARTESIAN_POINT('Ctrl Pts',(-38.3668695803311,18.0044210131818,-2.95582157994119));
#38684=CARTESIAN_POINT('Ctrl Pts',(-38.3339844060987,17.9808535987548,-2.5));
#38685=CARTESIAN_POINT('Ctrl Pts',(-37.9619040598854,17.7140502257561,-2.5));
#38686=CARTESIAN_POINT('Ctrl Pts',(-38.3960122766866,17.96151412598,-2.96006384799544));
#38687=CARTESIAN_POINT('Ctrl Pts',(-38.3647032001448,17.9420087393569,-2.5));
#38688=CARTESIAN_POINT('Ctrl Pts',(-37.9728325697887,17.6977186737315,-2.5));
#38689=CARTESIAN_POINT('Ctrl Pts',(-38.4095468146066,17.9393381811376,-2.96224084544494));
#38690=CARTESIAN_POINT('Ctrl Pts',(-38.3792301089262,17.921787539762,-2.5));
#38691=CARTESIAN_POINT('Ctrl Pts',(-37.9779080274105,17.6892792325375,-2.5));
#38692=CARTESIAN_POINT('Ctrl Pts',(-38.4282645108262,17.904969535058,-2.96558787871309));
#38693=CARTESIAN_POINT('Ctrl Pts',(-38.399714653804,17.8902405113807,-2.5));
#38694=CARTESIAN_POINT('Ctrl Pts',(-37.9849271555627,17.6762019272695,-2.5));
#38695=CARTESIAN_POINT('Ctrl Pts',(-38.4342446366122,17.89331766282,-2.96671826104229));
#38696=CARTESIAN_POINT('Ctrl Pts',(-38.4063407380303,17.8794930259532,-2.5));
#38697=CARTESIAN_POINT('Ctrl Pts',(-37.9871697012262,17.6717687488141,-2.5));
#38698=CARTESIAN_POINT('Ctrl Pts',(-38.4456424175336,17.8696845533725,-2.96900170083772));
#38699=CARTESIAN_POINT('Ctrl Pts',(-38.4191252098151,17.8576079915772,-2.5));
#38700=CARTESIAN_POINT('Ctrl Pts',(-37.991443877371,17.6627778699454,-2.5));
#38701=CARTESIAN_POINT('Ctrl Pts',(-38.4510249910641,17.8577775263316,-2.9701475957582));
#38702=CARTESIAN_POINT('Ctrl Pts',(-38.4252432488303,17.8465380939854,-2.5));
#38703=CARTESIAN_POINT('Ctrl Pts',(-37.9934623353037,17.6582483931711,-2.5));
#38704=CARTESIAN_POINT('Ctrl Pts',(-38.4763900971177,17.7977995570222,-2.97589627219185));
#38705=CARTESIAN_POINT('Ctrl Pts',(-38.4545812226388,17.790369539723,-2.5));
#38706=CARTESIAN_POINT('Ctrl Pts',(-38.002974265032,17.6354345524181,-2.5));
#38707=CARTESIAN_POINT('Ctrl Pts',(-38.4917731732021,17.7484124059281,-2.98055544920644));
#38708=CARTESIAN_POINT('Ctrl Pts',(-38.473661265785,17.7435263663243,-2.5));
#38709=CARTESIAN_POINT('Ctrl Pts',(-38.0087429143111,17.6166554164039,-2.5));
#38710=CARTESIAN_POINT('Ctrl Pts',(-38.5049497227733,17.6849440597232,-2.9864412217583));
#38711=CARTESIAN_POINT('Ctrl Pts',(-38.4919775578133,17.6825071777955,-2.5));
#38712=CARTESIAN_POINT('Ctrl Pts',(-38.0136841107577,17.5925304537987,-2.5));
#38713=CARTESIAN_POINT('Ctrl Pts',(-38.5072797054594,17.6721629059777,-2.9876215411643));
#38714=CARTESIAN_POINT('Ctrl Pts',(-38.4953743016544,17.6701248728446,-2.5));
#38715=CARTESIAN_POINT('Ctrl Pts',(-38.0145578594488,17.5876726194739,-2.5));
#38716=CARTESIAN_POINT('Ctrl Pts',(-38.5113201026512,17.646423044551,-2.98998846097813));
#38717=CARTESIAN_POINT('Ctrl Pts',(-38.501596520551,17.645080935214,-2.5));
#38718=CARTESIAN_POINT('Ctrl Pts',(-38.0160730018852,17.5778902994518,-2.5));
#38719=CARTESIAN_POINT('Ctrl Pts',(-38.5130325575213,17.6334445126556,-2.99117686889631));
#38720=CARTESIAN_POINT('Ctrl Pts',(-38.5044245550668,17.6323990130624,-2.5));
#38721=CARTESIAN_POINT('Ctrl Pts',(-38.0167151730816,17.5729582831273,-2.5));
#38722=CARTESIAN_POINT('Ctrl Pts',(-38.5172060896891,17.5943721213219,-2.99473928414168));
#38723=CARTESIAN_POINT('Ctrl Pts',(-38.5120043473919,17.5940082770842,-2.5));
#38724=CARTESIAN_POINT('Ctrl Pts',(-38.0182802555498,17.5581115117232,-2.5));
#38725=CARTESIAN_POINT('Ctrl Pts',(-38.5186917422194,17.5683120165936,-2.99709499970835));
#38726=CARTESIAN_POINT('Ctrl Pts',(-38.5157988525533,17.5682102346573,-2.5));
#38727=CARTESIAN_POINT('Ctrl Pts',(-38.0188373699573,17.5482108332471,-2.5));
#38728=CARTESIAN_POINT('Ctrl Pts',(-38.5191072198307,17.5161686034308,-3.00176886678129));
#38729=CARTESIAN_POINT('Ctrl Pts',(-38.5208771553493,17.5161399120222,-2.5));
#38730=CARTESIAN_POINT('Ctrl Pts',(-38.0189931741039,17.5284038967669,-2.5));
#38731=CARTESIAN_POINT('Ctrl Pts',(-38.5180370412835,17.4900852974077,-3.00408701695548));
#38732=CARTESIAN_POINT('Ctrl Pts',(-38.5221491625175,17.4898665253747,-2.5));
#38733=CARTESIAN_POINT('Ctrl Pts',(-38.0185918623631,17.5184976387542,-2.5));
#38734=CARTESIAN_POINT('Ctrl Pts',(-38.5144871859473,17.4509429730902,-3.00753674366307));
#38735=CARTESIAN_POINT('Ctrl Pts',(-38.5220957984724,17.4501405073408,-2.5));
#38736=CARTESIAN_POINT('Ctrl Pts',(-38.0172606587587,17.5036340064431,-2.5));
#38737=CARTESIAN_POINT('Ctrl Pts',(-38.512979645677,17.4379142878159,-3.00868013835556));
#38738=CARTESIAN_POINT('Ctrl Pts',(-38.5217466988597,17.4368445410147,-2.5));
#38739=CARTESIAN_POINT('Ctrl Pts',(-38.0166953304505,17.4986869777819,-2.5));
#38740=CARTESIAN_POINT('Ctrl Pts',(-38.5093456409823,17.4120774324436,-3.01093824610606));
#38741=CARTESIAN_POINT('Ctrl Pts',(-38.5203938380985,17.4103637207151,-2.5));
#38742=CARTESIAN_POINT('Ctrl Pts',(-38.0153325853393,17.4888774005165,-2.5));
#38743=CARTESIAN_POINT('Ctrl Pts',(-38.5072169868592,17.3992427493601,-3.01205529745571));
#38744=CARTESIAN_POINT('Ctrl Pts',(-38.5193887795888,17.3971525411347,-2.5));
#38745=CARTESIAN_POINT('Ctrl Pts',(-38.014534334724,17.4840047859771,-2.5));
#38746=CARTESIAN_POINT('Ctrl Pts',(-38.4950383810716,17.335482072003,-3.01758225181016));
#38747=CARTESIAN_POINT('Ctrl Pts',(-38.512708363373,17.3310164313404,-2.5));
#38748=CARTESIAN_POINT('Ctrl Pts',(-38.0099673675257,17.4598001953765,-2.5));
#38749=CARTESIAN_POINT('Ctrl Pts',(-38.4804258988967,17.2857825382543,-3.02181836676292));
#38750=CARTESIAN_POINT('Ctrl Pts',(-38.5021474563194,17.2787657562271,-2.5));
#38751=CARTESIAN_POINT('Ctrl Pts',(-38.0044876905449,17.4409392110453,-2.5));
#38752=CARTESIAN_POINT('Ctrl Pts',(-38.4559979025521,17.2253187773268,-3.02689693274587));
#38753=CARTESIAN_POINT('Ctrl Pts',(-38.482188384964,17.2143685236006,-2.5));
#38754=CARTESIAN_POINT('Ctrl Pts',(-37.9953271771502,17.4179991279534,-2.5));
#38755=CARTESIAN_POINT('Ctrl Pts',(-38.4508014471794,17.2133098047403,-3.02790174447839));
#38756=CARTESIAN_POINT('Ctrl Pts',(-38.4778364738777,17.2014855815011,-2.5));
#38757=CARTESIAN_POINT('Ctrl Pts',(-37.9933785134793,17.4134431981463,-2.5));
#38758=CARTESIAN_POINT('Ctrl Pts',(-38.4425304868847,17.1954247892708,-3.02939268814916));
#38759=CARTESIAN_POINT('Ctrl Pts',(-38.4707770006933,17.1822327898589,-2.5));
#38760=CARTESIAN_POINT('Ctrl Pts',(-37.9902768971576,17.4066584740223,-2.5));
#38761=CARTESIAN_POINT('Ctrl Pts',(-38.4396936273783,17.1894842833032,-3.02988697260699));
#38762=CARTESIAN_POINT('Ctrl Pts',(-38.4683326604495,17.1758218953105,-2.5));
#38763=CARTESIAN_POINT('Ctrl Pts',(-37.9892130751568,17.4044050008767,-2.5));
#38764=CARTESIAN_POINT('Ctrl Pts',(-38.433892526343,17.1777122168892,-3.03086468827693));
#38765=CARTESIAN_POINT('Ctrl Pts',(-38.4632915541776,17.1630927437411,-2.5));
#38766=CARTESIAN_POINT('Ctrl Pts',(-37.9870376657812,17.3999395207739,-2.5));
#38767=CARTESIAN_POINT('Ctrl Pts',(-38.4309245022383,17.1718722889636,-3.03134881683581));
#38768=CARTESIAN_POINT('Ctrl Pts',(-38.4606914472883,17.1567656550912,-2.5));
#38769=CARTESIAN_POINT('Ctrl Pts',(-37.9859246535537,17.3977243429034,-2.5));
#38770=CARTESIAN_POINT('Ctrl Pts',(-38.4157502976598,17.1429009507965,-3.03374623521863));
#38771=CARTESIAN_POINT('Ctrl Pts',(-38.4472751802113,17.1252685427155,-2.5));
#38772=CARTESIAN_POINT('Ctrl Pts',(-37.9802343339963,17.3867353766995,-2.5));
#38773=CARTESIAN_POINT('Ctrl Pts',(-38.4025443177972,17.1204528053856,-3.03559000380591));
#38774=CARTESIAN_POINT('Ctrl Pts',(-38.4352923297066,17.1007128648909,-2.5));
#38775=CARTESIAN_POINT('Ctrl Pts',(-37.9752820848364,17.3782217794531,-2.5));
#38776=CARTESIAN_POINT('Ctrl Pts',(-38.3597927098826,17.0552514733911,-3.04091068696068));
#38777=CARTESIAN_POINT('Ctrl Pts',(-38.3955062069388,17.0287324610293,-2.5));
#38778=CARTESIAN_POINT('Ctrl Pts',(-37.9592502348198,17.3534964507582,-2.5));
#38779=CARTESIAN_POINT('Ctrl Pts',(-38.3271443327293,17.0146202226201,-3.04417881485026));
#38780=CARTESIAN_POINT('Ctrl Pts',(-38.3640171485458,16.9833146484955,-2.5));
#38781=CARTESIAN_POINT('Ctrl Pts',(-37.9470071050743,17.3380921508149,-2.5));
#38782=CARTESIAN_POINT('Ctrl Pts',(-38.2809131555838,16.9675438780044,-3.0479256286666));
#38783=CARTESIAN_POINT('Ctrl Pts',(-38.3181512189723,16.9301557601742,-2.5));
#38784=CARTESIAN_POINT('Ctrl Pts',(-37.9296703965765,17.3202474359949,-2.5));
#38785=CARTESIAN_POINT('Ctrl Pts',(-38.2714380751677,16.9583630961748,-3.04865416425237));
#38786=CARTESIAN_POINT('Ctrl Pts',(-38.3086648857525,16.9197304651529,-2.5));
#38787=CARTESIAN_POINT('Ctrl Pts',(-37.9261172426642,17.3167675393722,-2.5));
#38788=CARTESIAN_POINT('Ctrl Pts',(-38.2521347050763,16.9405580024456,-3.05006336142326));
#38789=CARTESIAN_POINT('Ctrl Pts',(-38.2892172779821,16.8994516379931,-2.5));
#38790=CARTESIAN_POINT('Ctrl Pts',(-37.9188784832198,17.3100189529994,-2.5));
#38791=CARTESIAN_POINT('Ctrl Pts',(-38.2422914181653,16.9319183323786,-3.05074524347667));
#38792=CARTESIAN_POINT('Ctrl Pts',(-38.2792412041749,16.8895824979303,-2.5));
#38793=CARTESIAN_POINT('Ctrl Pts',(-37.9151872472733,17.3067444493034,-2.5));
#38794=CARTESIAN_POINT('Ctrl Pts',(-38.2121946005029,16.9067773575311,-3.05272459995863));
#38795=CARTESIAN_POINT('Ctrl Pts',(-38.2485441235301,16.860762254136,-2.5));
#38796=CARTESIAN_POINT('Ctrl Pts',(-37.9039009442048,17.2972161773508,-2.5));
#38797=CARTESIAN_POINT('Ctrl Pts',(-38.1913754559341,16.8910522598471,-3.05395594589729));
#38798=CARTESIAN_POINT('Ctrl Pts',(-38.227102342556,16.842648790628,-2.5));
#38799=CARTESIAN_POINT('Ctrl Pts',(-37.8960937635255,17.2912569793141,-2.5));
#38800=CARTESIAN_POINT('Ctrl Pts',(-38.1482366444428,16.861662216655,-3.05624785925289));
#38801=CARTESIAN_POINT('Ctrl Pts',(-38.1822556751584,16.8086281750341,-2.5));
#38802=CARTESIAN_POINT('Ctrl Pts',(-37.8799167074083,17.280120019,-2.5));
#38803=CARTESIAN_POINT('Ctrl Pts',(-38.1259170445788,16.8479971821675,-3.05730841943199));
#38804=CARTESIAN_POINT('Ctrl Pts',(-38.1588541824173,16.7927328735794,-2.5));
#38805=CARTESIAN_POINT('Ctrl Pts',(-37.8715468617295,17.274942215395,-2.5));
#38806=CARTESIAN_POINT('Ctrl Pts',(-38.0912859803399,16.829081464749,-3.05877140147105));
#38807=CARTESIAN_POINT('Ctrl Pts',(-38.1222868782628,16.7706491428746,-2.5));
#38808=CARTESIAN_POINT('Ctrl Pts',(-37.8585602075906,17.2677752860875,-2.5));
#38809=CARTESIAN_POINT('Ctrl Pts',(-38.0795482163152,16.8230394748505,-3.05923777409933));
#38810=CARTESIAN_POINT('Ctrl Pts',(-38.1098421306826,16.7635765111134,-2.5));
#38811=CARTESIAN_POINT('Ctrl Pts',(-37.854158548831,17.2654861133914,-2.5));
#38812=CARTESIAN_POINT('Ctrl Pts',(-38.0556863997546,16.8114994618048,-3.06012706376275));
#38813=CARTESIAN_POINT('Ctrl Pts',(-38.0844586622232,16.7500420272248,-2.5));
#38814=CARTESIAN_POINT('Ctrl Pts',(-37.8452103654877,17.2611139901796,-2.5));
#38815=CARTESIAN_POINT('Ctrl Pts',(-38.0436500462945,16.8060440839517,-3.06054669237718));
#38816=CARTESIAN_POINT('Ctrl Pts',(-38.0716141384825,16.7436315079723,-2.5));
#38817=CARTESIAN_POINT('Ctrl Pts',(-37.8406967327678,17.2590471876283,-2.5));
#38818=CARTESIAN_POINT('Ctrl Pts',(-37.983033732995,16.7803474050268,-3.06252042955387));
#38819=CARTESIAN_POINT('Ctrl Pts',(-38.006651933923,16.7133430503521,-2.5));
#38820=CARTESIAN_POINT('Ctrl Pts',(-37.817965621475,17.2493120442009,-2.5));
#38821=CARTESIAN_POINT('Ctrl Pts',(-37.9330756082843,16.7647592929747,-3.06370859239269));
#38822=CARTESIAN_POINT('Ctrl Pts',(-37.9526360706556,16.6948699048902,-2.5));
#38823=CARTESIAN_POINT('Ctrl Pts',(-37.7992313215639,17.2434072153618,-2.5));
#38824=CARTESIAN_POINT('Ctrl Pts',(-37.8688152137882,16.7514251465279,-3.06472324864037));
#38825=CARTESIAN_POINT('Ctrl Pts',(-37.8827461609207,16.6790214482703,-2.5));
#38826=CARTESIAN_POINT('Ctrl Pts',(-37.7751336713641,17.2383563320521,-2.5));
#38827=CARTESIAN_POINT('Ctrl Pts',(-37.8558716761049,16.7490686581359,-3.06490240337987));
#38828=CARTESIAN_POINT('Ctrl Pts',(-37.8686399794402,16.6762161508003,-2.5));
#38829=CARTESIAN_POINT('Ctrl Pts',(-37.7702798457447,17.2374637147322,-2.5));
#38830=CARTESIAN_POINT('Ctrl Pts',(-37.836316999401,16.7460068446618,-3.06513506367886));
#38831=CARTESIAN_POINT('Ctrl Pts',(-37.8473067499512,16.6725690712863,-2.5));
#38832=CARTESIAN_POINT('Ctrl Pts',(-37.762946841142,17.2363039481978,-2.5));
#38833=CARTESIAN_POINT('Ctrl Pts',(-37.829775537342,16.7450650975492,-3.06520660039349));
#38834=CARTESIAN_POINT('Ctrl Pts',(-37.8401659882031,16.6714468083953,-2.5));
#38835=CARTESIAN_POINT('Ctrl Pts',(-37.7604937934312,17.23594722548,-2.5));
#38836=CARTESIAN_POINT('Ctrl Pts',(-37.8166456311835,16.7433410180028,-3.0653375358751));
#38837=CARTESIAN_POINT('Ctrl Pts',(-37.82582654984,16.669391703467,-2.5));
#38838=CARTESIAN_POINT('Ctrl Pts',(-37.7555700780584,17.2352941782029,-2.5));
#38839=CARTESIAN_POINT('Ctrl Pts',(-37.8100479347227,16.7425577604292,-3.06539700330435));
#38840=CARTESIAN_POINT('Ctrl Pts',(-37.818617934926,16.668457783908,-2.5));
#38841=CARTESIAN_POINT('Ctrl Pts',(-37.7530959419294,17.2349974951212,-2.5));
#38842=CARTESIAN_POINT('Ctrl Pts',(-37.777067284866,16.7390579643222,-3.06566266886128));
#38843=CARTESIAN_POINT('Ctrl Pts',(-37.7825632243643,16.6642830215665,-2.5));
#38844=CARTESIAN_POINT('Ctrl Pts',(-37.7407281994226,17.2336718308661,-2.5));
#38845=CARTESIAN_POINT('Ctrl Pts',(-37.7507569280122,16.7375882697876,-3.06577409663493));
#38846=CARTESIAN_POINT('Ctrl Pts',(-37.7537706577765,16.6625286572503,-2.5));
#38847=CARTESIAN_POINT('Ctrl Pts',(-37.7308618146269,17.2331151625715,-2.5));
#38848=CARTESIAN_POINT('Ctrl Pts',(-37.6720409935013,16.7370385868534,-3.06581578422071));
#38849=CARTESIAN_POINT('Ctrl Pts',(-37.6675998077381,16.6618723975768,-2.5));
#38850=CARTESIAN_POINT('Ctrl Pts',(-37.7013433392571,17.2329069461004,-2.5));
#38851=CARTESIAN_POINT('Ctrl Pts',(-37.6198485285534,16.7417812990776,-3.06545669284864));
#38852=CARTESIAN_POINT('Ctrl Pts',(-37.6105054868964,16.6675345545024,-2.5));
#38853=CARTESIAN_POINT('Ctrl Pts',(-37.6817711620469,17.2347033137879,-2.5));
#38854=CARTESIAN_POINT('Ctrl Pts',(-37.5549716201007,16.7542328279335,-3.06450964654665));
#38855=CARTESIAN_POINT('Ctrl Pts',(-37.539791579201,16.6823618030451,-2.5));
#38856=CARTESIAN_POINT('Ctrl Pts',(-37.6574423248857,17.2394198627989,-2.5));
#38857=CARTESIAN_POINT('Ctrl Pts',(-37.5419780772432,16.7570618699045,-3.06429433377577));
#38858=CARTESIAN_POINT('Ctrl Pts',(-37.5256575742345,16.6857256023118,-2.5));
#38859=CARTESIAN_POINT('Ctrl Pts',(-37.6525697466396,17.2404914902659,-2.5));
#38860=CARTESIAN_POINT('Ctrl Pts',(-37.5162549007385,16.7633361071356,-3.06381631649363));
#38861=CARTESIAN_POINT('Ctrl Pts',(-37.4977213282955,16.6931780113973,-2.5));
#38862=CARTESIAN_POINT('Ctrl Pts',(-37.642923553396,17.2428681687046,-2.5));
#38863=CARTESIAN_POINT('Ctrl Pts',(-37.5035214136028,16.7667796187423,-3.0635537446777));
#38864=CARTESIAN_POINT('Ctrl Pts',(-37.4839161235599,16.6972638969602,-2.5));
#38865=CARTESIAN_POINT('Ctrl Pts',(-37.6381484975799,17.2441725977466,-2.5));
#38866=CARTESIAN_POINT('Ctrl Pts',(-37.4656977945507,16.7780114577165,-3.06269625818825));
#38867=CARTESIAN_POINT('Ctrl Pts',(-37.4430016133797,16.7105699687229,-2.5));
#38868=CARTESIAN_POINT('Ctrl Pts',(-37.6239646379375,17.2484273528784,-2.5));
#38869=CARTESIAN_POINT('Ctrl Pts',(-37.4409836224016,16.7866989403601,-3.06203177270948));
#38870=CARTESIAN_POINT('Ctrl Pts',(-37.4163729269822,16.720839368388,-2.5));
#38871=CARTESIAN_POINT('Ctrl Pts',(-37.6146968252125,17.2517183816627,-2.5));
#38872=CARTESIAN_POINT('Ctrl Pts',(-37.3925416751236,16.80643246839,-3.06051737328866));
#38873=CARTESIAN_POINT('Ctrl Pts',(-37.3644453567216,16.7440900855917,-2.5));
#38874=CARTESIAN_POINT('Ctrl Pts',(-37.5965310946519,17.2591942841924,-2.5));
#38875=CARTESIAN_POINT('Ctrl Pts',(-37.3688139142769,16.8174785426132,-3.05966746752498));
#38876=CARTESIAN_POINT('Ctrl Pts',(-37.3391549609578,16.7570619950295,-2.5));
#38877=CARTESIAN_POINT('Ctrl Pts',(-37.5876331822018,17.2633791709517,-2.5));
#38878=CARTESIAN_POINT('Ctrl Pts',(-37.3339711607475,16.8358377670208,-3.05824914363553));
#38879=CARTESIAN_POINT('Ctrl Pts',(-37.3022443333108,16.7785464121055,-2.5));
#38880=CARTESIAN_POINT('Ctrl Pts',(-37.5745671530757,17.270335145276,-2.5));
#38881=CARTESIAN_POINT('Ctrl Pts',(-37.3224819496572,16.8422563904187,-3.05775241081752));
#38882=CARTESIAN_POINT('Ctrl Pts',(-37.2901231475283,16.7860382908692,-2.5));
#38883=CARTESIAN_POINT('Ctrl Pts',(-37.570258695808,17.2727671020922,-2.5));
#38884=CARTESIAN_POINT('Ctrl Pts',(-37.2997579173503,16.8557016280555,-3.05670968389331));
#38885=CARTESIAN_POINT('Ctrl Pts',(-37.2662411766355,16.8016967416051,-2.5));
#38886=CARTESIAN_POINT('Ctrl Pts',(-37.5617371876123,17.2778615635871,-2.5));
#38887=CARTESIAN_POINT('Ctrl Pts',(-37.2885084984505,16.8627400253605,-3.0561627663965));
#38888=CARTESIAN_POINT('Ctrl Pts',(-37.2544661462563,16.8098753233558,-2.5));
#38889=CARTESIAN_POINT('Ctrl Pts',(-37.5575186558127,17.2805285214769,-2.5));
#38890=CARTESIAN_POINT('Ctrl Pts',(-37.2335131076936,16.8990718659001,-3.05333313807168));
#38891=CARTESIAN_POINT('Ctrl Pts',(-37.1972561950466,16.8519104255022,-2.5));
#38892=CARTESIAN_POINT('Ctrl Pts',(-37.5368953730412,17.2942956929266,-2.5));
#38893=CARTESIAN_POINT('Ctrl Pts',(-37.1930113241315,16.9320140399769,-3.05074799765065));
#38894=CARTESIAN_POINT('Ctrl Pts',(-37.1558511506002,16.8897253205875,-2.5));
#38895=CARTESIAN_POINT('Ctrl Pts',(-37.5217072095524,17.3067799280439,-2.5));
#38896=CARTESIAN_POINT('Ctrl Pts',(-37.1373488654157,16.987068334806,-3.04637357495642));
#38897=CARTESIAN_POINT('Ctrl Pts',(-37.1001829683923,16.9522623708449,-2.5));
#38898=CARTESIAN_POINT('Ctrl Pts',(-37.5008337929987,17.3276482177729,-2.5));
#38899=CARTESIAN_POINT('Ctrl Pts',(-37.119649230241,17.0063667438965,-3.04483205480724));
#38900=CARTESIAN_POINT('Ctrl Pts',(-37.08275128213,16.9740145507512,-2.5));
#38901=CARTESIAN_POINT('Ctrl Pts',(-37.4941964218283,17.334963880511,-2.5));
#38902=CARTESIAN_POINT('Ctrl Pts',(-37.09862407612,17.0317074280592,-3.04279459962286));
#38903=CARTESIAN_POINT('Ctrl Pts',(-37.0623359323734,17.0024240843538,-2.5));
#38904=CARTESIAN_POINT('Ctrl Pts',(-37.4863119967309,17.344571096994,-2.5));
#38905=CARTESIAN_POINT('Ctrl Pts',(-37.0944707116322,17.0368412601703,-3.04238118958153));
#38906=CARTESIAN_POINT('Ctrl Pts',(-37.0583251973171,17.0081622414672,-2.5));
#38907=CARTESIAN_POINT('Ctrl Pts',(-37.4847544852643,17.3465174947961,-2.5));
#38908=CARTESIAN_POINT('Ctrl Pts',(-37.086318602129,17.0471765103316,-3.04154758456322));
#38909=CARTESIAN_POINT('Ctrl Pts',(-37.0504867079477,17.0196942280984,-2.5));
#38910=CARTESIAN_POINT('Ctrl Pts',(-37.4816974406886,17.350436015139,-2.5));
#38911=CARTESIAN_POINT('Ctrl Pts',(-37.0823147848581,17.0523838124048,-3.04112691976143));
#38912=CARTESIAN_POINT('Ctrl Pts',(-37.0466539524108,17.0254945229426,-2.5));
#38913=CARTESIAN_POINT('Ctrl Pts',(-37.4801960124776,17.3524103736432,-2.5));
#38914=CARTESIAN_POINT('Ctrl Pts',(-37.0705176170079,17.0681234054201,-3.03985333807572));
#38915=CARTESIAN_POINT('Ctrl Pts',(-37.0354170178543,17.0429878142689,-2.5));
#38916=CARTESIAN_POINT('Ctrl Pts',(-37.475772070005,17.3583782202939,-2.5));
#38917=CARTESIAN_POINT('Ctrl Pts',(-37.0629384235517,17.0787733000584,-3.03898884786155));
#38918=CARTESIAN_POINT('Ctrl Pts',(-37.0282631566779,17.0547884840968,-2.5));
#38919=CARTESIAN_POINT('Ctrl Pts',(-37.4729298774794,17.3624164681974,-2.5));
#38920=CARTESIAN_POINT('Ctrl Pts',(-37.026446523552,17.132793523799,-3.03458889787333));
#38921=CARTESIAN_POINT('Ctrl Pts',(-36.9942613247177,17.1142615428478,-2.5));
#38922=CARTESIAN_POINT('Ctrl Pts',(-37.4592454049732,17.3829010974121,-2.5));
#38923=CARTESIAN_POINT('Ctrl Pts',(-37.0017062809529,17.1784542255603,-3.03082304423241));
#38924=CARTESIAN_POINT('Ctrl Pts',(-36.9722499558993,17.1639506562642,-2.5));
#38925=CARTESIAN_POINT('Ctrl Pts',(-37.4499678115662,17.4002194094609,-2.5));
#38926=CARTESIAN_POINT('Ctrl Pts',(-36.9763738972329,17.2385950219028,-3.02578307239997));
#38927=CARTESIAN_POINT('Ctrl Pts',(-36.9511407639783,17.2285709769479,-2.5));
#38928=CARTESIAN_POINT('Ctrl Pts',(-37.4404681807179,17.4230360661467,-2.5));
#38929=CARTESIAN_POINT('Ctrl Pts',(-36.9715895606736,17.2507777927924,-3.02475831530062));
#38930=CARTESIAN_POINT('Ctrl Pts',(-36.9472559919366,17.2415671008265,-2.5));
#38931=CARTESIAN_POINT('Ctrl Pts',(-37.4386740479595,17.4276583514805,-2.5));
#38932=CARTESIAN_POINT('Ctrl Pts',(-36.9625961480096,17.2754584703774,-3.02267407819011));
#38933=CARTESIAN_POINT('Ctrl Pts',(-36.9401413648218,17.2677878485332,-2.5));
#38934=CARTESIAN_POINT('Ctrl Pts',(-37.4353015260892,17.4370231465561,-2.5));
#38935=CARTESIAN_POINT('Ctrl Pts',(-36.9584132845463,17.2878868497566,-3.02162045942486));
#38936=CARTESIAN_POINT('Ctrl Pts',(-36.9369311676226,17.2809375542772,-2.5));
#38937=CARTESIAN_POINT('Ctrl Pts',(-37.4337329516611,17.441739269899,-2.5));
#38938=CARTESIAN_POINT('Ctrl Pts',(-36.9468363797903,17.3252899977778,-3.01843695447992));
#38939=CARTESIAN_POINT('Ctrl Pts',(-36.9283615872827,17.3203042842923,-2.5));
#38940=CARTESIAN_POINT('Ctrl Pts',(-37.4293916024477,17.4559334232034,-2.5));
#38941=CARTESIAN_POINT('Ctrl Pts',(-36.9403896403824,17.3504426477826,-3.01627937557837));
#38942=CARTESIAN_POINT('Ctrl Pts',(-36.9240158817722,17.3465871928938,-2.5));
#38943=CARTESIAN_POINT('Ctrl Pts',(-37.4269740834161,17.4654799598295,-2.5));
#38944=CARTESIAN_POINT('Ctrl Pts',(-36.9299795767171,17.401171550854,-3.01189204818851));
#38945=CARTESIAN_POINT('Ctrl Pts',(-36.9179681053284,17.3991512563075,-2.5));
#38946=CARTESIAN_POINT('Ctrl Pts',(-37.4230703062887,17.4847366734944,-2.5));
#38947=CARTESIAN_POINT('Ctrl Pts',(-36.9260163611498,17.4267478207179,-3.0096623048872));
#38948=CARTESIAN_POINT('Ctrl Pts',(-36.9162547401427,17.4254293823291,-2.5));
#38949=CARTESIAN_POINT('Ctrl Pts',(-37.421584098594,17.4944468593896,-2.5));
#38950=CARTESIAN_POINT('Ctrl Pts',(-36.9205861826877,17.4783255467987,-3.0051277827859));
#38951=CARTESIAN_POINT('Ctrl Pts',(-36.91541973322,17.4779707405914,-2.5));
#38952=CARTESIAN_POINT('Ctrl Pts',(-37.4195477886376,17.5140317228638,-2.5));
#38953=CARTESIAN_POINT('Ctrl Pts',(-36.919118933325,17.5043343662994,-3.00282235189172));
#38954=CARTESIAN_POINT('Ctrl Pts',(-36.9162867050069,17.5042383112405,-2.5));
#38955=CARTESIAN_POINT('Ctrl Pts',(-37.4189975669682,17.5239091955899,-2.5));
#38956=CARTESIAN_POINT('Ctrl Pts',(-36.918942728626,17.5305480494939,-3.00047863991406));
#38957=CARTESIAN_POINT('Ctrl Pts',(-36.9184636408495,17.5305448701384,-2.5));
#38958=CARTESIAN_POINT('Ctrl Pts',(-37.418931489881,17.5338661095488,-2.5));
#38959=CARTESIAN_POINT('',(-38.0189154695161,17.5383073665604,-2.5));
#38960=CARTESIAN_POINT('Origin',(-38.0189152720306,17.538307365007,-3.));
#38961=CARTESIAN_POINT('',(-37.4189314692081,17.5338661094116,-2.5));
#38962=CARTESIAN_POINT('Ctrl Pts',(-37.4189314692081,17.5338661094116,-2.5));
#38963=CARTESIAN_POINT('Ctrl Pts',(-37.418924080912,17.5349752987399,-2.5));
#38964=CARTESIAN_POINT('Ctrl Pts',(-37.4189227173758,17.5360840623156,-2.5));
#38965=CARTESIAN_POINT('Ctrl Pts',(-37.418927375124,17.5371921369015,-2.50000000000001));
#38966=CARTESIAN_POINT('Ctrl Pts',(-37.4189482673457,17.5421623797679,-2.50000000000001));
#38967=CARTESIAN_POINT('Ctrl Pts',(-37.4190900906852,17.547112870658,-2.5));
#38968=CARTESIAN_POINT('Ctrl Pts',(-37.4193504503231,17.5520440628482,-2.5));
#38969=CARTESIAN_POINT('Ctrl Pts',(-37.4195528629438,17.5558777428411,-2.5));
#38970=CARTESIAN_POINT('Ctrl Pts',(-37.4198270040927,17.5596999384012,-2.5));
#38971=CARTESIAN_POINT('Ctrl Pts',(-37.4201718933211,17.5635102713167,-2.5));
#38972=CARTESIAN_POINT('Ctrl Pts',(-37.4207142534576,17.5695022609473,-2.5));
#38973=CARTESIAN_POINT('Ctrl Pts',(-37.4214316067083,17.5754659138134,-2.5));
#38974=CARTESIAN_POINT('Ctrl Pts',(-37.4223232424291,17.5814010980502,-2.5));
#38975=CARTESIAN_POINT('Ctrl Pts',(-37.4228904665252,17.5851768322829,-2.5));
#38976=CARTESIAN_POINT('Ctrl Pts',(-37.4235282497785,17.5889410563489,-2.5));
#38977=CARTESIAN_POINT('Ctrl Pts',(-37.424236403788,17.5926938015469,-2.5));
#38978=CARTESIAN_POINT('Ctrl Pts',(-37.4253492854007,17.5985913338245,-2.5));
#38979=CARTESIAN_POINT('Ctrl Pts',(-37.4266359441733,17.6044605190523,-2.5));
#38980=CARTESIAN_POINT('Ctrl Pts',(-37.4280987205395,17.610300986808,-2.5));
#38981=CARTESIAN_POINT('Ctrl Pts',(-37.4290298839969,17.6140188689625,-2.5));
#38982=CARTESIAN_POINT('Ctrl Pts',(-37.4300325085037,17.6177254059074,-2.5));
#38983=CARTESIAN_POINT('Ctrl Pts',(-37.4311069581255,17.6214196423252,-2.5));
#38984=CARTESIAN_POINT('Ctrl Pts',(-37.4314134572077,17.6224734656487,-2.5));
#38985=CARTESIAN_POINT('Ctrl Pts',(-37.4317258579008,17.6235264245972,-2.5));
#38986=CARTESIAN_POINT('Ctrl Pts',(-37.4320441492926,17.6245784015581,-2.5));
#38987=CARTESIAN_POINT('Ctrl Pts',(-37.4331601682326,17.628266927994,-2.5));
#38988=CARTESIAN_POINT('Ctrl Pts',(-37.4343492641677,17.6319454076607,-2.5));
#38989=CARTESIAN_POINT('Ctrl Pts',(-37.4356108634578,17.6356081256996,-2.5));
#38990=CARTESIAN_POINT('Ctrl Pts',(-37.4359704139135,17.6366519848316,-2.5));
#38991=CARTESIAN_POINT('Ctrl Pts',(-37.4363352907883,17.63769295271,-2.5));
#38992=CARTESIAN_POINT('Ctrl Pts',(-37.4367054529537,17.638730998124,-2.5));
#38993=CARTESIAN_POINT('Ctrl Pts',(-37.4380045061287,17.6423739317277,-2.5));
#38994=CARTESIAN_POINT('Ctrl Pts',(-37.4393688887006,17.6459815111093,-2.5));
#38995=CARTESIAN_POINT('Ctrl Pts',(-37.440797406153,17.6495538350512,-2.5));
#38996=CARTESIAN_POINT('Ctrl Pts',(-37.4467102048854,17.6643400964579,-2.5));
#38997=CARTESIAN_POINT('Ctrl Pts',(-37.4537132952356,17.6785310992158,-2.49999999999996));
#38998=CARTESIAN_POINT('Ctrl Pts',(-37.461799572854,17.6921314373255,-2.50000000000007));
#38999=CARTESIAN_POINT('Ctrl Pts',(-37.4637549480288,17.6954201895505,-2.5000000000001));
#39000=CARTESIAN_POINT('Ctrl Pts',(-37.4657735120508,17.6986739789099,-2.50000000000008));
#39001=CARTESIAN_POINT('Ctrl Pts',(-37.4678552376092,17.7018931471268,-2.50000000000005));
#39002=CARTESIAN_POINT('Ctrl Pts',(-37.4711178370673,17.706938411829,-2.50000000000001));
#39003=CARTESIAN_POINT('Ctrl Pts',(-37.4745386091628,17.7119005181788,-2.5));
#39004=CARTESIAN_POINT('Ctrl Pts',(-37.4781182518123,17.7167738292873,-2.5));
#39005=CARTESIAN_POINT('Ctrl Pts',(-37.4804030608609,17.7198843591383,-2.5));
#39006=CARTESIAN_POINT('Ctrl Pts',(-37.4827540352099,17.7229605353768,-2.49999999999995));
#39007=CARTESIAN_POINT('Ctrl Pts',(-37.4851688194139,17.725997596559,-2.50000000000007));
#39008=CARTESIAN_POINT('Ctrl Pts',(-37.4858526471977,17.7268576431063,-2.5000000000001));
#39009=CARTESIAN_POINT('Ctrl Pts',(-37.4865404402418,17.7277131251369,-2.50000000000015));
#39010=CARTESIAN_POINT('Ctrl Pts',(-37.4872321232356,17.728563994922,-2.50000000000025));
#39011=CARTESIAN_POINT('Ctrl Pts',(-37.4903663293432,17.7324195202151,-2.50000000000068));
#39012=CARTESIAN_POINT('Ctrl Pts',(-37.4935839883218,17.7361819881709,-2.5));
#39013=CARTESIAN_POINT('Ctrl Pts',(-37.4968822816754,17.7398546535842,-2.5));
#39014=CARTESIAN_POINT('Ctrl Pts',(-37.4994535903269,17.7427178180573,-2.5));
#39015=CARTESIAN_POINT('Ctrl Pts',(-37.5020742944106,17.7455259637112,-2.5));
#39016=CARTESIAN_POINT('Ctrl Pts',(-37.5047437562526,17.7482797483086,-2.5));
#39017=CARTESIAN_POINT('Ctrl Pts',(-37.5157710837796,17.7596554062098,-2.5));
#39018=CARTESIAN_POINT('Ctrl Pts',(-37.5276248076514,17.7701102809069,-2.5));
#39019=CARTESIAN_POINT('Ctrl Pts',(-37.5403203589352,17.7796263513267,-2.5));
#39020=CARTESIAN_POINT('Ctrl Pts',(-37.5433960495854,17.7819317643145,-2.5));
#39021=CARTESIAN_POINT('Ctrl Pts',(-37.5465218144476,17.7841825394691,-2.5));
#39022=CARTESIAN_POINT('Ctrl Pts',(-37.5496960494136,17.786377178086,-2.5));
#39023=CARTESIAN_POINT('Ctrl Pts',(-37.5505903348199,17.7869954792855,-2.5));
#39024=CARTESIAN_POINT('Ctrl Pts',(-37.5514888101488,17.787609476892,-2.5));
#39025=CARTESIAN_POINT('Ctrl Pts',(-37.5523912367608,17.7882189895587,-2.5));
#39026=CARTESIAN_POINT('Ctrl Pts',(-37.5555951317451,17.7903829489877,-2.5));
#39027=CARTESIAN_POINT('Ctrl Pts',(-37.5588532093185,17.7924931481196,-2.5));
#39028=CARTESIAN_POINT('Ctrl Pts',(-37.5621535646477,17.7945404310863,-2.5));
#39029=CARTESIAN_POINT('Ctrl Pts',(-37.5630823747426,17.7951165924074,-2.5));
#39030=CARTESIAN_POINT('Ctrl Pts',(-37.5640134395123,17.7956871178347,-2.5));
#39031=CARTESIAN_POINT('Ctrl Pts',(-37.564946673507,17.7962519914256,-2.5));
#39032=CARTESIAN_POINT('Ctrl Pts',(-37.5682633047709,17.7982595023205,-2.5));
#39033=CARTESIAN_POINT('Ctrl Pts',(-37.5716089097383,17.800196530261,-2.5));
#39034=CARTESIAN_POINT('Ctrl Pts',(-37.5749830496898,17.8020641498484,-2.5));
#39035=CARTESIAN_POINT('Ctrl Pts',(-37.5802548890879,17.8049821647094,-2.5));
#39036=CARTESIAN_POINT('Ctrl Pts',(-37.58559627027,17.8077310264052,-2.5));
#39037=CARTESIAN_POINT('Ctrl Pts',(-37.5910065014943,17.8103124473042,-2.5));
#39038=CARTESIAN_POINT('Ctrl Pts',(-37.5944705744368,17.8119652842937,-2.5));
#39039=CARTESIAN_POINT('Ctrl Pts',(-37.5979628694577,17.8135494693829,-2.5));
#39040=CARTESIAN_POINT('Ctrl Pts',(-37.6014832022656,17.8150654513137,-2.5));
#39041=CARTESIAN_POINT('Ctrl Pts',(-37.6105016362735,17.8189491133836,-2.5));
#39042=CARTESIAN_POINT('Ctrl Pts',(-37.6197040838036,17.8223851534601,-2.5));
#39043=CARTESIAN_POINT('Ctrl Pts',(-37.629092831199,17.8253680273689,-2.5));
#39044=CARTESIAN_POINT('Ctrl Pts',(-37.6337872059174,17.8268594646476,-2.5));
#39045=CARTESIAN_POINT('Ctrl Pts',(-37.6385282342954,17.8282374191786,-2.5));
#39046=CARTESIAN_POINT('Ctrl Pts',(-37.6433167322283,17.8294999097575,-2.5));
#39047=CARTESIAN_POINT('Ctrl Pts',(-37.644363925716,17.8297760029982,-2.5));
#39048=CARTESIAN_POINT('Ctrl Pts',(-37.6454133898735,17.8300465731124,-2.5));
#39049=CARTESIAN_POINT('Ctrl Pts',(-37.6464651365387,17.830311591346,-2.5));
#39050=CARTESIAN_POINT('Ctrl Pts',(-37.6478180462502,17.830652496389,-2.5));
#39051=CARTESIAN_POINT('Ctrl Pts',(-37.6491747302882,17.8309842382055,-2.5));
#39052=CARTESIAN_POINT('Ctrl Pts',(-37.6505352154912,17.8313067389472,-2.5));
#39053=CARTESIAN_POINT('Ctrl Pts',(-37.6529533369025,17.8318799505828,-2.50000000000001));
#39054=CARTESIAN_POINT('Ctrl Pts',(-37.6553864837853,17.8324245544573,-2.50000000000003));
#39055=CARTESIAN_POINT('Ctrl Pts',(-37.6578190611257,17.832936920446,-2.50000000000004));
#39056=CARTESIAN_POINT('Ctrl Pts',(-37.6588822778756,17.8331608623912,-2.50000000000004));
#39057=CARTESIAN_POINT('Ctrl Pts',(-37.6599457907485,17.8333788156395,-2.50000000000003));
#39058=CARTESIAN_POINT('Ctrl Pts',(-37.6610095988213,17.833590783111,-2.50000000000002));
#39059=CARTESIAN_POINT('Ctrl Pts',(-37.6658767167307,17.8345605733419,-2.49999999999998));
#39060=CARTESIAN_POINT('Ctrl Pts',(-37.6707498784643,17.8354056443311,-2.5));
#39061=CARTESIAN_POINT('Ctrl Pts',(-37.6756293102449,17.8361269204229,-2.5));
#39062=CARTESIAN_POINT('Ctrl Pts',(-37.6853881738059,17.8375694726066,-2.5));
#39063=CARTESIAN_POINT('Ctrl Pts',(-37.6951719386941,17.8385167826839,-2.49999999999996));
#39064=CARTESIAN_POINT('Ctrl Pts',(-37.7049796194108,17.8389772004795,-2.50000000000004));
#39065=CARTESIAN_POINT('Ctrl Pts',(-37.7088146288424,17.8391572335209,-2.50000000000008));
#39066=CARTESIAN_POINT('Ctrl Pts',(-37.7126533284138,17.8392626978782,-2.50000000000008));
#39067=CARTESIAN_POINT('Ctrl Pts',(-37.716495688883,17.8392941481056,-2.50000000000005));
#39068=CARTESIAN_POINT('Ctrl Pts',(-37.7224798087271,17.839343128916,-2.50000000000002));
#39069=CARTESIAN_POINT('Ctrl Pts',(-37.7284728705124,17.8392112724852,-2.5));
#39070=CARTESIAN_POINT('Ctrl Pts',(-37.7344750534382,17.8388957842887,-2.5));
#39071=CARTESIAN_POINT('Ctrl Pts',(-37.7383305288519,17.8386931318538,-2.5));
#39072=CARTESIAN_POINT('Ctrl Pts',(-37.7421906430535,17.8384145663926,-2.5));
#39073=CARTESIAN_POINT('Ctrl Pts',(-37.7460528064355,17.838059592336,-2.5));
#39074=CARTESIAN_POINT('Ctrl Pts',(-37.7471272624033,17.837960838359,-2.50000000000001));
#39075=CARTESIAN_POINT('Ctrl Pts',(-37.7482024838803,17.8378560565892,-2.50000000000001));
#39076=CARTESIAN_POINT('Ctrl Pts',(-37.7492777731307,17.8377453314094,-2.50000000000002));
#39077=CARTESIAN_POINT('Ctrl Pts',(-37.7531438406325,17.8373472329264,-2.50000000000005));
#39078=CARTESIAN_POINT('Ctrl Pts',(-37.757017212452,17.8368712456081,-2.50000000000001));
#39079=CARTESIAN_POINT('Ctrl Pts',(-37.7608631543582,17.8363214679065,-2.5));
#39080=CARTESIAN_POINT('Ctrl Pts',(-37.7619319418431,17.8361686846505,-2.5));
#39081=CARTESIAN_POINT('Ctrl Pts',(-37.7629989602928,17.8360102070827,-2.5));
#39082=CARTESIAN_POINT('Ctrl Pts',(-37.7640641141128,17.8358460852665,-2.5));
#39083=CARTESIAN_POINT('Ctrl Pts',(-37.7678975817809,17.835255414075,-2.5));
#39084=CARTESIAN_POINT('Ctrl Pts',(-37.7717092081801,17.8345911184888,-2.5));
#39085=CARTESIAN_POINT('Ctrl Pts',(-37.7754993148818,17.8338542984479,-2.5));
#39086=CARTESIAN_POINT('Ctrl Pts',(-37.79107968017,17.830825379662,-2.5));
#39087=CARTESIAN_POINT('Ctrl Pts',(-37.8062996088011,17.8265817597102,-2.49999999999996));
#39088=CARTESIAN_POINT('Ctrl Pts',(-37.8211596455932,17.8211262245503,-2.50000000000007));
#39089=CARTESIAN_POINT('Ctrl Pts',(-37.8247778021374,17.8197978980787,-2.5000000000001));
#39090=CARTESIAN_POINT('Ctrl Pts',(-37.8283738571345,17.8183979213105,-2.50000000000008));
#39091=CARTESIAN_POINT('Ctrl Pts',(-37.8319487721061,17.8169260699933,-2.50000000000006));
#39092=CARTESIAN_POINT('Ctrl Pts',(-37.836512836464,17.8150469695978,-2.50000000000003));
#39093=CARTESIAN_POINT('Ctrl Pts',(-37.8410421353742,17.8130496817546,-2.50000000000001));
#39094=CARTESIAN_POINT('Ctrl Pts',(-37.8455379349741,17.8109311783838,-2.50000000000002));
#39095=CARTESIAN_POINT('Ctrl Pts',(-37.8465112351386,17.8104725414643,-2.50000000000002));
#39096=CARTESIAN_POINT('Ctrl Pts',(-37.8474829057772,17.8100082029157,-2.50000000000002));
#39097=CARTESIAN_POINT('Ctrl Pts',(-37.8484524731366,17.8095384110422,-2.50000000000003));
#39098=CARTESIAN_POINT('Ctrl Pts',(-37.8519612366045,17.807838283096,-2.50000000000004));
#39099=CARTESIAN_POINT('Ctrl Pts',(-37.8554370944497,17.8060691333991,-2.50000000000001));
#39100=CARTESIAN_POINT('Ctrl Pts',(-37.8588613828517,17.8042413401211,-2.5));
#39101=CARTESIAN_POINT('Ctrl Pts',(-37.8598073158636,17.803736426458,-2.5));
#39102=CARTESIAN_POINT('Ctrl Pts',(-37.8607499173818,17.8032267705866,-2.5));
#39103=CARTESIAN_POINT('Ctrl Pts',(-37.8616892897569,17.8027123372952,-2.5));
#39104=CARTESIAN_POINT('Ctrl Pts',(-37.8660292009529,17.8003356495616,-2.5));
#39105=CARTESIAN_POINT('Ctrl Pts',(-37.8702969136781,17.7978586386703,-2.5));
#39106=CARTESIAN_POINT('Ctrl Pts',(-37.8744934438381,17.7952826854476,-2.5));
#39107=CARTESIAN_POINT('Ctrl Pts',(-37.8777830267203,17.7932634430489,-2.5));
#39108=CARTESIAN_POINT('Ctrl Pts',(-37.8810288717245,17.7911833904253,-2.5));
#39109=CARTESIAN_POINT('Ctrl Pts',(-37.8842314572436,17.7890432104997,-2.5));
#39110=CARTESIAN_POINT('Ctrl Pts',(-37.8973710612388,17.780262456158,-2.5));
#39111=CARTESIAN_POINT('Ctrl Pts',(-37.909787707558,17.770476851842,-2.5));
#39112=CARTESIAN_POINT('Ctrl Pts',(-37.9214627815581,17.7596617340041,-2.5));
#39113=CARTESIAN_POINT('Ctrl Pts',(-37.9243104333541,17.7570238329738,-2.5));
#39114=CARTESIAN_POINT('Ctrl Pts',(-37.9271138062512,17.7543248652812,-2.49999999999999));
#39115=CARTESIAN_POINT('Ctrl Pts',(-37.9298738983267,17.7515632530563,-2.5));
#39116=CARTESIAN_POINT('Ctrl Pts',(-37.9306323609192,17.7508043727326,-2.50000000000001));
#39117=CARTESIAN_POINT('Ctrl Pts',(-37.9313866370695,17.7500415820386,-2.50000000000001));
#39118=CARTESIAN_POINT('Ctrl Pts',(-37.9321366200852,17.7492750237347,-2.50000000000002));
#39119=CARTESIAN_POINT('Ctrl Pts',(-37.9348664680114,17.7464848437543,-2.50000000000006));
#39120=CARTESIAN_POINT('Ctrl Pts',(-37.9375346700091,17.7436492082643,-2.50000000000001));
#39121=CARTESIAN_POINT('Ctrl Pts',(-37.9401394064799,17.7407723818853,-2.5));
#39122=CARTESIAN_POINT('Ctrl Pts',(-37.9408544316472,17.7399826654261,-2.5));
#39123=CARTESIAN_POINT('Ctrl Pts',(-37.9415648944728,17.7391896173097,-2.5));
#39124=CARTESIAN_POINT('Ctrl Pts',(-37.9422708937099,17.7383931600166,-2.5));
#39125=CARTESIAN_POINT('Ctrl Pts',(-37.9448433738321,17.735491073942,-2.5));
#39126=CARTESIAN_POINT('Ctrl Pts',(-37.9473544995132,17.7325458015199,-2.5));
#39127=CARTESIAN_POINT('Ctrl Pts',(-37.9498050507074,17.7295578914628,-2.5));
#39128=CARTESIAN_POINT('Ctrl Pts',(-37.953599486724,17.7249314084242,-2.5));
#39129=CARTESIAN_POINT('Ctrl Pts',(-37.9572489362766,17.720202871343,-2.5));
#39130=CARTESIAN_POINT('Ctrl Pts',(-37.9607543179931,17.7153729233453,-2.5));
#39131=CARTESIAN_POINT('Ctrl Pts',(-37.963019073585,17.7122523925099,-2.5));
#39132=CARTESIAN_POINT('Ctrl Pts',(-37.9652236695998,17.7090895187778,-2.5));
#39133=CARTESIAN_POINT('Ctrl Pts',(-37.9673683607455,17.7058844804642,-2.5));
#39134=CARTESIAN_POINT('Ctrl Pts',(-37.9706870703085,17.7009249825326,-2.5));
#39135=CARTESIAN_POINT('Ctrl Pts',(-37.9738623463162,17.6958645281885,-2.5));
#39136=CARTESIAN_POINT('Ctrl Pts',(-37.9768926058306,17.6907019898296,-2.5));
#39137=CARTESIAN_POINT('Ctrl Pts',(-37.9788516386036,17.6873644598956,-2.5));
#39138=CARTESIAN_POINT('Ctrl Pts',(-37.9807502945889,17.6839838181975,-2.5));
#39139=CARTESIAN_POINT('Ctrl Pts',(-37.9825874564246,17.6805610345249,-2.5));
#39140=CARTESIAN_POINT('Ctrl Pts',(-37.983089397607,17.6796258767994,-2.5));
#39141=CARTESIAN_POINT('Ctrl Pts',(-37.9835868344571,17.6786873721866,-2.5));
#39142=CARTESIAN_POINT('Ctrl Pts',(-37.9840796736073,17.6777456651142,-2.5));
#39143=CARTESIAN_POINT('Ctrl Pts',(-37.9858839189027,17.6742981497245,-2.5));
#39144=CARTESIAN_POINT('Ctrl Pts',(-37.9876280092296,17.6708047329094,-2.5));
#39145=CARTESIAN_POINT('Ctrl Pts',(-37.9893067995452,17.6672733142509,-2.5));
#39146=CARTESIAN_POINT('Ctrl Pts',(-37.9897649997402,17.6663094674242,-2.5));
#39147=CARTESIAN_POINT('Ctrl Pts',(-37.9902177317802,17.6653440883829,-2.5));
#39148=CARTESIAN_POINT('Ctrl Pts',(-37.9906650024386,17.6643772306817,-2.5));
#39149=CARTESIAN_POINT('Ctrl Pts',(-37.9923040383024,17.6608341535369,-2.5));
#39150=CARTESIAN_POINT('Ctrl Pts',(-37.9938701991613,17.6572701642616,-2.5));
#39151=CARTESIAN_POINT('Ctrl Pts',(-37.9953647259209,17.6536856269683,-2.5));
#39152=CARTESIAN_POINT('Ctrl Pts',(-38.0014785926123,17.6390218660013,-2.5));
#39153=CARTESIAN_POINT('Ctrl Pts',(-38.00640415232,17.6240172077284,-2.49999999999996));
#39154=CARTESIAN_POINT('Ctrl Pts',(-38.0101545839031,17.6086755353485,-2.50000000000007));
#39155=CARTESIAN_POINT('Ctrl Pts',(-38.011072015426,17.6049226515687,-2.50000000000009));
#39156=CARTESIAN_POINT('Ctrl Pts',(-38.0119191589871,17.6011490664917,-2.50000000000008));
#39157=CARTESIAN_POINT('Ctrl Pts',(-38.0126960956751,17.5973554922411,-2.50000000000005));
#39158=CARTESIAN_POINT('Ctrl Pts',(-38.0136844102185,17.5925298164031,-2.50000000000002));
#39159=CARTESIAN_POINT('Ctrl Pts',(-38.0145581006726,17.5876715036185,-2.5));
#39160=CARTESIAN_POINT('Ctrl Pts',(-38.0153154860037,17.5827814680338,-2.5));
#39161=CARTESIAN_POINT('Ctrl Pts',(-38.015477177083,17.5817375144489,-2.5));
#39162=CARTESIAN_POINT('Ctrl Pts',(-38.0156336037888,17.5806917722016,-2.5));
#39163=CARTESIAN_POINT('Ctrl Pts',(-38.0157847183714,17.5796444881076,-2.5));
#39164=CARTESIAN_POINT('Ctrl Pts',(-38.0163414467211,17.5757861394604,-2.50000000000001));
#39165=CARTESIAN_POINT('Ctrl Pts',(-38.0168265261798,17.5719026151513,-2.5));
#39166=CARTESIAN_POINT('Ctrl Pts',(-38.0172369355354,17.5680093665256,-2.5));
#39167=CARTESIAN_POINT('Ctrl Pts',(-38.0173482325746,17.5669535742082,-2.5));
#39168=CARTESIAN_POINT('Ctrl Pts',(-38.0174539918432,17.5658978049004,-2.50000000000001));
#39169=CARTESIAN_POINT('Ctrl Pts',(-38.0175542183555,17.5648421351762,-2.50000000000001));
#39170=CARTESIAN_POINT('Ctrl Pts',(-38.0180240315044,17.5598936688902,-2.50000000000001));
#39171=CARTESIAN_POINT('Ctrl Pts',(-38.0183723928837,17.5549445094189,-2.5));
#39172=CARTESIAN_POINT('Ctrl Pts',(-38.0186003857153,17.5499946296404,-2.5));
#39173=CARTESIAN_POINT('Ctrl Pts',(-38.0187798053734,17.5460993065656,-2.5));
#39174=CARTESIAN_POINT('Ctrl Pts',(-38.0188847752909,17.5422035509477,-2.50000000000002));
#39175=CARTESIAN_POINT('Ctrl Pts',(-38.0189154695161,17.5383073665604,-2.50000000000004));
#39176=CARTESIAN_POINT('Origin',(-37.418931489881,17.5338661095487,-2.99999999999999));
#39177=CARTESIAN_POINT('Origin',(-37.718924746634,25.7501158975689,-1.15479289890034));
#39178=CARTESIAN_POINT('',(-37.718924746634,25.0506850112887,-0.766467731910881));
#39179=CARTESIAN_POINT('Origin',(-17.718924746634,24.9242463227439,7.77478435608303));
#39180=CARTESIAN_POINT('',(-17.718924746634,24.1393970581951,7.61982748486642));
#39181=CARTESIAN_POINT('Origin',(-17.718924746634,17.0757536772561,6.22521564391699));
#39182=CARTESIAN_POINT('Ctrl Pts',(-18.0133068931633,17.0493818775115,6.22000892238259));
#39183=CARTESIAN_POINT('Ctrl Pts',(-18.0151995259403,17.0589094855094,6.2218900075713));
#39184=CARTESIAN_POINT('Ctrl Pts',(-18.0166154517927,17.0685214343805,6.22378774460121));
#39185=CARTESIAN_POINT('Ctrl Pts',(-18.0175568383944,17.0782373050469,6.22570599946563));
#39186=CARTESIAN_POINT('Ctrl Pts',(-18.0176064793518,17.0787496398519,6.22580715239014));
#39187=CARTESIAN_POINT('Ctrl Pts',(-18.0176547742521,17.079262076957,6.22590832551228));
#39188=CARTESIAN_POINT('Ctrl Pts',(-18.0177017242961,17.0797745926913,6.22600951415857));
#39189=CARTESIAN_POINT('Ctrl Pts',(-18.0180997249336,17.0841192443959,6.22686730133517));
#39190=CARTESIAN_POINT('Ctrl Pts',(-18.0183999920715,17.0884652630194,6.22772535838965));
#39191=CARTESIAN_POINT('Ctrl Pts',(-18.0186030723344,17.0927970021125,6.22858059616219));
#39192=CARTESIAN_POINT('Ctrl Pts',(-18.0188302270038,17.0976422526911,6.22953721917737));
#39193=CARTESIAN_POINT('Ctrl Pts',(-18.0189364808522,17.1024766655667,6.2304917024485));
#39194=CARTESIAN_POINT('Ctrl Pts',(-18.0189238263079,17.1073011345983,6.23144422245482));
#39195=CARTESIAN_POINT('Ctrl Pts',(-18.0188971857286,17.1174576955315,6.23344948509009));
#39196=CARTESIAN_POINT('Ctrl Pts',(-18.0183483687477,17.1275705647777,6.23544612144843));
#39197=CARTESIAN_POINT('Ctrl Pts',(-18.0172736561345,17.1376463417085,6.23743543447808));
#39198=CARTESIAN_POINT('Ctrl Pts',(-18.0163062039052,17.1467165179889,6.23922620654257));
#39199=CARTESIAN_POINT('Ctrl Pts',(-18.0149127944694,17.1557527788852,6.24101028251644));
#39200=CARTESIAN_POINT('Ctrl Pts',(-18.0130910712219,17.164755336083,6.24278770419385));
#39201=CARTESIAN_POINT('Ctrl Pts',(-18.0129906098694,17.1652517940787,6.24288572247734));
#39202=CARTESIAN_POINT('Ctrl Pts',(-18.012888834453,17.1657481486638,6.24298372034392));
#39203=CARTESIAN_POINT('Ctrl Pts',(-18.0127857420086,17.1662443996692,6.24308169776025));
#39204=CARTESIAN_POINT('Ctrl Pts',(-18.0119023898804,17.1704965481556,6.24392122154546));
#39205=CARTESIAN_POINT('Ctrl Pts',(-18.01092307448,17.1747382382048,6.24475868046705));
#39206=CARTESIAN_POINT('Ctrl Pts',(-18.0098438883496,17.1789775150786,6.24559566294285));
#39207=CARTESIAN_POINT('Ctrl Pts',(-18.0097181622568,17.1794713944035,6.24569317210597));
#39208=CARTESIAN_POINT('Ctrl Pts',(-18.0095911499154,17.1799649488279,6.24579061712228));
#39209=CARTESIAN_POINT('Ctrl Pts',(-18.0094628549034,17.1804581707779,6.24588799649643));
#39210=CARTESIAN_POINT('Ctrl Pts',(-18.0083614518184,17.184692444338,6.246723991142));
#39211=CARTESIAN_POINT('Ctrl Pts',(-18.0071692721591,17.1888882609517,6.2475523930327));
#39212=CARTESIAN_POINT('Ctrl Pts',(-18.005888759018,17.1930435737714,6.24837279804873));
#39213=CARTESIAN_POINT('Ctrl Pts',(-18.005739794034,17.1935269706909,6.24846823761601));
#39214=CARTESIAN_POINT('Ctrl Pts',(-18.0055896174112,17.1940098841075,6.24856358172282));
#39215=CARTESIAN_POINT('Ctrl Pts',(-18.0054382246546,17.1944923306919,6.24865883366051));
#39216=CARTESIAN_POINT('Ctrl Pts',(-18.0026835667137,17.2032706589575,6.25039198465394));
#39217=CARTESIAN_POINT('Ctrl Pts',(-17.9995320635773,17.2118760854732,6.25209099875588));
#39218=CARTESIAN_POINT('Ctrl Pts',(-17.9959915059306,17.2203120171548,6.2537565486114));
#39219=CARTESIAN_POINT('Ctrl Pts',(-17.9920630646076,17.2296721422883,6.2556045667856));
#39220=CARTESIAN_POINT('Ctrl Pts',(-17.9876590484585,17.2388253614501,6.25741173443796));
#39221=CARTESIAN_POINT('Ctrl Pts',(-17.9827682254716,17.2477663515645,6.25917700060597));
#39222=CARTESIAN_POINT('Ctrl Pts',(-17.978358783995,17.2558273205992,6.26076851963648));
#39223=CARTESIAN_POINT('Ctrl Pts',(-17.9735560484698,17.263712298677,6.26232529185723));
#39224=CARTESIAN_POINT('Ctrl Pts',(-17.9683445575794,17.2714279183298,6.26384862676358));
#39225=CARTESIAN_POINT('Ctrl Pts',(-17.9680609879744,17.2718477435321,6.2639315150362));
#39226=CARTESIAN_POINT('Ctrl Pts',(-17.9677764219516,17.272266728987,6.26401423751312));
#39227=CARTESIAN_POINT('Ctrl Pts',(-17.9674908612731,17.2726848753105,6.26409679431597));
#39228=CARTESIAN_POINT('Ctrl Pts',(-17.962241876116,17.2803709610012,6.26561429817859));
#39229=CARTESIAN_POINT('Ctrl Pts',(-17.9566686125952,17.287757411178,6.26707264344373));
#39230=CARTESIAN_POINT('Ctrl Pts',(-17.9507822138997,17.2948520727703,6.26847337937143));
#39231=CARTESIAN_POINT('Ctrl Pts',(-17.9504629875019,17.2952368247013,6.26854934294571));
#39232=CARTESIAN_POINT('Ctrl Pts',(-17.9501428289144,17.295620732202,6.26862513979976));
#39233=CARTESIAN_POINT('Ctrl Pts',(-17.9498217365886,17.2960037971992,6.26870077031396));
#39234=CARTESIAN_POINT('Ctrl Pts',(-17.9439000104084,17.3030684506987,6.27009558158786));
#39235=CARTESIAN_POINT('Ctrl Pts',(-17.9376641923768,17.3098425498617,6.27143302720835));
#39236=CARTESIAN_POINT('Ctrl Pts',(-17.9311160363576,17.3163270111148,6.27271328811027));
#39237=CARTESIAN_POINT('Ctrl Pts',(-17.9242125826885,17.3231633139913,6.27406301493335));
#39238=CARTESIAN_POINT('Ctrl Pts',(-17.9169620149873,17.3296777303634,6.27534919003014));
#39239=CARTESIAN_POINT('Ctrl Pts',(-17.9093564103244,17.3358620845237,6.27657019922831));
#39240=CARTESIAN_POINT('Ctrl Pts',(-17.9089677439614,17.3361781212552,6.27663259600348));
#39241=CARTESIAN_POINT('Ctrl Pts',(-17.9085781282527,17.33649330971,6.27669482529897));
#39242=CARTESIAN_POINT('Ctrl Pts',(-17.9081875674216,17.3368076431069,6.27675688577594));
#39243=CARTESIAN_POINT('Ctrl Pts',(-17.9047568553611,17.3395687683655,6.27730202909254));
#39244=CARTESIAN_POINT('Ctrl Pts',(-17.9012526549201,17.3422643567528,6.27783423312387));
#39245=CARTESIAN_POINT('Ctrl Pts',(-17.8976780873748,17.3448896272997,6.27835255393837));
#39246=CARTESIAN_POINT('Ctrl Pts',(-17.8972718062779,17.3451880124286,6.27841146566585));
#39247=CARTESIAN_POINT('Ctrl Pts',(-17.8968649183223,17.3454852683764,6.27847015445325));
#39248=CARTESIAN_POINT('Ctrl Pts',(-17.8964574268529,17.3457813960457,6.27852862047875));
#39249=CARTESIAN_POINT('Ctrl Pts',(-17.8928715423093,17.3483872901855,6.27904311570846));
#39250=CARTESIAN_POINT('Ctrl Pts',(-17.8892395463305,17.3509051559847,6.27954023104512));
#39251=CARTESIAN_POINT('Ctrl Pts',(-17.8855625443911,17.3533364734939,6.28002025870288));
#39252=CARTESIAN_POINT('Ctrl Pts',(-17.8851453833495,17.3536123098849,6.28007471851579));
#39253=CARTESIAN_POINT('Ctrl Pts',(-17.8847276428159,17.3538870458274,6.28012896106144));
#39254=CARTESIAN_POINT('Ctrl Pts',(-17.884309321612,17.3541606824097,6.28018298655469));
#39255=CARTESIAN_POINT('Ctrl Pts',(-17.8760982231813,17.3595318108423,6.28124343636894));
#39256=CARTESIAN_POINT('Ctrl Pts',(-17.8676653792537,17.3644784082662,6.28222006881877));
#39257=CARTESIAN_POINT('Ctrl Pts',(-17.8590112984533,17.3690021459286,6.28311321386716));
#39258=CARTESIAN_POINT('Ctrl Pts',(-17.8507952450643,17.373296914028,6.28396115226419));
#39259=CARTESIAN_POINT('Ctrl Pts',(-17.8423802671056,17.3772106561903,6.28473386272934));
#39260=CARTESIAN_POINT('Ctrl Pts',(-17.8337665264467,17.3807441488957,6.28543149856692));
#39261=CARTESIAN_POINT('Ctrl Pts',(-17.8333072968939,17.3809325321242,6.28546869204724));
#39262=CARTESIAN_POINT('Ctrl Pts',(-17.8328474973904,17.3811198248295,6.2855056702199));
#39263=CARTESIAN_POINT('Ctrl Pts',(-17.8323871269169,17.3813060250783,6.28554243270319));
#39264=CARTESIAN_POINT('Ctrl Pts',(-17.8282990371385,17.382959483277,6.28586888355269));
#39265=CARTESIAN_POINT('Ctrl Pts',(-17.8241650495164,17.3845273373272,6.28617843313006));
#39266=CARTESIAN_POINT('Ctrl Pts',(-17.8199872841232,17.3860072533335,6.28647062064218));
#39267=CARTESIAN_POINT('Ctrl Pts',(-17.819517535096,17.3861736554741,6.28650347428202));
#39268=CARTESIAN_POINT('Ctrl Pts',(-17.8190471432221,17.3863389729831,6.28653611377741));
#39269=CARTESIAN_POINT('Ctrl Pts',(-17.8185761407676,17.3865031933171,6.28656853665184));
#39270=CARTESIAN_POINT('Ctrl Pts',(-17.8143864015698,17.3879639932853,6.28685694998517));
#39271=CARTESIAN_POINT('Ctrl Pts',(-17.8101435756898,17.3893394993071,6.28712852329117));
#39272=CARTESIAN_POINT('Ctrl Pts',(-17.8058709862739,17.3906204723322,6.28738143245607));
#39273=CARTESIAN_POINT('Ctrl Pts',(-17.8053915126047,17.3907642242298,6.28740981414068));
#39274=CARTESIAN_POINT('Ctrl Pts',(-17.8049118810369,17.3909067288397,6.28743794956678));
#39275=CARTESIAN_POINT('Ctrl Pts',(-17.8044320969961,17.3910479869729,6.2874658388945));
#39276=CARTESIAN_POINT('Ctrl Pts',(-17.7954000423655,17.3937072066784,6.28799086246787));
#39277=CARTESIAN_POINT('Ctrl Pts',(-17.78630765222,17.3959264977103,6.28842902863579));
#39278=CARTESIAN_POINT('Ctrl Pts',(-17.7771567393255,17.397719289795,6.2887829888989));
#39279=CARTESIAN_POINT('Ctrl Pts',(-17.7670367925117,17.3997019292053,6.28917443170665));
#39280=CARTESIAN_POINT('Ctrl Pts',(-17.7568457798152,17.4011666604281,6.289463621208));
#39281=CARTESIAN_POINT('Ctrl Pts',(-17.7465828115781,17.4021072682102,6.28964933029322));
#39282=CARTESIAN_POINT('Ctrl Pts',(-17.7372993592615,17.4029581027146,6.28981731497344));
#39283=CARTESIAN_POINT('Ctrl Pts',(-17.7279574142293,17.4033800700187,6.28990062617237));
#39284=CARTESIAN_POINT('Ctrl Pts',(-17.7185558210734,17.4033686132305,6.2898983641991));
#39285=CARTESIAN_POINT('Ctrl Pts',(-17.7180614574138,17.4033680107986,6.28989824525784));
#39286=CARTESIAN_POINT('Ctrl Pts',(-17.7175669272791,17.4033661986565,6.28989788747721));
#39287=CARTESIAN_POINT('Ctrl Pts',(-17.7170722302065,17.4033631739899,6.28989729030154));
#39288=CARTESIAN_POINT('Ctrl Pts',(-17.7150908610137,17.4033510595431,6.28989489848333));
#39289=CARTESIAN_POINT('Ctrl Pts',(-17.713106823896,17.4033194963692,6.28988866680177));
#39290=CARTESIAN_POINT('Ctrl Pts',(-17.7111200943939,17.4032683024772,6.28987855932548));
#39291=CARTESIAN_POINT('Ctrl Pts',(-17.7086373297241,17.4032043267893,6.28986592827277));
#39292=CARTESIAN_POINT('Ctrl Pts',(-17.7061493206867,17.4031095514149,6.28984721627779));
#39293=CARTESIAN_POINT('Ctrl Pts',(-17.7036711651943,17.4029846303786,6.28982255246806));
#39294=CARTESIAN_POINT('Ctrl Pts',(-17.7031768681837,17.4029597134212,6.2898176329836));
#39295=CARTESIAN_POINT('Ctrl Pts',(-17.7026828252418,17.4029335955226,6.28981247639108));
#39296=CARTESIAN_POINT('Ctrl Pts',(-17.7021890358816,17.4029062789949,6.28980708314698));
#39297=CARTESIAN_POINT('Ctrl Pts',(-17.6977316048652,17.4026596930054,6.28975839839293));
#39298=CARTESIAN_POINT('Ctrl Pts',(-17.6932948233157,17.4023154871287,6.28969044003697));
#39299=CARTESIAN_POINT('Ctrl Pts',(-17.6888783478203,17.4018753094736,6.28960353347377));
#39300=CARTESIAN_POINT('Ctrl Pts',(-17.688389904011,17.4018266276569,6.28959392196956));
#39301=CARTESIAN_POINT('Ctrl Pts',(-17.6879017081709,17.4017767739381,6.28958407909064));
#39302=CARTESIAN_POINT('Ctrl Pts',(-17.6874137601304,17.4017257492013,6.28957400501155));
#39303=CARTESIAN_POINT('Ctrl Pts',(-17.6781002074841,17.4007518308069,6.28938171923894));
#39304=CARTESIAN_POINT('Ctrl Pts',(-17.66887685941,17.3993514864911,6.28910524197941));
#39305=CARTESIAN_POINT('Ctrl Pts',(-17.6597422801017,17.397531513091,6.28874591516785));
#39306=CARTESIAN_POINT('Ctrl Pts',(-17.6501291359109,17.3956161904332,6.28836776305657));
#39307=CARTESIAN_POINT('Ctrl Pts',(-17.6406143081556,17.3932361045023,6.28789785031569));
#39308=CARTESIAN_POINT('Ctrl Pts',(-17.6311990050655,17.3903855899544,6.28733505840692));
#39309=CARTESIAN_POINT('Ctrl Pts',(-17.6307333868561,17.3902446224819,6.28730722646584));
#39310=CARTESIAN_POINT('Ctrl Pts',(-17.6302680124599,17.3901025025716,6.28727916699298));
#39311=CARTESIAN_POINT('Ctrl Pts',(-17.6298028822972,17.3899592282443,6.28725087959758));
#39312=CARTESIAN_POINT('Ctrl Pts',(-17.6255653243114,17.3886539306776,6.28699316791192));
#39313=CARTESIAN_POINT('Ctrl Pts',(-17.6213472115623,17.3872525326915,6.2867164826208));
#39314=CARTESIAN_POINT('Ctrl Pts',(-17.6171512211235,17.3857544345316,6.28642070531156));
#39315=CARTESIAN_POINT('Ctrl Pts',(-17.6166913908926,17.3855902609395,6.28638829166563));
#39316=CARTESIAN_POINT('Ctrl Pts',(-17.6162317405224,17.3854248853256,6.2863556406983));
#39317=CARTESIAN_POINT('Ctrl Pts',(-17.6157723292095,17.3852583310309,6.28632275701788));
#39318=CARTESIAN_POINT('Ctrl Pts',(-17.611579352614,17.3837382155269,6.28602263270991));
#39319=CARTESIAN_POINT('Ctrl Pts',(-17.6074023369311,17.3821183117921,6.28570280669268));
#39320=CARTESIAN_POINT('Ctrl Pts',(-17.6032870770419,17.380416304936,6.28536677062928));
#39321=CARTESIAN_POINT('Ctrl Pts',(-17.6028369747322,17.38023014969,6.28533001703112));
#39322=CARTESIAN_POINT('Ctrl Pts',(-17.6023875004942,17.3800429894745,6.28529306501661));
#39323=CARTESIAN_POINT('Ctrl Pts',(-17.6019386577086,17.379854826811,6.28525591508357));
#39324=CARTESIAN_POINT('Ctrl Pts',(-17.5928334838723,17.3760377803621,6.28450229575596));
#39325=CARTESIAN_POINT('Ctrl Pts',(-17.5839822725707,17.3718062598322,6.28366684465546));
#39326=CARTESIAN_POINT('Ctrl Pts',(-17.5753808547761,17.3671661414509,6.28275072195659));
#39327=CARTESIAN_POINT('Ctrl Pts',(-17.5672010821262,17.3627534836386,6.28187950798057));
#39328=CARTESIAN_POINT('Ctrl Pts',(-17.5592466988203,17.3579709628613,6.28093527003623));
#39329=CARTESIAN_POINT('Ctrl Pts',(-17.551515652032,17.3528245952513,6.27991919591984));
#39330=CARTESIAN_POINT('Ctrl Pts',(-17.54338434228,17.3474117824355,6.27885051614107));
#39331=CARTESIAN_POINT('Ctrl Pts',(-17.5355018854376,17.3415935456519,6.27770179140026));
#39332=CARTESIAN_POINT('Ctrl Pts',(-17.527876561236,17.3353594564721,6.27647096275861));
#39333=CARTESIAN_POINT('Ctrl Pts',(-17.527504484612,17.3350552649658,6.27641090464783));
#39334=CARTESIAN_POINT('Ctrl Pts',(-17.5271329362737,17.3347500052773,6.27635063564029));
#39335=CARTESIAN_POINT('Ctrl Pts',(-17.5267620036043,17.3344437506483,6.27629017019649));
#39336=CARTESIAN_POINT('Ctrl Pts',(-17.5252323697242,17.3331808328872,6.27604082577622));
#39337=CARTESIAN_POINT('Ctrl Pts',(-17.5237128212741,17.3319006630474,6.27578807518837));
#39338=CARTESIAN_POINT('Ctrl Pts',(-17.5222096817844,17.3306085300547,6.27553296265302));
#39339=CARTESIAN_POINT('Ctrl Pts',(-17.5203423804563,17.329003355239,6.27521604464285));
#39340=CARTESIAN_POINT('Ctrl Pts',(-17.5184987822701,17.3273784795521,6.27489523698725));
#39341=CARTESIAN_POINT('Ctrl Pts',(-17.5166789587972,17.3257344763096,6.2745706528789));
#39342=CARTESIAN_POINT('Ctrl Pts',(-17.5163243493235,17.3254141270376,6.27450740465644));
#39343=CARTESIAN_POINT('Ctrl Pts',(-17.5159706422872,17.3250930517187,6.27444401308677));
#39344=CARTESIAN_POINT('Ctrl Pts',(-17.5156178386202,17.3247712542517,6.27438047893964));
#39345=CARTESIAN_POINT('Ctrl Pts',(-17.5123492315953,17.3217899092154,6.2737918564873));
#39346=CARTESIAN_POINT('Ctrl Pts',(-17.5091574796189,17.3187456886125,6.27319082018488));
#39347=CARTESIAN_POINT('Ctrl Pts',(-17.5060413667377,17.3156395916544,6.2725775673119));
#39348=CARTESIAN_POINT('Ctrl Pts',(-17.5057055852483,17.3153048894461,6.27251148531459));
#39349=CARTESIAN_POINT('Ctrl Pts',(-17.5053706742823,17.3149694751014,6.2724452627165));
#39350=CARTESIAN_POINT('Ctrl Pts',(-17.50503663389,17.3146333485789,6.27237889950942));
#39351=CARTESIAN_POINT('Ctrl Pts',(-17.4981686427345,17.3077224658295,6.27101444799423));
#39352=CARTESIAN_POINT('Ctrl Pts',(-17.4916683867703,17.3005107152883,6.26959059458653));
#39353=CARTESIAN_POINT('Ctrl Pts',(-17.4855366603079,17.2929973081219,6.26810718354282));
#39354=CARTESIAN_POINT('Ctrl Pts',(-17.4797011422079,17.2858468548555,6.26669543237481));
#39355=CARTESIAN_POINT('Ctrl Pts',(-17.4741996148819,17.2784234803524,6.26522979694795));
#39356=CARTESIAN_POINT('Ctrl Pts',(-17.4690325144084,17.2707263188011,6.26371010632058));
#39357=CARTESIAN_POINT('Ctrl Pts',(-17.4687702346341,17.2703356142262,6.26363296748483));
#39358=CARTESIAN_POINT('Ctrl Pts',(-17.468508824208,17.2699441979455,6.26355568813333));
#39359=CARTESIAN_POINT('Ctrl Pts',(-17.4682482847578,17.2695520685622,6.26347826799026));
#39360=CARTESIAN_POINT('Ctrl Pts',(-17.4658117031665,17.2658848495045,6.26275422986355));
#39361=CARTESIAN_POINT('Ctrl Pts',(-17.4634512948009,17.2621553054514,6.26201788658893));
#39362=CARTESIAN_POINT('Ctrl Pts',(-17.4611684259367,17.2583623237431,6.2612690184882));
#39363=CARTESIAN_POINT('Ctrl Pts',(-17.458641452522,17.2541637628493,6.26044007478003));
#39364=CARTESIAN_POINT('Ctrl Pts',(-17.4562225545235,17.2499084715741,6.2595999304977));
#39365=CARTESIAN_POINT('Ctrl Pts',(-17.453921204761,17.2456173631331,6.25875271464607));
#39366=CARTESIAN_POINT('Ctrl Pts',(-17.4536996553159,17.2452042609139,6.25867115372695));
#39367=CARTESIAN_POINT('Ctrl Pts',(-17.4534791583449,17.2447907694999,6.25858951596709));
#39368=CARTESIAN_POINT('Ctrl Pts',(-17.453259712687,17.2443768893244,6.25850780145202));
#39369=CARTESIAN_POINT('Ctrl Pts',(-17.4489201906875,17.2361924388161,6.25689190283213));
#39370=CARTESIAN_POINT('Ctrl Pts',(-17.4449915782234,17.22785591363,6.25524597931787));
#39371=CARTESIAN_POINT('Ctrl Pts',(-17.4414648184729,17.2193708249878,6.25357072414803));
#39372=CARTESIAN_POINT('Ctrl Pts',(-17.4377596760485,17.2104565625692,6.25181073496798));
#39373=CARTESIAN_POINT('Ctrl Pts',(-17.434498115918,17.2013783091928,6.25001836820042));
#39374=CARTESIAN_POINT('Ctrl Pts',(-17.4316824779197,17.1921354103922,6.24819349463067));
#39375=CARTESIAN_POINT('Ctrl Pts',(-17.4315478755021,17.1916935508474,6.24810625600323));
#39376=CARTESIAN_POINT('Ctrl Pts',(-17.431414290673,17.1912513087585,6.24801894184813));
#39377=CARTESIAN_POINT('Ctrl Pts',(-17.4312817253082,17.1908086844359,6.24793155222665));
#39378=CARTESIAN_POINT('Ctrl Pts',(-17.4298954472664,17.1861800215884,6.24701769125339));
#39379=CARTESIAN_POINT('Ctrl Pts',(-17.4286207447609,17.1815100802888,6.24609568046068));
#39380=CARTESIAN_POINT('Ctrl Pts',(-17.4274595038986,17.1767981983333,6.24516538910623));
#39381=CARTESIAN_POINT('Ctrl Pts',(-17.4264089791608,17.1725355610832,6.24432379446985));
#39382=CARTESIAN_POINT('Ctrl Pts',(-17.4254503111968,17.1682336230582,6.24347444047714));
#39383=CARTESIAN_POINT('Ctrl Pts',(-17.4245878781802,17.16390605946,6.24262002709426));
#39384=CARTESIAN_POINT('Ctrl Pts',(-36.918942728626,17.5305480494939,-3.00047863991406));
#39385=CARTESIAN_POINT('Ctrl Pts',(-36.9184636408495,17.5305448701384,-2.5));
#39386=CARTESIAN_POINT('Ctrl Pts',(-37.418931489881,17.5338661095488,-2.5));
#39387=CARTESIAN_POINT('Ctrl Pts',(-36.918766523927,17.5567617326884,-2.99813492793641));
#39388=CARTESIAN_POINT('Ctrl Pts',(-36.9206303865991,17.5567282897711,-2.5));
#39389=CARTESIAN_POINT('Ctrl Pts',(-37.4188654127938,17.5438230235078,-2.5));
#39390=CARTESIAN_POINT('Ctrl Pts',(-36.9198840261816,17.5827769733229,-2.99578898700793));
#39391=CARTESIAN_POINT('Ctrl Pts',(-36.9240615386413,17.5825477668969,-2.5));
#39392=CARTESIAN_POINT('Ctrl Pts',(-37.4192844801969,17.5537061882809,-2.5));
#39393=CARTESIAN_POINT('Ctrl Pts',(-36.9246169309371,17.6343825999131,-2.99109602673912));
#39394=CARTESIAN_POINT('Ctrl Pts',(-36.9333093941054,17.6333273268776,-2.5));
#39395=CARTESIAN_POINT('Ctrl Pts',(-37.4210593120151,17.5733143538484,-2.5));
#39396=CARTESIAN_POINT('Ctrl Pts',(-36.9282325359345,17.6599800335755,-2.98874837352374));
#39397=CARTESIAN_POINT('Ctrl Pts',(-36.9391161778231,17.6582989890867,-2.5));
#39398=CARTESIAN_POINT('Ctrl Pts',(-37.4224151662337,17.5830420307807,-2.5));
#39399=CARTESIAN_POINT('Ctrl Pts',(-36.9379460863992,17.710766834452,-2.98405135826386));
#39400=CARTESIAN_POINT('Ctrl Pts',(-36.9530417639778,17.7074272412772,-2.5));
#39401=CARTESIAN_POINT('Ctrl Pts',(-37.4260577504339,17.6023455517275,-2.5));
#39402=CARTESIAN_POINT('Ctrl Pts',(-36.9440439356691,17.7359562130125,-2.98170199150478));
#39403=CARTESIAN_POINT('Ctrl Pts',(-36.961150208635,17.7315882072703,-2.5));
#39404=CARTESIAN_POINT('Ctrl Pts',(-37.4283444361295,17.6119214029654,-2.5));
#39405=CARTESIAN_POINT('Ctrl Pts',(-36.9550940181883,17.7734276473997,-2.97817796458518));
#39406=CARTESIAN_POINT('Ctrl Pts',(-36.9750602300798,17.7672721065816,-2.5));
#39407=CARTESIAN_POINT('Ctrl Pts',(-37.4324882266632,17.6261687598122,-2.5));
#39408=CARTESIAN_POINT('Ctrl Pts',(-36.9590977423692,17.7858733013829,-2.97700260220075));
#39409=CARTESIAN_POINT('Ctrl Pts',(-36.9799820522302,17.7790613692586,-2.5));
#39410=CARTESIAN_POINT('Ctrl Pts',(-37.4339896230655,17.6309012462933,-2.5));
#39411=CARTESIAN_POINT('Ctrl Pts',(-36.9677444087214,17.8106277669609,-2.97465510692309));
#39412=CARTESIAN_POINT('Ctrl Pts',(-36.9903966889781,17.8024136686443,-2.5));
#39413=CARTESIAN_POINT('Ctrl Pts',(-37.437232116886,17.6403150006157,-2.5));
#39414=CARTESIAN_POINT('Ctrl Pts',(-36.9723569013568,17.8228504435788,-2.97349114599914));
#39415=CARTESIAN_POINT('Ctrl Pts',(-36.9958519245572,17.8138964486576,-2.5));
#39416=CARTESIAN_POINT('Ctrl Pts',(-37.4389618074377,17.6449635078328,-2.5));
#39417=CARTESIAN_POINT('Ctrl Pts',(-36.9968316404772,17.8831937506765,-2.96772154502321));
#39418=CARTESIAN_POINT('Ctrl Pts',(-37.0242345246282,17.8701746208594,-2.5));
#39419=CARTESIAN_POINT('Ctrl Pts',(-37.4481398206947,17.6679151360551,-2.5));
#39420=CARTESIAN_POINT('Ctrl Pts',(-37.0208955392833,17.9290397288272,-2.96326313438592));
#39421=CARTESIAN_POINT('Ctrl Pts',(-37.0507916007085,17.9123870158746,-2.5));
#39422=CARTESIAN_POINT('Ctrl Pts',(-37.4571637864037,17.6853590086553,-2.5));
#39423=CARTESIAN_POINT('Ctrl Pts',(-37.0636620936595,17.9942014163556,-2.95683590040463));
#39424=CARTESIAN_POINT('Ctrl Pts',(-37.0962159645972,17.9716354404605,-2.5));
#39425=CARTESIAN_POINT('Ctrl Pts',(-37.4732012555054,17.7101600273524,-2.5));
#39426=CARTESIAN_POINT('Ctrl Pts',(-37.0790511866489,18.0153339916105,-2.95473552840589));
#39427=CARTESIAN_POINT('Ctrl Pts',(-37.1122588011471,17.9906733177174,-2.5));
#39428=CARTESIAN_POINT('Ctrl Pts',(-37.4789721679196,17.7182046074472,-2.5));
#39429=CARTESIAN_POINT('Ctrl Pts',(-37.1121011063091,18.0562700748877,-2.95063882870761));
#39430=CARTESIAN_POINT('Ctrl Pts',(-37.1461872334036,18.0272996809472,-2.5));
#39431=CARTESIAN_POINT('Ctrl Pts',(-37.4913658752322,17.733790264152,-2.5));
#39432=CARTESIAN_POINT('Ctrl Pts',(-37.1295103581676,18.0757653348942,-2.94867340342006));
#39433=CARTESIAN_POINT('Ctrl Pts',(-37.1638134804818,18.0446236356694,-2.5));
#39434=CARTESIAN_POINT('Ctrl Pts',(-37.4978943532022,17.7412139562433,-2.5));
#39435=CARTESIAN_POINT('Ctrl Pts',(-37.1843057553075,18.1314233942583,-2.94302770433399));
#39436=CARTESIAN_POINT('Ctrl Pts',(-37.2185148052678,18.0936922878623,-2.5));
#39437=CARTESIAN_POINT('Ctrl Pts',(-37.5184426204004,17.7624112761694,-2.5));
#39438=CARTESIAN_POINT('Ctrl Pts',(-37.2242361969918,18.1647864737446,-2.93959528754205));
#39439=CARTESIAN_POINT('Ctrl Pts',(-37.2575873678388,18.1227938260313,-2.5));
#39440=CARTESIAN_POINT('Ctrl Pts',(-37.5334165320212,17.7751217694643,-2.5));
#39441=CARTESIAN_POINT('Ctrl Pts',(-37.278501267837,18.2017080527822,-2.93576187067611));
#39442=CARTESIAN_POINT('Ctrl Pts',(-37.3098415222596,18.154743770369,-2.5));
#39443=CARTESIAN_POINT('Ctrl Pts',(-37.5537659442094,17.7891910078983,-2.5));
#39444=CARTESIAN_POINT('Ctrl Pts',(-37.2895908939828,18.2088614252754,-2.9350171685076));
#39445=CARTESIAN_POINT('Ctrl Pts',(-37.3204553852497,18.1609059986669,-2.5));
#39446=CARTESIAN_POINT('Ctrl Pts',(-37.5579245541323,17.7919170308987,-2.5));
#39447=CARTESIAN_POINT('Ctrl Pts',(-37.3121456740118,18.222628713375,-2.93358056573866));
#39448=CARTESIAN_POINT('Ctrl Pts',(-37.3419594345533,18.1727383129417,-2.5));
#39449=CARTESIAN_POINT('Ctrl Pts',(-37.5663825921581,17.7971638038772,-2.5));
#39450=CARTESIAN_POINT('Ctrl Pts',(-37.3235504689819,18.2292070024891,-2.93289238561845));
#39451=CARTESIAN_POINT('Ctrl Pts',(-37.3527929576584,18.1783789941509,-2.5));
#39452=CARTESIAN_POINT('Ctrl Pts',(-37.5706593939047,17.7996709619125,-2.5));
#39453=CARTESIAN_POINT('Ctrl Pts',(-37.3581397345302,18.2480437180578,-2.93091764257171));
#39454=CARTESIAN_POINT('Ctrl Pts',(-37.3855178350711,18.1944875128524,-2.5));
#39455=CARTESIAN_POINT('Ctrl Pts',(-37.5836303643146,17.8068505202015,-2.5));
#39456=CARTESIAN_POINT('Ctrl Pts',(-37.3816981781207,18.2594061256977,-2.92972067272748));
#39457=CARTESIAN_POINT('Ctrl Pts',(-37.4076765730136,18.2041692805068,-2.5));
#39458=CARTESIAN_POINT('Ctrl Pts',(-37.5924647836065,17.811181769741,-2.5));
#39459=CARTESIAN_POINT('Ctrl Pts',(-37.4297964715305,18.2797809159781,-2.92756741754469));
#39460=CARTESIAN_POINT('Ctrl Pts',(-37.4526661261266,18.2214705311287,-2.5));
#39461=CARTESIAN_POINT('Ctrl Pts',(-37.6105016433052,17.8189490809156,-2.5));
#39462=CARTESIAN_POINT('Ctrl Pts',(-37.4543363298823,18.2887932678948,-2.92661112217483));
#39463=CARTESIAN_POINT('Ctrl Pts',(-37.4755052012686,18.2290974806186,-2.5));
#39464=CARTESIAN_POINT('Ctrl Pts',(-37.6197040888717,17.8223851300001,-2.5));
#39465=CARTESIAN_POINT('Ctrl Pts',(-37.4918913116176,18.3005282374446,-2.92536297515959));
#39466=CARTESIAN_POINT('Ctrl Pts',(-37.5103223388011,18.2390056374751,-2.5));
#39467=CARTESIAN_POINT('Ctrl Pts',(-37.633787209243,17.8268594543971,-2.5));
#39468=CARTESIAN_POINT('Ctrl Pts',(-37.5045340558524,18.3041421023044,-2.92497802297482));
#39469=CARTESIAN_POINT('Ctrl Pts',(-37.5220166849113,18.2420518473036,-2.5));
#39470=CARTESIAN_POINT('Ctrl Pts',(-37.6385282366181,17.8282374131812,-2.5));
#39471=CARTESIAN_POINT('Ctrl Pts',(-37.5236880380742,18.3091085696021,-2.92444842107095));
#39472=CARTESIAN_POINT('Ctrl Pts',(-37.5397059345923,18.2462341178242,-2.5));
#39473=CARTESIAN_POINT('Ctrl Pts',(-37.6457109814105,17.8301311528227,-2.5));
#39474=CARTESIAN_POINT('Ctrl Pts',(-37.530104354971,18.310688300037,-2.92427986194296));
#39475=CARTESIAN_POINT('Ctrl Pts',(-37.5456258343898,18.2475634797771,-2.5));
#39476=CARTESIAN_POINT('Ctrl Pts',(-37.6481170992389,17.8307335274115,-2.5));
#39477=CARTESIAN_POINT('Ctrl Pts',(-37.5430010389201,18.3136945178689,-2.9239589307846));
#39478=CARTESIAN_POINT('Ctrl Pts',(-37.5575155990342,18.2500919427414,-2.5));
#39479=CARTESIAN_POINT('Ctrl Pts',(-37.6529533567628,17.8318798449285,-2.5));
#39480=CARTESIAN_POINT('Ctrl Pts',(-37.5494894557846,18.3151225191071,-2.92380639706833));
#39481=CARTESIAN_POINT('Ctrl Pts',(-37.5634930070409,18.2512923999885,-2.5));
#39482=CARTESIAN_POINT('Ctrl Pts',(-37.6553865130038,17.8324243739287,-2.5));
#39483=CARTESIAN_POINT('Ctrl Pts',(-37.6078715508142,18.3272151542962,-2.92251412976417));
#39484=CARTESIAN_POINT('Ctrl Pts',(-37.6171933811497,18.261444733944,-2.5));
#39485=CARTESIAN_POINT('Ctrl Pts',(-37.6772797946946,17.8370356375276,-2.5));
#39486=CARTESIAN_POINT('Ctrl Pts',(-37.6600314084477,18.3327140130362,-2.92192313396902));
#39487=CARTESIAN_POINT('Ctrl Pts',(-37.6650031743221,18.2660494018553,-2.5));
#39488=CARTESIAN_POINT('Ctrl Pts',(-37.6968397447769,17.8391327868468,-2.5));
#39489=CARTESIAN_POINT('Ctrl Pts',(-37.7386551922739,18.3333477986367,-2.92185513454714));
#39490=CARTESIAN_POINT('Ctrl Pts',(-37.7369884997638,18.2665799642824,-2.5));
#39491=CARTESIAN_POINT('Ctrl Pts',(-37.7263236637676,17.8393744833388,-2.5));
#39492=CARTESIAN_POINT('Ctrl Pts',(-37.7649275847458,18.332280602678,-2.92196969819476));
#39493=CARTESIAN_POINT('Ctrl Pts',(-37.7610453062294,18.2656866234871,-2.5));
#39494=CARTESIAN_POINT('Ctrl Pts',(-37.7361758116312,17.8389674969796,-2.5));
#39495=CARTESIAN_POINT('Ctrl Pts',(-37.8044355425913,18.3287092953001,-2.9223525645861));
#39496=CARTESIAN_POINT('Ctrl Pts',(-37.7972513234411,18.2626950729203,-2.5));
#39497=CARTESIAN_POINT('Ctrl Pts',(-37.7509912947654,17.8376055413245,-2.5));
#39498=CARTESIAN_POINT('Ctrl Pts',(-37.8176556209491,18.3271839572083,-2.92251604054704));
#39499=CARTESIAN_POINT('Ctrl Pts',(-37.8093757241164,18.2614166995762,-2.5));
#39500=CARTESIAN_POINT('Ctrl Pts',(-37.7559488239131,17.8370238468006,-2.5));
#39501=CARTESIAN_POINT('Ctrl Pts',(-37.8438653515097,18.3235000632348,-2.92291055095015));
#39502=CARTESIAN_POINT('Ctrl Pts',(-37.8334337540048,18.2583273875558,-2.5));
#39503=CARTESIAN_POINT('Ctrl Pts',(-37.7657774740514,17.8356190137894,-2.5));
#39504=CARTESIAN_POINT('Ctrl Pts',(-37.8568746743686,18.321341537448,-2.92314158144293));
#39505=CARTESIAN_POINT('Ctrl Pts',(-37.8453867146324,18.256516085823,-2.5));
#39506=CARTESIAN_POINT('Ctrl Pts',(-37.7706559690046,17.8347958710238,-2.5));
#39507=CARTESIAN_POINT('Ctrl Pts',(-37.9214525991908,18.3089956020391,-2.92446167772975));
#39508=CARTESIAN_POINT('Ctrl Pts',(-37.9048311581349,18.2461405986857,-2.5));
#39509=CARTESIAN_POINT('Ctrl Pts',(-37.7948726934621,17.8300879827949,-2.5));
#39510=CARTESIAN_POINT('Ctrl Pts',(-37.971628515283,18.2941930137726,-2.92604160841261));
#39511=CARTESIAN_POINT('Ctrl Pts',(-37.951260778169,18.233665691823,-2.5));
#39512=CARTESIAN_POINT('Ctrl Pts',(-37.8136886637651,17.8244435332827,-2.5));
#39513=CARTESIAN_POINT('Ctrl Pts',(-38.0324952429552,18.2695437413729,-2.9286496092432));
#39514=CARTESIAN_POINT('Ctrl Pts',(-38.0080199920834,18.2127861786537,-2.5));
#39515=CARTESIAN_POINT('Ctrl Pts',(-37.8365136817825,17.8150464189915,-2.5));
#39516=CARTESIAN_POINT('Ctrl Pts',(-38.044575088039,18.264303794869,-2.92920311231327));
#39517=CARTESIAN_POINT('Ctrl Pts',(-38.0193295823946,18.208334158798,-2.5));
#39518=CARTESIAN_POINT('Ctrl Pts',(-37.8410436263355,17.8130488679072,-2.5));
#39519=CARTESIAN_POINT('Ctrl Pts',(-38.0685444585904,18.2531925029883,-2.93037437162195));
#39520=CARTESIAN_POINT('Ctrl Pts',(-38.0418344218168,18.1988760473144,-2.5));
#39521=CARTESIAN_POINT('Ctrl Pts',(-37.850032136943,17.8088132624928,-2.5));
#39522=CARTESIAN_POINT('Ctrl Pts',(-38.0804306041699,18.2473200654554,-2.93099223718261));
#39523=CARTESIAN_POINT('Ctrl Pts',(-38.0530277696176,18.1938679552602,-2.5));
#39524=CARTESIAN_POINT('Ctrl Pts',(-37.8544894413598,17.8065748058377,-2.5));
#39525=CARTESIAN_POINT('Ctrl Pts',(-38.1154058739446,18.2289535054552,-2.93292028761117));
#39526=CARTESIAN_POINT('Ctrl Pts',(-38.0860884329982,18.1781636427194,-2.5));
#39527=CARTESIAN_POINT('Ctrl Pts',(-37.8676051730758,17.7995742349009,-2.5));
#39528=CARTESIAN_POINT('Ctrl Pts',(-38.1379498775984,18.2156512801827,-2.93431116406502));
#39529=CARTESIAN_POINT('Ctrl Pts',(-38.107532686332,18.1667488029368,-2.5));
#39530=CARTESIAN_POINT('Ctrl Pts',(-37.8760591693826,17.7945044510302,-2.5));
#39531=CARTESIAN_POINT('Ctrl Pts',(-38.2033280576451,18.17265741314,-2.93878236806526));
#39532=CARTESIAN_POINT('Ctrl Pts',(-38.1702794467489,18.1296291178422,-2.5));
#39533=CARTESIAN_POINT('Ctrl Pts',(-37.9005759909892,17.7781206666248,-2.5));
#39534=CARTESIAN_POINT('Ctrl Pts',(-38.2439301407294,18.1399084455847,-2.94215865140722));
#39535=CARTESIAN_POINT('Ctrl Pts',(-38.2098765411374,18.1011163150348,-2.5));
#39536=CARTESIAN_POINT('Ctrl Pts',(-37.9158017810326,17.7656435334912,-2.5));
#39537=CARTESIAN_POINT('Ctrl Pts',(-38.2908370693989,18.0936969886663,-2.94685549765066));
#39538=CARTESIAN_POINT('Ctrl Pts',(-38.2564928085569,18.0604885105553,-2.5));
#39539=CARTESIAN_POINT('Ctrl Pts',(-37.9333918647676,17.7480431201017,-2.5));
#39540=CARTESIAN_POINT('Ctrl Pts',(-38.2999735282245,18.0842373184233,-2.94781393656573));
#39541=CARTESIAN_POINT('Ctrl Pts',(-38.2656503724343,18.0521248196139,-2.5));
#39542=CARTESIAN_POINT('Ctrl Pts',(-37.9368180370691,17.744440511481,-2.5));
#39543=CARTESIAN_POINT('Ctrl Pts',(-38.3176873507553,18.0649722522993,-2.94975921175979));
#39544=CARTESIAN_POINT('Ctrl Pts',(-38.2835158468797,18.035036707545,-2.5));
#39545=CARTESIAN_POINT('Ctrl Pts',(-37.9434607258409,17.7371042069719,-2.5));
#39546=CARTESIAN_POINT('Ctrl Pts',(-38.3262776360071,18.0551541758763,-2.95074733976652));
#39547=CARTESIAN_POINT('Ctrl Pts',(-38.292236426,18.0262999067001,-2.5));
#39548=CARTESIAN_POINT('Ctrl Pts',(-37.9466820784148,17.7333656728621,-2.5));
#39549=CARTESIAN_POINT('Ctrl Pts',(-38.3512613834271,18.0251519219321,-2.95375629684687));
#39550=CARTESIAN_POINT('Ctrl Pts',(-38.3177954315766,17.9994877930366,-2.5));
#39551=CARTESIAN_POINT('Ctrl Pts',(-37.9560509888996,17.721942323421,-2.5));
#39552=CARTESIAN_POINT('Ctrl Pts',(-38.3668695803311,18.0044210131818,-2.95582157994119));
#39553=CARTESIAN_POINT('Ctrl Pts',(-38.3339844060987,17.9808535987548,-2.5));
#39554=CARTESIAN_POINT('Ctrl Pts',(-37.9619040598854,17.7140502257561,-2.5));
#39555=CARTESIAN_POINT('Ctrl Pts',(-38.3960122766866,17.96151412598,-2.96006384799544));
#39556=CARTESIAN_POINT('Ctrl Pts',(-38.3647032001448,17.9420087393569,-2.5));
#39557=CARTESIAN_POINT('Ctrl Pts',(-37.9728325697887,17.6977186737315,-2.5));
#39558=CARTESIAN_POINT('Ctrl Pts',(-38.4095468146066,17.9393381811376,-2.96224084544494));
#39559=CARTESIAN_POINT('Ctrl Pts',(-38.3792301089262,17.921787539762,-2.5));
#39560=CARTESIAN_POINT('Ctrl Pts',(-37.9779080274105,17.6892792325375,-2.5));
#39561=CARTESIAN_POINT('Ctrl Pts',(-38.4282645108262,17.904969535058,-2.96558787871309));
#39562=CARTESIAN_POINT('Ctrl Pts',(-38.399714653804,17.8902405113807,-2.5));
#39563=CARTESIAN_POINT('Ctrl Pts',(-37.9849271555627,17.6762019272695,-2.5));
#39564=CARTESIAN_POINT('Ctrl Pts',(-38.4342446366122,17.89331766282,-2.96671826104229));
#39565=CARTESIAN_POINT('Ctrl Pts',(-38.4063407380303,17.8794930259532,-2.5));
#39566=CARTESIAN_POINT('Ctrl Pts',(-37.9871697012262,17.6717687488141,-2.5));
#39567=CARTESIAN_POINT('Ctrl Pts',(-38.4456424175336,17.8696845533725,-2.96900170083772));
#39568=CARTESIAN_POINT('Ctrl Pts',(-38.4191252098151,17.8576079915772,-2.5));
#39569=CARTESIAN_POINT('Ctrl Pts',(-37.991443877371,17.6627778699454,-2.5));
#39570=CARTESIAN_POINT('Ctrl Pts',(-38.4510249910641,17.8577775263316,-2.9701475957582));
#39571=CARTESIAN_POINT('Ctrl Pts',(-38.4252432488303,17.8465380939854,-2.5));
#39572=CARTESIAN_POINT('Ctrl Pts',(-37.9934623353037,17.6582483931711,-2.5));
#39573=CARTESIAN_POINT('Ctrl Pts',(-38.4763900971177,17.7977995570222,-2.97589627219185));
#39574=CARTESIAN_POINT('Ctrl Pts',(-38.4545812226388,17.790369539723,-2.5));
#39575=CARTESIAN_POINT('Ctrl Pts',(-38.002974265032,17.6354345524181,-2.5));
#39576=CARTESIAN_POINT('Ctrl Pts',(-38.4917731732021,17.7484124059281,-2.98055544920644));
#39577=CARTESIAN_POINT('Ctrl Pts',(-38.473661265785,17.7435263663243,-2.5));
#39578=CARTESIAN_POINT('Ctrl Pts',(-38.0087429143111,17.6166554164039,-2.5));
#39579=CARTESIAN_POINT('Ctrl Pts',(-38.5049497227733,17.6849440597232,-2.9864412217583));
#39580=CARTESIAN_POINT('Ctrl Pts',(-38.4919775578133,17.6825071777955,-2.5));
#39581=CARTESIAN_POINT('Ctrl Pts',(-38.0136841107577,17.5925304537987,-2.5));
#39582=CARTESIAN_POINT('Ctrl Pts',(-38.5072797054594,17.6721629059777,-2.9876215411643));
#39583=CARTESIAN_POINT('Ctrl Pts',(-38.4953743016544,17.6701248728446,-2.5));
#39584=CARTESIAN_POINT('Ctrl Pts',(-38.0145578594488,17.5876726194739,-2.5));
#39585=CARTESIAN_POINT('Ctrl Pts',(-38.5113201026512,17.646423044551,-2.98998846097813));
#39586=CARTESIAN_POINT('Ctrl Pts',(-38.501596520551,17.645080935214,-2.5));
#39587=CARTESIAN_POINT('Ctrl Pts',(-38.0160730018852,17.5778902994518,-2.5));
#39588=CARTESIAN_POINT('Ctrl Pts',(-38.5130325575213,17.6334445126556,-2.99117686889631));
#39589=CARTESIAN_POINT('Ctrl Pts',(-38.5044245550668,17.6323990130624,-2.5));
#39590=CARTESIAN_POINT('Ctrl Pts',(-38.0167151730816,17.5729582831273,-2.5));
#39591=CARTESIAN_POINT('Ctrl Pts',(-38.5172060896891,17.5943721213219,-2.99473928414168));
#39592=CARTESIAN_POINT('Ctrl Pts',(-38.5120043473919,17.5940082770842,-2.5));
#39593=CARTESIAN_POINT('Ctrl Pts',(-38.0182802555498,17.5581115117232,-2.5));
#39594=CARTESIAN_POINT('Ctrl Pts',(-38.5186917422194,17.5683120165936,-2.99709499970835));
#39595=CARTESIAN_POINT('Ctrl Pts',(-38.5157988525533,17.5682102346573,-2.5));
#39596=CARTESIAN_POINT('Ctrl Pts',(-38.0188373699573,17.5482108332471,-2.5));
#39597=CARTESIAN_POINT('Ctrl Pts',(-38.5191072198307,17.5161686034308,-3.00176886678129));
#39598=CARTESIAN_POINT('Ctrl Pts',(-38.5208771553493,17.5161399120222,-2.5));
#39599=CARTESIAN_POINT('Ctrl Pts',(-38.0189931741039,17.5284038967669,-2.5));
#39600=CARTESIAN_POINT('Ctrl Pts',(-38.5180370412835,17.4900852974077,-3.00408701695548));
#39601=CARTESIAN_POINT('Ctrl Pts',(-38.5221491625175,17.4898665253747,-2.5));
#39602=CARTESIAN_POINT('Ctrl Pts',(-38.0185918623631,17.5184976387542,-2.5));
#39603=CARTESIAN_POINT('Ctrl Pts',(-38.5144871859473,17.4509429730902,-3.00753674366307));
#39604=CARTESIAN_POINT('Ctrl Pts',(-38.5220957984724,17.4501405073408,-2.5));
#39605=CARTESIAN_POINT('Ctrl Pts',(-38.0172606587587,17.5036340064431,-2.5));
#39606=CARTESIAN_POINT('Ctrl Pts',(-38.512979645677,17.4379142878159,-3.00868013835556));
#39607=CARTESIAN_POINT('Ctrl Pts',(-38.5217466988597,17.4368445410147,-2.5));
#39608=CARTESIAN_POINT('Ctrl Pts',(-38.0166953304505,17.4986869777819,-2.5));
#39609=CARTESIAN_POINT('Ctrl Pts',(-38.5093456409823,17.4120774324436,-3.01093824610606));
#39610=CARTESIAN_POINT('Ctrl Pts',(-38.5203938380985,17.4103637207151,-2.5));
#39611=CARTESIAN_POINT('Ctrl Pts',(-38.0153325853393,17.4888774005165,-2.5));
#39612=CARTESIAN_POINT('Ctrl Pts',(-38.5072169868592,17.3992427493601,-3.01205529745571));
#39613=CARTESIAN_POINT('Ctrl Pts',(-38.5193887795888,17.3971525411347,-2.5));
#39614=CARTESIAN_POINT('Ctrl Pts',(-38.014534334724,17.4840047859771,-2.5));
#39615=CARTESIAN_POINT('Ctrl Pts',(-38.4950383810716,17.335482072003,-3.01758225181016));
#39616=CARTESIAN_POINT('Ctrl Pts',(-38.512708363373,17.3310164313404,-2.5));
#39617=CARTESIAN_POINT('Ctrl Pts',(-38.0099673675257,17.4598001953765,-2.5));
#39618=CARTESIAN_POINT('Ctrl Pts',(-38.4804258988967,17.2857825382543,-3.02181836676292));
#39619=CARTESIAN_POINT('Ctrl Pts',(-38.5021474563194,17.2787657562271,-2.5));
#39620=CARTESIAN_POINT('Ctrl Pts',(-38.0044876905449,17.4409392110453,-2.5));
#39621=CARTESIAN_POINT('Ctrl Pts',(-38.4559979025521,17.2253187773268,-3.02689693274587));
#39622=CARTESIAN_POINT('Ctrl Pts',(-38.482188384964,17.2143685236006,-2.5));
#39623=CARTESIAN_POINT('Ctrl Pts',(-37.9953271771502,17.4179991279534,-2.5));
#39624=CARTESIAN_POINT('Ctrl Pts',(-38.4508014471794,17.2133098047403,-3.02790174447839));
#39625=CARTESIAN_POINT('Ctrl Pts',(-38.4778364738777,17.2014855815011,-2.5));
#39626=CARTESIAN_POINT('Ctrl Pts',(-37.9933785134793,17.4134431981463,-2.5));
#39627=CARTESIAN_POINT('Ctrl Pts',(-38.4425304868847,17.1954247892708,-3.02939268814916));
#39628=CARTESIAN_POINT('Ctrl Pts',(-38.4707770006933,17.1822327898589,-2.5));
#39629=CARTESIAN_POINT('Ctrl Pts',(-37.9902768971576,17.4066584740223,-2.5));
#39630=CARTESIAN_POINT('Ctrl Pts',(-38.4396936273783,17.1894842833032,-3.02988697260699));
#39631=CARTESIAN_POINT('Ctrl Pts',(-38.4683326604495,17.1758218953105,-2.5));
#39632=CARTESIAN_POINT('Ctrl Pts',(-37.9892130751568,17.4044050008767,-2.5));
#39633=CARTESIAN_POINT('Ctrl Pts',(-38.433892526343,17.1777122168892,-3.03086468827693));
#39634=CARTESIAN_POINT('Ctrl Pts',(-38.4632915541776,17.1630927437411,-2.5));
#39635=CARTESIAN_POINT('Ctrl Pts',(-37.9870376657812,17.3999395207739,-2.5));
#39636=CARTESIAN_POINT('Ctrl Pts',(-38.4309245022383,17.1718722889636,-3.03134881683581));
#39637=CARTESIAN_POINT('Ctrl Pts',(-38.4606914472883,17.1567656550912,-2.5));
#39638=CARTESIAN_POINT('Ctrl Pts',(-37.9859246535537,17.3977243429034,-2.5));
#39639=CARTESIAN_POINT('Ctrl Pts',(-38.4157502976598,17.1429009507965,-3.03374623521863));
#39640=CARTESIAN_POINT('Ctrl Pts',(-38.4472751802113,17.1252685427155,-2.5));
#39641=CARTESIAN_POINT('Ctrl Pts',(-37.9802343339963,17.3867353766995,-2.5));
#39642=CARTESIAN_POINT('Ctrl Pts',(-38.4025443177972,17.1204528053856,-3.03559000380591));
#39643=CARTESIAN_POINT('Ctrl Pts',(-38.4352923297066,17.1007128648909,-2.5));
#39644=CARTESIAN_POINT('Ctrl Pts',(-37.9752820848364,17.3782217794531,-2.5));
#39645=CARTESIAN_POINT('Ctrl Pts',(-38.3597927098826,17.0552514733911,-3.04091068696068));
#39646=CARTESIAN_POINT('Ctrl Pts',(-38.3955062069388,17.0287324610293,-2.5));
#39647=CARTESIAN_POINT('Ctrl Pts',(-37.9592502348198,17.3534964507582,-2.5));
#39648=CARTESIAN_POINT('Ctrl Pts',(-38.3271443327293,17.0146202226201,-3.04417881485026));
#39649=CARTESIAN_POINT('Ctrl Pts',(-38.3640171485458,16.9833146484955,-2.5));
#39650=CARTESIAN_POINT('Ctrl Pts',(-37.9470071050743,17.3380921508149,-2.5));
#39651=CARTESIAN_POINT('Ctrl Pts',(-38.2809131555838,16.9675438780044,-3.0479256286666));
#39652=CARTESIAN_POINT('Ctrl Pts',(-38.3181512189723,16.9301557601742,-2.5));
#39653=CARTESIAN_POINT('Ctrl Pts',(-37.9296703965765,17.3202474359949,-2.5));
#39654=CARTESIAN_POINT('Ctrl Pts',(-38.2714380751677,16.9583630961748,-3.04865416425237));
#39655=CARTESIAN_POINT('Ctrl Pts',(-38.3086648857525,16.9197304651529,-2.5));
#39656=CARTESIAN_POINT('Ctrl Pts',(-37.9261172426642,17.3167675393722,-2.5));
#39657=CARTESIAN_POINT('Ctrl Pts',(-38.2521347050763,16.9405580024456,-3.05006336142326));
#39658=CARTESIAN_POINT('Ctrl Pts',(-38.2892172779821,16.8994516379931,-2.5));
#39659=CARTESIAN_POINT('Ctrl Pts',(-37.9188784832198,17.3100189529994,-2.5));
#39660=CARTESIAN_POINT('Ctrl Pts',(-38.2422914181653,16.9319183323786,-3.05074524347667));
#39661=CARTESIAN_POINT('Ctrl Pts',(-38.2792412041749,16.8895824979303,-2.5));
#39662=CARTESIAN_POINT('Ctrl Pts',(-37.9151872472733,17.3067444493034,-2.5));
#39663=CARTESIAN_POINT('Ctrl Pts',(-38.2121946005029,16.9067773575311,-3.05272459995863));
#39664=CARTESIAN_POINT('Ctrl Pts',(-38.2485441235301,16.860762254136,-2.5));
#39665=CARTESIAN_POINT('Ctrl Pts',(-37.9039009442048,17.2972161773508,-2.5));
#39666=CARTESIAN_POINT('Ctrl Pts',(-38.1913754559341,16.8910522598471,-3.05395594589729));
#39667=CARTESIAN_POINT('Ctrl Pts',(-38.227102342556,16.842648790628,-2.5));
#39668=CARTESIAN_POINT('Ctrl Pts',(-37.8960937635255,17.2912569793141,-2.5));
#39669=CARTESIAN_POINT('Ctrl Pts',(-38.1482366444428,16.861662216655,-3.05624785925289));
#39670=CARTESIAN_POINT('Ctrl Pts',(-38.1822556751584,16.8086281750341,-2.5));
#39671=CARTESIAN_POINT('Ctrl Pts',(-37.8799167074083,17.280120019,-2.5));
#39672=CARTESIAN_POINT('Ctrl Pts',(-38.1259170445788,16.8479971821675,-3.05730841943199));
#39673=CARTESIAN_POINT('Ctrl Pts',(-38.1588541824173,16.7927328735794,-2.5));
#39674=CARTESIAN_POINT('Ctrl Pts',(-37.8715468617295,17.274942215395,-2.5));
#39675=CARTESIAN_POINT('Ctrl Pts',(-38.0912859803399,16.829081464749,-3.05877140147105));
#39676=CARTESIAN_POINT('Ctrl Pts',(-38.1222868782628,16.7706491428746,-2.5));
#39677=CARTESIAN_POINT('Ctrl Pts',(-37.8585602075906,17.2677752860875,-2.5));
#39678=CARTESIAN_POINT('Ctrl Pts',(-38.0795482163152,16.8230394748505,-3.05923777409933));
#39679=CARTESIAN_POINT('Ctrl Pts',(-38.1098421306826,16.7635765111134,-2.5));
#39680=CARTESIAN_POINT('Ctrl Pts',(-37.854158548831,17.2654861133914,-2.5));
#39681=CARTESIAN_POINT('Ctrl Pts',(-38.0556863997546,16.8114994618048,-3.06012706376275));
#39682=CARTESIAN_POINT('Ctrl Pts',(-38.0844586622232,16.7500420272248,-2.5));
#39683=CARTESIAN_POINT('Ctrl Pts',(-37.8452103654877,17.2611139901796,-2.5));
#39684=CARTESIAN_POINT('Ctrl Pts',(-38.0436500462945,16.8060440839517,-3.06054669237718));
#39685=CARTESIAN_POINT('Ctrl Pts',(-38.0716141384825,16.7436315079723,-2.5));
#39686=CARTESIAN_POINT('Ctrl Pts',(-37.8406967327678,17.2590471876283,-2.5));
#39687=CARTESIAN_POINT('Ctrl Pts',(-37.983033732995,16.7803474050268,-3.06252042955387));
#39688=CARTESIAN_POINT('Ctrl Pts',(-38.006651933923,16.7133430503521,-2.5));
#39689=CARTESIAN_POINT('Ctrl Pts',(-37.817965621475,17.2493120442009,-2.5));
#39690=CARTESIAN_POINT('Ctrl Pts',(-37.9330756082843,16.7647592929747,-3.06370859239269));
#39691=CARTESIAN_POINT('Ctrl Pts',(-37.9526360706556,16.6948699048902,-2.5));
#39692=CARTESIAN_POINT('Ctrl Pts',(-37.7992313215639,17.2434072153618,-2.5));
#39693=CARTESIAN_POINT('Ctrl Pts',(-37.8688152137882,16.7514251465279,-3.06472324864037));
#39694=CARTESIAN_POINT('Ctrl Pts',(-37.8827461609207,16.6790214482703,-2.5));
#39695=CARTESIAN_POINT('Ctrl Pts',(-37.7751336713641,17.2383563320521,-2.5));
#39696=CARTESIAN_POINT('Ctrl Pts',(-37.8558716761049,16.7490686581359,-3.06490240337987));
#39697=CARTESIAN_POINT('Ctrl Pts',(-37.8686399794402,16.6762161508003,-2.5));
#39698=CARTESIAN_POINT('Ctrl Pts',(-37.7702798457447,17.2374637147322,-2.5));
#39699=CARTESIAN_POINT('Ctrl Pts',(-37.836316999401,16.7460068446618,-3.06513506367886));
#39700=CARTESIAN_POINT('Ctrl Pts',(-37.8473067499512,16.6725690712863,-2.5));
#39701=CARTESIAN_POINT('Ctrl Pts',(-37.762946841142,17.2363039481978,-2.5));
#39702=CARTESIAN_POINT('Ctrl Pts',(-37.829775537342,16.7450650975492,-3.06520660039349));
#39703=CARTESIAN_POINT('Ctrl Pts',(-37.8401659882031,16.6714468083953,-2.5));
#39704=CARTESIAN_POINT('Ctrl Pts',(-37.7604937934312,17.23594722548,-2.5));
#39705=CARTESIAN_POINT('Ctrl Pts',(-37.8166456311835,16.7433410180028,-3.0653375358751));
#39706=CARTESIAN_POINT('Ctrl Pts',(-37.82582654984,16.669391703467,-2.5));
#39707=CARTESIAN_POINT('Ctrl Pts',(-37.7555700780584,17.2352941782029,-2.5));
#39708=CARTESIAN_POINT('Ctrl Pts',(-37.8100479347227,16.7425577604292,-3.06539700330435));
#39709=CARTESIAN_POINT('Ctrl Pts',(-37.818617934926,16.668457783908,-2.5));
#39710=CARTESIAN_POINT('Ctrl Pts',(-37.7530959419294,17.2349974951212,-2.5));
#39711=CARTESIAN_POINT('Ctrl Pts',(-37.777067284866,16.7390579643222,-3.06566266886128));
#39712=CARTESIAN_POINT('Ctrl Pts',(-37.7825632243643,16.6642830215665,-2.5));
#39713=CARTESIAN_POINT('Ctrl Pts',(-37.7407281994226,17.2336718308661,-2.5));
#39714=CARTESIAN_POINT('Ctrl Pts',(-37.7507569280122,16.7375882697876,-3.06577409663493));
#39715=CARTESIAN_POINT('Ctrl Pts',(-37.7537706577765,16.6625286572503,-2.5));
#39716=CARTESIAN_POINT('Ctrl Pts',(-37.7308618146269,17.2331151625715,-2.5));
#39717=CARTESIAN_POINT('Ctrl Pts',(-37.6720409935013,16.7370385868534,-3.06581578422071));
#39718=CARTESIAN_POINT('Ctrl Pts',(-37.6675998077381,16.6618723975768,-2.5));
#39719=CARTESIAN_POINT('Ctrl Pts',(-37.7013433392571,17.2329069461004,-2.5));
#39720=CARTESIAN_POINT('Ctrl Pts',(-37.6198485285534,16.7417812990776,-3.06545669284864));
#39721=CARTESIAN_POINT('Ctrl Pts',(-37.6105054868964,16.6675345545024,-2.5));
#39722=CARTESIAN_POINT('Ctrl Pts',(-37.6817711620469,17.2347033137879,-2.5));
#39723=CARTESIAN_POINT('Ctrl Pts',(-37.5549716201007,16.7542328279335,-3.06450964654665));
#39724=CARTESIAN_POINT('Ctrl Pts',(-37.539791579201,16.6823618030451,-2.5));
#39725=CARTESIAN_POINT('Ctrl Pts',(-37.6574423248857,17.2394198627989,-2.5));
#39726=CARTESIAN_POINT('Ctrl Pts',(-37.5419780772432,16.7570618699045,-3.06429433377577));
#39727=CARTESIAN_POINT('Ctrl Pts',(-37.5256575742345,16.6857256023118,-2.5));
#39728=CARTESIAN_POINT('Ctrl Pts',(-37.6525697466396,17.2404914902659,-2.5));
#39729=CARTESIAN_POINT('Ctrl Pts',(-37.5162549007385,16.7633361071356,-3.06381631649363));
#39730=CARTESIAN_POINT('Ctrl Pts',(-37.4977213282955,16.6931780113973,-2.5));
#39731=CARTESIAN_POINT('Ctrl Pts',(-37.642923553396,17.2428681687046,-2.5));
#39732=CARTESIAN_POINT('Ctrl Pts',(-37.5035214136028,16.7667796187423,-3.0635537446777));
#39733=CARTESIAN_POINT('Ctrl Pts',(-37.4839161235599,16.6972638969602,-2.5));
#39734=CARTESIAN_POINT('Ctrl Pts',(-37.6381484975799,17.2441725977466,-2.5));
#39735=CARTESIAN_POINT('Ctrl Pts',(-37.4656977945507,16.7780114577165,-3.06269625818825));
#39736=CARTESIAN_POINT('Ctrl Pts',(-37.4430016133797,16.7105699687229,-2.5));
#39737=CARTESIAN_POINT('Ctrl Pts',(-37.6239646379375,17.2484273528784,-2.5));
#39738=CARTESIAN_POINT('Ctrl Pts',(-37.4409836224016,16.7866989403601,-3.06203177270948));
#39739=CARTESIAN_POINT('Ctrl Pts',(-37.4163729269822,16.720839368388,-2.5));
#39740=CARTESIAN_POINT('Ctrl Pts',(-37.6146968252125,17.2517183816627,-2.5));
#39741=CARTESIAN_POINT('Ctrl Pts',(-37.3925416751236,16.80643246839,-3.06051737328866));
#39742=CARTESIAN_POINT('Ctrl Pts',(-37.3644453567216,16.7440900855917,-2.5));
#39743=CARTESIAN_POINT('Ctrl Pts',(-37.5965310946519,17.2591942841924,-2.5));
#39744=CARTESIAN_POINT('Ctrl Pts',(-37.3688139142769,16.8174785426132,-3.05966746752498));
#39745=CARTESIAN_POINT('Ctrl Pts',(-37.3391549609578,16.7570619950295,-2.5));
#39746=CARTESIAN_POINT('Ctrl Pts',(-37.5876331822018,17.2633791709517,-2.5));
#39747=CARTESIAN_POINT('Ctrl Pts',(-37.3339711607475,16.8358377670208,-3.05824914363553));
#39748=CARTESIAN_POINT('Ctrl Pts',(-37.3022443333108,16.7785464121055,-2.5));
#39749=CARTESIAN_POINT('Ctrl Pts',(-37.5745671530757,17.270335145276,-2.5));
#39750=CARTESIAN_POINT('Ctrl Pts',(-37.3224819496572,16.8422563904187,-3.05775241081752));
#39751=CARTESIAN_POINT('Ctrl Pts',(-37.2901231475283,16.7860382908692,-2.5));
#39752=CARTESIAN_POINT('Ctrl Pts',(-37.570258695808,17.2727671020922,-2.5));
#39753=CARTESIAN_POINT('Ctrl Pts',(-37.2997579173503,16.8557016280555,-3.05670968389331));
#39754=CARTESIAN_POINT('Ctrl Pts',(-37.2662411766355,16.8016967416051,-2.5));
#39755=CARTESIAN_POINT('Ctrl Pts',(-37.5617371876123,17.2778615635871,-2.5));
#39756=CARTESIAN_POINT('Ctrl Pts',(-37.2885084984505,16.8627400253605,-3.0561627663965));
#39757=CARTESIAN_POINT('Ctrl Pts',(-37.2544661462563,16.8098753233558,-2.5));
#39758=CARTESIAN_POINT('Ctrl Pts',(-37.5575186558127,17.2805285214769,-2.5));
#39759=CARTESIAN_POINT('Ctrl Pts',(-37.2335131076936,16.8990718659001,-3.05333313807168));
#39760=CARTESIAN_POINT('Ctrl Pts',(-37.1972561950466,16.8519104255022,-2.5));
#39761=CARTESIAN_POINT('Ctrl Pts',(-37.5368953730412,17.2942956929266,-2.5));
#39762=CARTESIAN_POINT('Ctrl Pts',(-37.1930113241315,16.9320140399769,-3.05074799765065));
#39763=CARTESIAN_POINT('Ctrl Pts',(-37.1558511506002,16.8897253205875,-2.5));
#39764=CARTESIAN_POINT('Ctrl Pts',(-37.5217072095524,17.3067799280439,-2.5));
#39765=CARTESIAN_POINT('Ctrl Pts',(-37.1373488654157,16.987068334806,-3.04637357495642));
#39766=CARTESIAN_POINT('Ctrl Pts',(-37.1001829683923,16.9522623708449,-2.5));
#39767=CARTESIAN_POINT('Ctrl Pts',(-37.5008337929987,17.3276482177729,-2.5));
#39768=CARTESIAN_POINT('Ctrl Pts',(-37.119649230241,17.0063667438965,-3.04483205480724));
#39769=CARTESIAN_POINT('Ctrl Pts',(-37.08275128213,16.9740145507512,-2.5));
#39770=CARTESIAN_POINT('Ctrl Pts',(-37.4941964218283,17.334963880511,-2.5));
#39771=CARTESIAN_POINT('Ctrl Pts',(-37.09862407612,17.0317074280592,-3.04279459962286));
#39772=CARTESIAN_POINT('Ctrl Pts',(-37.0623359323734,17.0024240843538,-2.5));
#39773=CARTESIAN_POINT('Ctrl Pts',(-37.4863119967309,17.344571096994,-2.5));
#39774=CARTESIAN_POINT('Ctrl Pts',(-37.0944707116322,17.0368412601703,-3.04238118958153));
#39775=CARTESIAN_POINT('Ctrl Pts',(-37.0583251973171,17.0081622414672,-2.5));
#39776=CARTESIAN_POINT('Ctrl Pts',(-37.4847544852643,17.3465174947961,-2.5));
#39777=CARTESIAN_POINT('Ctrl Pts',(-37.086318602129,17.0471765103316,-3.04154758456322));
#39778=CARTESIAN_POINT('Ctrl Pts',(-37.0504867079477,17.0196942280984,-2.5));
#39779=CARTESIAN_POINT('Ctrl Pts',(-37.4816974406886,17.350436015139,-2.5));
#39780=CARTESIAN_POINT('Ctrl Pts',(-37.0823147848581,17.0523838124048,-3.04112691976143));
#39781=CARTESIAN_POINT('Ctrl Pts',(-37.0466539524108,17.0254945229426,-2.5));
#39782=CARTESIAN_POINT('Ctrl Pts',(-37.4801960124776,17.3524103736432,-2.5));
#39783=CARTESIAN_POINT('Ctrl Pts',(-37.0705176170079,17.0681234054201,-3.03985333807572));
#39784=CARTESIAN_POINT('Ctrl Pts',(-37.0354170178543,17.0429878142689,-2.5));
#39785=CARTESIAN_POINT('Ctrl Pts',(-37.475772070005,17.3583782202939,-2.5));
#39786=CARTESIAN_POINT('Ctrl Pts',(-37.0629384235517,17.0787733000584,-3.03898884786155));
#39787=CARTESIAN_POINT('Ctrl Pts',(-37.0282631566779,17.0547884840968,-2.5));
#39788=CARTESIAN_POINT('Ctrl Pts',(-37.4729298774794,17.3624164681974,-2.5));
#39789=CARTESIAN_POINT('Ctrl Pts',(-37.026446523552,17.132793523799,-3.03458889787333));
#39790=CARTESIAN_POINT('Ctrl Pts',(-36.9942613247177,17.1142615428478,-2.5));
#39791=CARTESIAN_POINT('Ctrl Pts',(-37.4592454049732,17.3829010974121,-2.5));
#39792=CARTESIAN_POINT('Ctrl Pts',(-37.0017062809529,17.1784542255603,-3.03082304423241));
#39793=CARTESIAN_POINT('Ctrl Pts',(-36.9722499558993,17.1639506562642,-2.5));
#39794=CARTESIAN_POINT('Ctrl Pts',(-37.4499678115662,17.4002194094609,-2.5));
#39795=CARTESIAN_POINT('Ctrl Pts',(-36.9763738972329,17.2385950219028,-3.02578307239997));
#39796=CARTESIAN_POINT('Ctrl Pts',(-36.9511407639783,17.2285709769479,-2.5));
#39797=CARTESIAN_POINT('Ctrl Pts',(-37.4404681807179,17.4230360661467,-2.5));
#39798=CARTESIAN_POINT('Ctrl Pts',(-36.9715895606736,17.2507777927924,-3.02475831530062));
#39799=CARTESIAN_POINT('Ctrl Pts',(-36.9472559919366,17.2415671008265,-2.5));
#39800=CARTESIAN_POINT('Ctrl Pts',(-37.4386740479595,17.4276583514805,-2.5));
#39801=CARTESIAN_POINT('Ctrl Pts',(-36.9625961480096,17.2754584703774,-3.02267407819011));
#39802=CARTESIAN_POINT('Ctrl Pts',(-36.9401413648218,17.2677878485332,-2.5));
#39803=CARTESIAN_POINT('Ctrl Pts',(-37.4353015260892,17.4370231465561,-2.5));
#39804=CARTESIAN_POINT('Ctrl Pts',(-36.9584132845463,17.2878868497566,-3.02162045942486));
#39805=CARTESIAN_POINT('Ctrl Pts',(-36.9369311676226,17.2809375542772,-2.5));
#39806=CARTESIAN_POINT('Ctrl Pts',(-37.4337329516611,17.441739269899,-2.5));
#39807=CARTESIAN_POINT('Ctrl Pts',(-36.9468363797903,17.3252899977778,-3.01843695447992));
#39808=CARTESIAN_POINT('Ctrl Pts',(-36.9283615872827,17.3203042842923,-2.5));
#39809=CARTESIAN_POINT('Ctrl Pts',(-37.4293916024477,17.4559334232034,-2.5));
#39810=CARTESIAN_POINT('Ctrl Pts',(-36.9403896403824,17.3504426477826,-3.01627937557837));
#39811=CARTESIAN_POINT('Ctrl Pts',(-36.9240158817722,17.3465871928938,-2.5));
#39812=CARTESIAN_POINT('Ctrl Pts',(-37.4269740834161,17.4654799598295,-2.5));
#39813=CARTESIAN_POINT('Ctrl Pts',(-36.9299795767171,17.401171550854,-3.01189204818851));
#39814=CARTESIAN_POINT('Ctrl Pts',(-36.9179681053284,17.3991512563075,-2.5));
#39815=CARTESIAN_POINT('Ctrl Pts',(-37.4230703062887,17.4847366734944,-2.5));
#39816=CARTESIAN_POINT('Ctrl Pts',(-36.9260163611498,17.4267478207179,-3.0096623048872));
#39817=CARTESIAN_POINT('Ctrl Pts',(-36.9162547401427,17.4254293823291,-2.5));
#39818=CARTESIAN_POINT('Ctrl Pts',(-37.421584098594,17.4944468593896,-2.5));
#39819=CARTESIAN_POINT('Ctrl Pts',(-36.9205861826877,17.4783255467987,-3.0051277827859));
#39820=CARTESIAN_POINT('Ctrl Pts',(-36.91541973322,17.4779707405914,-2.5));
#39821=CARTESIAN_POINT('Ctrl Pts',(-37.4195477886376,17.5140317228638,-2.5));
#39822=CARTESIAN_POINT('Ctrl Pts',(-36.919118933325,17.5043343662994,-3.00282235189172));
#39823=CARTESIAN_POINT('Ctrl Pts',(-36.9162867050069,17.5042383112405,-2.5));
#39824=CARTESIAN_POINT('Ctrl Pts',(-37.4189975669682,17.5239091955899,-2.5));
#39825=CARTESIAN_POINT('Ctrl Pts',(-36.918942728626,17.5305480494939,-3.00047863991406));
#39826=CARTESIAN_POINT('Ctrl Pts',(-36.9184636408495,17.5305448701384,-2.5));
#39827=CARTESIAN_POINT('Ctrl Pts',(-37.418931489881,17.5338661095488,-2.5));
#39828=CARTESIAN_POINT('Ctrl Pts',(-38.0189154695161,17.5383073665605,-2.50000000000004));
#39829=CARTESIAN_POINT('Ctrl Pts',(-38.0189627830564,17.5323016024105,-2.50000000000007));
#39830=CARTESIAN_POINT('Ctrl Pts',(-38.0188335214001,17.526294798684,-2.5));
#39831=CARTESIAN_POINT('Ctrl Pts',(-38.0185267455263,17.5202869732672,-2.5));
#39832=CARTESIAN_POINT('Ctrl Pts',(-38.0183276500332,17.5163879346995,-2.5));
#39833=CARTESIAN_POINT('Ctrl Pts',(-38.0180536771219,17.5124884613595,-2.5));
#39834=CARTESIAN_POINT('Ctrl Pts',(-38.0177044004012,17.5085885499102,-2.5));
#39835=CARTESIAN_POINT('Ctrl Pts',(-38.0172606705395,17.5036340050864,-2.5));
#39836=CARTESIAN_POINT('Ctrl Pts',(-38.0166953474297,17.4986869761097,-2.5));
#39837=CARTESIAN_POINT('Ctrl Pts',(-38.0160139739599,17.4937821869174,-2.5));
#39838=CARTESIAN_POINT('Ctrl Pts',(-38.0158691453091,17.4927396543972,-2.5));
#39839=CARTESIAN_POINT('Ctrl Pts',(-38.0157190359243,17.4916985754705,-2.5));
#39840=CARTESIAN_POINT('Ctrl Pts',(-38.0155636624038,17.4906589455518,-2.5));
#39841=CARTESIAN_POINT('Ctrl Pts',(-38.014988053617,17.4868074519734,-2.5));
#39842=CARTESIAN_POINT('Ctrl Pts',(-38.0143402000425,17.482975834817,-2.5));
#39843=CARTESIAN_POINT('Ctrl Pts',(-38.0136209507028,17.4791638660799,-2.5));
#39844=CARTESIAN_POINT('Ctrl Pts',(-38.0106871725347,17.4636150570073,-2.5));
#39845=CARTESIAN_POINT('Ctrl Pts',(-38.0065759453709,17.4483902924033,-2.49999999999996));
#39846=CARTESIAN_POINT('Ctrl Pts',(-38.0012757977561,17.4334930688153,-2.50000000000006));
#39847=CARTESIAN_POINT('Ctrl Pts',(-37.9999753398566,17.4298378475833,-2.50000000000009));
#39848=CARTESIAN_POINT('Ctrl Pts',(-37.9986033182443,17.4262026238621,-2.50000000000007));
#39849=CARTESIAN_POINT('Ctrl Pts',(-37.9971594850432,17.4225870626251,-2.50000000000005));
#39850=CARTESIAN_POINT('Ctrl Pts',(-37.9953274844092,17.4179994755872,-2.50000000000002));
#39851=CARTESIAN_POINT('Ctrl Pts',(-37.9933788600298,17.4134438231221,-2.5));
#39852=CARTESIAN_POINT('Ctrl Pts',(-37.9913107977719,17.4089200356984,-2.5));
#39853=CARTESIAN_POINT('Ctrl Pts',(-37.9908731012467,17.407962595453,-2.5));
#39854=CARTESIAN_POINT('Ctrl Pts',(-37.9904300218038,17.4070065658388,-2.5));
#39855=CARTESIAN_POINT('Ctrl Pts',(-37.9899820161801,17.4060528984355,-2.5));
#39856=CARTESIAN_POINT('Ctrl Pts',(-37.9893718123521,17.4047539604999,-2.5));
#39857=CARTESIAN_POINT('Ctrl Pts',(-37.9887525557905,17.4034596118976,-2.5));
#39858=CARTESIAN_POINT('Ctrl Pts',(-37.9881254017715,17.4021722455759,-2.5));
#39859=CARTESIAN_POINT('Ctrl Pts',(-37.9870375902219,17.3999392822031,-2.5));
#39860=CARTESIAN_POINT('Ctrl Pts',(-37.9859245939872,17.397724152872,-2.5));
#39861=CARTESIAN_POINT('Ctrl Pts',(-37.9847866171473,17.3955265354199,-2.5));
#39862=CARTESIAN_POINT('Ctrl Pts',(-37.9820294084877,17.3902019192611,-2.5));
#39863=CARTESIAN_POINT('Ctrl Pts',(-37.9791258866422,17.3849798744598,-2.5));
#39864=CARTESIAN_POINT('Ctrl Pts',(-37.9760768589988,17.3798572660055,-2.5));
#39865=CARTESIAN_POINT('Ctrl Pts',(-37.9740918835002,17.3765223496125,-2.5));
#39866=CARTESIAN_POINT('Ctrl Pts',(-37.9720454773427,17.3732300388444,-2.5));
#39867=CARTESIAN_POINT('Ctrl Pts',(-37.9699381542059,17.3699799906587,-2.5));
#39868=CARTESIAN_POINT('Ctrl Pts',(-37.9613591254407,17.3567488651679,-2.5));
#39869=CARTESIAN_POINT('Ctrl Pts',(-37.9517779186379,17.3442130263075,-2.5));
#39870=CARTESIAN_POINT('Ctrl Pts',(-37.9411583825942,17.3323984400336,-2.5));
#39871=CARTESIAN_POINT('Ctrl Pts',(-37.9385479640711,17.3294942627961,-2.5));
#39872=CARTESIAN_POINT('Ctrl Pts',(-37.935875250628,17.3266341069194,-2.49999999999999));
#39873=CARTESIAN_POINT('Ctrl Pts',(-37.9331377938301,17.3238163249865,-2.50000000000001));
#39874=CARTESIAN_POINT('Ctrl Pts',(-37.9324072910173,17.3230643870456,-2.50000000000001));
#39875=CARTESIAN_POINT('Ctrl Pts',(-37.931672878228,17.3223162896498,-2.50000000000001));
#39876=CARTESIAN_POINT('Ctrl Pts',(-37.9309346989953,17.321572153053,-2.50000000000002));
#39877=CARTESIAN_POINT('Ctrl Pts',(-37.9281679076421,17.3187830327274,-2.50000000000006));
#39878=CARTESIAN_POINT('Ctrl Pts',(-37.9253540527131,17.3160558693812,-2.50000000000001));
#39879=CARTESIAN_POINT('Ctrl Pts',(-37.9224978903194,17.3133932168198,-2.5));
#39880=CARTESIAN_POINT('Ctrl Pts',(-37.9217364535199,17.3126833686512,-2.5));
#39881=CARTESIAN_POINT('Ctrl Pts',(-37.9209717564412,17.311977852874,-2.5));
#39882=CARTESIAN_POINT('Ctrl Pts',(-37.9202037072535,17.3112765614779,-2.5));
#39883=CARTESIAN_POINT('Ctrl Pts',(-37.9173220266189,17.3086453526081,-2.5));
#39884=CARTESIAN_POINT('Ctrl Pts',(-37.9143956775635,17.3060761773964,-2.5));
#39885=CARTESIAN_POINT('Ctrl Pts',(-37.91142514877,17.3035683556681,-2.5));
#39886=CARTESIAN_POINT('Ctrl Pts',(-37.9068726347334,17.2997249680383,-2.5));
#39887=CARTESIAN_POINT('Ctrl Pts',(-37.9022165303951,17.2960254389671,-2.5));
#39888=CARTESIAN_POINT('Ctrl Pts',(-37.8974571980587,17.2924692568552,-2.5));
#39889=CARTESIAN_POINT('Ctrl Pts',(-37.8943505147015,17.2901479371822,-2.5));
#39890=CARTESIAN_POINT('Ctrl Pts',(-37.891199835165,17.2878877196527,-2.5));
#39891=CARTESIAN_POINT('Ctrl Pts',(-37.8880052659395,17.285688454894,-2.5));
#39892=CARTESIAN_POINT('Ctrl Pts',(-37.8831125345718,17.2823201097711,-2.5));
#39893=CARTESIAN_POINT('Ctrl Pts',(-37.8781168611668,17.2790947284676,-2.5));
#39894=CARTESIAN_POINT('Ctrl Pts',(-37.8730167977921,17.2760143027342,-2.5));
#39895=CARTESIAN_POINT('Ctrl Pts',(-37.8696855682523,17.2740022482862,-2.5));
#39896=CARTESIAN_POINT('Ctrl Pts',(-37.8663097399484,17.2720520067105,-2.5));
#39897=CARTESIAN_POINT('Ctrl Pts',(-37.8628890941836,17.2701642591167,-2.5));
#39898=CARTESIAN_POINT('Ctrl Pts',(-37.861981599614,17.2696634411987,-2.5));
#39899=CARTESIAN_POINT('Ctrl Pts',(-37.8610709158903,17.2691670147014,-2.5));
#39900=CARTESIAN_POINT('Ctrl Pts',(-37.8601570499388,17.2686750119215,-2.5));
#39901=CARTESIAN_POINT('Ctrl Pts',(-37.8567118526816,17.2668202031006,-2.5));
#39902=CARTESIAN_POINT('Ctrl Pts',(-37.8532208743116,17.2650279611968,-2.5));
#39903=CARTESIAN_POINT('Ctrl Pts',(-37.8496844586753,17.2633000486829,-2.5));
#39904=CARTESIAN_POINT('Ctrl Pts',(-37.848746946163,17.2628419748114,-2.5));
#39905=CARTESIAN_POINT('Ctrl Pts',(-37.8478076846838,17.2623891308455,-2.5));
#39906=CARTESIAN_POINT('Ctrl Pts',(-37.8468667418028,17.2619415236482,-2.5));
#39907=CARTESIAN_POINT('Ctrl Pts',(-37.8433171174546,17.2602529648227,-2.5));
#39908=CARTESIAN_POINT('Ctrl Pts',(-37.8397439187893,17.2586391053616,-2.5));
#39909=CARTESIAN_POINT('Ctrl Pts',(-37.8361505179169,17.2571001416462,-2.5));
#39910=CARTESIAN_POINT('Ctrl Pts',(-37.8215612152096,17.2508519082044,-2.5));
#39911=CARTESIAN_POINT('Ctrl Pts',(-37.8066209717456,17.24581669925,-2.49999999999996));
#39912=CARTESIAN_POINT('Ctrl Pts',(-37.7913279313869,17.2419826890728,-2.50000000000007));
#39913=CARTESIAN_POINT('Ctrl Pts',(-37.7875576854708,17.2410374773377,-2.50000000000009));
#39914=CARTESIAN_POINT('Ctrl Pts',(-37.7837661046096,17.2401654107225,-2.50000000000008));
#39915=CARTESIAN_POINT('Ctrl Pts',(-37.7799532476229,17.2393662882056,-2.50000000000005));
#39916=CARTESIAN_POINT('Ctrl Pts',(-37.7751337035001,17.2383561778754,-2.50000000000002));
#39917=CARTESIAN_POINT('Ctrl Pts',(-37.7702798591916,17.2374636662302,-2.5));
#39918=CARTESIAN_POINT('Ctrl Pts',(-37.7653911781742,17.2366905233561,-2.5));
#39919=CARTESIAN_POINT('Ctrl Pts',(-37.7643715662832,17.2365292721586,-2.5));
#39920=CARTESIAN_POINT('Ctrl Pts',(-37.7633504386129,17.2363732145414,-2.5));
#39921=CARTESIAN_POINT('Ctrl Pts',(-37.7623277881001,17.2362223736589,-2.5));
#39922=CARTESIAN_POINT('Ctrl Pts',(-37.7608988179668,17.2360116006595,-2.5));
#39923=CARTESIAN_POINT('Ctrl Pts',(-37.7594668741216,17.2358110159626,-2.5));
#39924=CARTESIAN_POINT('Ctrl Pts',(-37.7580319373903,17.2356206894349,-2.5));
#39925=CARTESIAN_POINT('Ctrl Pts',(-37.7555700795487,17.2352941545819,-2.5));
#39926=CARTESIAN_POINT('Ctrl Pts',(-37.7530959436449,17.2349974558877,-2.5));
#39927=CARTESIAN_POINT('Ctrl Pts',(-37.7506223976568,17.2347323228172,-2.5));
#39928=CARTESIAN_POINT('Ctrl Pts',(-37.7495913604537,17.2346218085753,-2.5));
#39929=CARTESIAN_POINT('Ctrl Pts',(-37.7485606256491,17.2345167684412,-2.5));
#39930=CARTESIAN_POINT('Ctrl Pts',(-37.7475301924415,17.2344171850529,-2.5));
#39931=CARTESIAN_POINT('Ctrl Pts',(-37.7425867575079,17.2339394403559,-2.5));
#39932=CARTESIAN_POINT('Ctrl Pts',(-37.7376502518963,17.2335871585163,-2.5));
#39933=CARTESIAN_POINT('Ctrl Pts',(-37.732720534154,17.2333582875895,-2.5));
#39934=CARTESIAN_POINT('Ctrl Pts',(-37.7288168891892,17.233177053919,-2.5));
#39935=CARTESIAN_POINT('Ctrl Pts',(-37.7249175017295,17.2330732131101,-2.5));
#39936=CARTESIAN_POINT('Ctrl Pts',(-37.7210223229877,17.2330457357049,-2.5));
#39937=CARTESIAN_POINT('Ctrl Pts',(-37.7052413970366,17.232934413754,-2.5));
#39938=CARTESIAN_POINT('Ctrl Pts',(-37.6895290645007,17.2340676126699,-2.5));
#39939=CARTESIAN_POINT('Ctrl Pts',(-37.6738870110463,17.2364666559217,-2.5));
#39940=CARTESIAN_POINT('Ctrl Pts',(-37.6700231603601,17.2370592600157,-2.5));
#39941=CARTESIAN_POINT('Ctrl Pts',(-37.6661623118345,17.2377293485442,-2.5));
#39942=CARTESIAN_POINT('Ctrl Pts',(-37.6623080806904,17.2384764930194,-2.5));
#39943=CARTESIAN_POINT('Ctrl Pts',(-37.6612987119646,17.2386721596099,-2.50000000000001));
#39944=CARTESIAN_POINT('Ctrl Pts',(-37.660289210411,17.2388733128986,-2.50000000000001));
#39945=CARTESIAN_POINT('Ctrl Pts',(-37.6592801428124,17.2390798290796,-2.50000000000001));
#39946=CARTESIAN_POINT('Ctrl Pts',(-37.6554261020534,17.2398685986132,-2.50000000000004));
#39947=CARTESIAN_POINT('Ctrl Pts',(-37.6515701993178,17.2407376700213,-2.5));
#39948=CARTESIAN_POINT('Ctrl Pts',(-37.6477466423331,17.2416797982958,-2.5));
#39949=CARTESIAN_POINT('Ctrl Pts',(-37.6467465078848,17.2419262324266,-2.5));
#39950=CARTESIAN_POINT('Ctrl Pts',(-37.6457485236272,17.2421776330844,-2.5));
#39951=CARTESIAN_POINT('Ctrl Pts',(-37.6447527879308,17.2424339430849,-2.5));
#39952=CARTESIAN_POINT('Ctrl Pts',(-37.6409454659456,17.2434139769465,-2.5));
#39953=CARTESIAN_POINT('Ctrl Pts',(-37.6371682078251,17.2444666547528,-2.5));
#39954=CARTESIAN_POINT('Ctrl Pts',(-37.6334205438091,17.2455908476015,-2.5));
#39955=CARTESIAN_POINT('Ctrl Pts',(-37.62771375832,17.2473027212937,-2.5));
#39956=CARTESIAN_POINT('Ctrl Pts',(-37.6220754800291,17.2491801446527,-2.5));
#39957=CARTESIAN_POINT('Ctrl Pts',(-37.6165050088923,17.2512214488661,-2.5));
#39958=CARTESIAN_POINT('Ctrl Pts',(-37.6128454688109,17.2525624906566,-2.5));
#39959=CARTESIAN_POINT('Ctrl Pts',(-37.6092151764346,17.2539742724173,-2.5));
#39960=CARTESIAN_POINT('Ctrl Pts',(-37.6056139518807,17.2554563133632,-2.5));
#39961=CARTESIAN_POINT('Ctrl Pts',(-37.5965310358405,17.2591942789575,-2.5));
#39962=CARTESIAN_POINT('Ctrl Pts',(-37.5876330400573,17.2633792084384,-2.5));
#39963=CARTESIAN_POINT('Ctrl Pts',(-37.5789224592486,17.2680164179132,-2.50000000000001));
#39964=CARTESIAN_POINT('Ctrl Pts',(-37.5745670413693,17.2703350905137,-2.50000000000001));
#39965=CARTESIAN_POINT('Ctrl Pts',(-37.5702585583013,17.2727670296124,-2.50000000000002));
#39966=CARTESIAN_POINT('Ctrl Pts',(-37.5659978498847,17.2753141792429,-2.50000000000003));
#39967=CARTESIAN_POINT('Ctrl Pts',(-37.565118441144,17.2758399100439,-2.50000000000004));
#39968=CARTESIAN_POINT('Ctrl Pts',(-37.5642408341502,17.2763707385894,-2.50000000000004));
#39969=CARTESIAN_POINT('Ctrl Pts',(-37.5633654832279,17.2769063722233,-2.50000000000004));
#39970=CARTESIAN_POINT('Ctrl Pts',(-37.5599999378737,17.2789657740497,-2.50000000000006));
#39971=CARTESIAN_POINT('Ctrl Pts',(-37.5566672283182,17.2810965684525,-2.50000000000007));
#39972=CARTESIAN_POINT('Ctrl Pts',(-37.5533938832534,17.2832817819911,-2.50000000000004));
#39973=CARTESIAN_POINT('Ctrl Pts',(-37.5525431027284,17.283849744453,-2.50000000000004));
#39974=CARTESIAN_POINT('Ctrl Pts',(-37.5516958228496,17.2844216135967,-2.50000000000003));
#39975=CARTESIAN_POINT('Ctrl Pts',(-37.5508520501366,17.2849973762455,-2.50000000000002));
#39976=CARTESIAN_POINT('Ctrl Pts',(-37.5467618946436,17.2877883633497,-2.49999999999998));
#39977=CARTESIAN_POINT('Ctrl Pts',(-37.5427534964736,17.2906709132821,-2.5));
#39978=CARTESIAN_POINT('Ctrl Pts',(-37.5388261662278,17.2936446071485,-2.5));
#39979=CARTESIAN_POINT('Ctrl Pts',(-37.5309715057361,17.2995919948813,-2.5));
#39980=CARTESIAN_POINT('Ctrl Pts',(-37.5234412766274,17.3059038765257,-2.49999999999992));
#39981=CARTESIAN_POINT('Ctrl Pts',(-37.516230966746,17.312574402672,-2.50000000000008));
#39982=CARTESIAN_POINT('Ctrl Pts',(-37.513367337156,17.3152236530326,-2.50000000000014));
#39983=CARTESIAN_POINT('Ctrl Pts',(-37.5105542607098,17.3179296200831,-2.50000000000013));
#39984=CARTESIAN_POINT('Ctrl Pts',(-37.507791384449,17.3206919070763,-2.50000000000009));
#39985=CARTESIAN_POINT('Ctrl Pts',(-37.5035976368246,17.3248847602562,-2.50000000000003));
#39986=CARTESIAN_POINT('Ctrl Pts',(-37.4995203862508,17.329208307633,-2.5));
#39987=CARTESIAN_POINT('Ctrl Pts',(-37.4955614569713,17.3336646801914,-2.5));
#39988=CARTESIAN_POINT('Ctrl Pts',(-37.492952123164,17.3366018793061,-2.5));
#39989=CARTESIAN_POINT('Ctrl Pts',(-37.4903949401247,17.3395960061336,-2.5));
#39990=CARTESIAN_POINT('Ctrl Pts',(-37.4878888724731,17.3426496460838,-2.5));
#39991=CARTESIAN_POINT('Ctrl Pts',(-37.487241336329,17.3434386679754,-2.5));
#39992=CARTESIAN_POINT('Ctrl Pts',(-37.4865970049051,17.3442319721867,-2.5));
#39993=CARTESIAN_POINT('Ctrl Pts',(-37.4859565191968,17.345028757489,-2.5));
#39994=CARTESIAN_POINT('Ctrl Pts',(-37.4850374162825,17.3461721517661,-2.5));
#39995=CARTESIAN_POINT('Ctrl Pts',(-37.4841265961072,17.3473222729907,-2.5));
#39996=CARTESIAN_POINT('Ctrl Pts',(-37.4832259396789,17.3484767367919,-2.5));
#39997=CARTESIAN_POINT('Ctrl Pts',(-37.4816972641988,17.3504361970814,-2.5));
#39998=CARTESIAN_POINT('Ctrl Pts',(-37.4801959692323,17.3524104032434,-2.5));
#39999=CARTESIAN_POINT('Ctrl Pts',(-37.4787213561336,17.3543996492973,-2.5));
#40000=CARTESIAN_POINT('Ctrl Pts',(-37.478116210868,17.3552159873814,-2.5));
#40001=CARTESIAN_POINT('Ctrl Pts',(-37.4775155587945,17.3560348581811,-2.5));
#40002=CARTESIAN_POINT('Ctrl Pts',(-37.476919360215,17.3568562868653,-2.5));
#40003=CARTESIAN_POINT('Ctrl Pts',(-37.4746101165123,17.3600379097028,-2.5));
#40004=CARTESIAN_POINT('Ctrl Pts',(-37.4723682904248,17.3632571145556,-2.5));
#40005=CARTESIAN_POINT('Ctrl Pts',(-37.4701929802585,17.3665133922235,-2.5));
#40006=CARTESIAN_POINT('Ctrl Pts',(-37.4614223503606,17.3796423734205,-2.5));
#40007=CARTESIAN_POINT('Ctrl Pts',(-37.4537235445676,17.3933687395656,-2.5));
#40008=CARTESIAN_POINT('Ctrl Pts',(-37.4471007774525,17.4076943969358,-2.5));
#40009=CARTESIAN_POINT('Ctrl Pts',(-37.4454569144177,17.4112502246117,-2.5));
#40010=CARTESIAN_POINT('Ctrl Pts',(-37.4438793364595,17.414842976684,-2.5));
#40011=CARTESIAN_POINT('Ctrl Pts',(-37.4423681010022,17.4184727323592,-2.5));
#40012=CARTESIAN_POINT('Ctrl Pts',(-37.4419797097032,17.4194055886623,-2.5));
#40013=CARTESIAN_POINT('Ctrl Pts',(-37.4415957390488,17.4203409106205,-2.5));
#40014=CARTESIAN_POINT('Ctrl Pts',(-37.4412162067833,17.4212787088996,-2.5));
#40015=CARTESIAN_POINT('Ctrl Pts',(-37.4397392352041,17.4249282046903,-2.5));
#40016=CARTESIAN_POINT('Ctrl Pts',(-37.4383296884591,17.4286145658692,-2.5));
#40017=CARTESIAN_POINT('Ctrl Pts',(-37.4369877690662,17.4323407425511,-2.5));
#40018=CARTESIAN_POINT('Ctrl Pts',(-37.4366431285229,17.4332977236953,-2.5));
#40019=CARTESIAN_POINT('Ctrl Pts',(-37.4363033603984,17.4342562299466,-2.5));
#40020=CARTESIAN_POINT('Ctrl Pts',(-37.4359684866688,17.4352161447217,-2.5));
#40021=CARTESIAN_POINT('Ctrl Pts',(-37.4346652921558,17.438951748794,-2.5));
#40022=CARTESIAN_POINT('Ctrl Pts',(-37.433437206174,17.4427059852574,-2.5));
#40023=CARTESIAN_POINT('Ctrl Pts',(-37.4322857798653,17.4464706373921,-2.5));
#40024=CARTESIAN_POINT('Ctrl Pts',(-37.4305413739693,17.4521740691535,-2.5));
#40025=CARTESIAN_POINT('Ctrl Pts',(-37.4289695650201,17.4579096521343,-2.5));
#40026=CARTESIAN_POINT('Ctrl Pts',(-37.4275674674098,17.463680867276,-2.5));
#40027=CARTESIAN_POINT('Ctrl Pts',(-37.4266455315817,17.4674756744075,-2.5));
#40028=CARTESIAN_POINT('Ctrl Pts',(-37.4257972794458,17.4712848537314,-2.5));
#40029=CARTESIAN_POINT('Ctrl Pts',(-37.4250221759071,17.4751083128213,-2.5));
#40030=CARTESIAN_POINT('Ctrl Pts',(-37.4230720543668,17.4847279436923,-2.5));
#40031=CARTESIAN_POINT('Ctrl Pts',(-37.4215850091917,17.4944379732078,-2.5));
#40032=CARTESIAN_POINT('Ctrl Pts',(-37.4205659366519,17.5042392904026,-2.5));
#40033=CARTESIAN_POINT('Ctrl Pts',(-37.4199448505089,17.5102128222722,-2.5));
#40034=CARTESIAN_POINT('Ctrl Pts',(-37.4194975446597,17.516221303522,-2.5));
#40035=CARTESIAN_POINT('Ctrl Pts',(-37.4192282868926,17.5222635707283,-2.5));
#40036=CARTESIAN_POINT('Ctrl Pts',(-37.4190560419298,17.5261288263199,-2.5));
#40037=CARTESIAN_POINT('Ctrl Pts',(-37.4189571461659,17.5300000552258,-2.5));
#40038=CARTESIAN_POINT('Ctrl Pts',(-37.4189314692081,17.5338661094116,-2.5));
#40039=CARTESIAN_POINT('Ctrl Pts',(-16.9340264307573,17.163528852123,6.73969634090002));
#40040=CARTESIAN_POINT('Ctrl Pts',(-16.9457712867961,17.2557485214382,6.26075296190838));
#40041=CARTESIAN_POINT('Ctrl Pts',(-17.4245878781802,17.16390605946,6.24262002709426));
#40042=CARTESIAN_POINT('Ctrl Pts',(-16.9238487697737,17.1121753468508,6.73379116642023));
#40043=CARTESIAN_POINT('Ctrl Pts',(-16.9318068964855,17.2064962780678,6.25102883540689));
#40044=CARTESIAN_POINT('Ctrl Pts',(-17.420771254245,17.144754794966,6.23883889336594));
#40045=CARTESIAN_POINT('Ctrl Pts',(-16.9188836705717,17.0606673879271,6.72780634103384));
#40046=CARTESIAN_POINT('Ctrl Pts',(-16.9228736444101,17.1565405083055,6.24116580803177));
#40047=CARTESIAN_POINT('Ctrl Pts',(-17.4189093402838,17.1255458393,6.23504636936957));
#40048=CARTESIAN_POINT('Ctrl Pts',(-16.9189456649685,16.983243156343,6.7187202593339));
#40049=CARTESIAN_POINT('Ctrl Pts',(-16.9168638503772,17.0804387429173,6.22614064079103));
#40050=CARTESIAN_POINT('Ctrl Pts',(-17.4189325924229,17.0966716564302,6.22934558931084));
#40051=CARTESIAN_POINT('Ctrl Pts',(-16.9202265012116,16.9574044014087,6.7156730067294));
#40052=CARTESIAN_POINT('Ctrl Pts',(-16.9161095341114,17.0547943482532,6.22107753461143));
#40053=CARTESIAN_POINT('Ctrl Pts',(-17.4194128979399,17.0870354499882,6.22744306296841));
#40054=CARTESIAN_POINT('Ctrl Pts',(-16.9240802930149,16.9185992377109,6.71107449121992));
#40055=CARTESIAN_POINT('Ctrl Pts',(-16.9169275550253,17.0160227636108,6.21342265905803));
#40056=CARTESIAN_POINT('Ctrl Pts',(-17.4208580798572,17.0725635360787,6.22458579775681));
#40057=CARTESIAN_POINT('Ctrl Pts',(-16.9256893119182,16.905644695499,6.70953565876855));
#40058=CARTESIAN_POINT('Ctrl Pts',(-16.9175289419495,17.0030164596971,6.21085475684852));
#40059=CARTESIAN_POINT('Ctrl Pts',(-17.4214614628586,17.0677322859808,6.22363193892933));
#40060=CARTESIAN_POINT('Ctrl Pts',(-16.9295597285367,16.8797683534593,6.70645460032402));
#40061=CARTESIAN_POINT('Ctrl Pts',(-16.919402781573,16.9769365576265,6.20570566617719));
#40062=CARTESIAN_POINT('Ctrl Pts',(-17.4229128606045,17.0580819710591,6.22172662707637));
#40063=CARTESIAN_POINT('Ctrl Pts',(-16.9318080465975,16.8669299669448,6.70492231261218));
#40064=CARTESIAN_POINT('Ctrl Pts',(-16.9206699203638,16.9639474234362,6.20314115387546));
#40065=CARTESIAN_POINT('Ctrl Pts',(-17.4237559870977,17.0532940171532,6.2207813164412));
#40066=CARTESIAN_POINT('Ctrl Pts',(-16.9445834894833,16.8032276683107,6.69730199287355));
#40067=CARTESIAN_POINT('Ctrl Pts',(-16.928658984358,16.8990583262999,6.1903297620293));
#40068=CARTESIAN_POINT('Ctrl Pts',(-17.4285467632928,17.0295367820529,6.2160908019868));
#40069=CARTESIAN_POINT('Ctrl Pts',(-16.9596689585237,16.7538180319705,6.69133567597977));
#40070=CARTESIAN_POINT('Ctrl Pts',(-16.9402496119177,16.8481169540716,6.18027214203455));
#40071=CARTESIAN_POINT('Ctrl Pts',(-17.4342038179283,17.0111096783419,6.21245264308723));
#40072=CARTESIAN_POINT('Ctrl Pts',(-16.9845527746887,16.6939788697473,6.6840528001532));
#40073=CARTESIAN_POINT('Ctrl Pts',(-16.9613133035777,16.7857105312913,6.16795091749546));
#40074=CARTESIAN_POINT('Ctrl Pts',(-17.4435352591956,16.9887926775086,6.20804648157282));
#40075=CARTESIAN_POINT('Ctrl Pts',(-16.9898335783274,16.6821080424272,6.68260507125331));
#40076=CARTESIAN_POINT('Ctrl Pts',(-16.9658750845434,16.7732516839765,6.16549110248884));
#40077=CARTESIAN_POINT('Ctrl Pts',(-17.4455155553034,16.984365439009,6.2071723888559));
#40078=CARTESIAN_POINT('Ctrl Pts',(-17.0010129029441,16.6585634598165,6.6797280266418));
#40079=CARTESIAN_POINT('Ctrl Pts',(-16.9756875213553,16.7484542773758,6.16059522156661));
#40080=CARTESIAN_POINT('Ctrl Pts',(-17.4497078084659,16.9755844415616,6.20543871087201));
#40081=CARTESIAN_POINT('Ctrl Pts',(-17.0069205341199,16.6468728289804,6.67829663781084));
#40082=CARTESIAN_POINT('Ctrl Pts',(-16.9809474116785,16.7360985023473,6.15815575665741));
#40083=CARTESIAN_POINT('Ctrl Pts',(-17.4519231707424,16.9712243839561,6.20457788202832));
#40084=CARTESIAN_POINT('Ctrl Pts',(-17.0255319975721,16.6122139276746,6.67404499554267));
#40085=CARTESIAN_POINT('Ctrl Pts',(-16.9977536936298,16.6993085573344,6.15089212651984));
#40086=CARTESIAN_POINT('Ctrl Pts',(-17.4589024581334,16.9582981905475,6.20202579645239));
#40087=CARTESIAN_POINT('Ctrl Pts',(-17.0389887268156,16.5898976324254,6.67129663775293));
#40088=CARTESIAN_POINT('Ctrl Pts',(-17.0101778412151,16.6754791025347,6.14618735335466));
#40089=CARTESIAN_POINT('Ctrl Pts',(-17.4639487418597,16.9499751842962,6.20038254205175));
#40090=CARTESIAN_POINT('Ctrl Pts',(-17.0824066515609,16.5252426617237,6.66330736417787));
#40091=CARTESIAN_POINT('Ctrl Pts',(-17.051127346388,16.6058793480108,6.13244591192685));
#40092=CARTESIAN_POINT('Ctrl Pts',(-17.4802304556663,16.925861531581,6.19562165821438));
#40093=CARTESIAN_POINT('Ctrl Pts',(-17.1153868669716,16.4851763244393,6.65831969837799));
#40094=CARTESIAN_POINT('Ctrl Pts',(-17.0831880908469,16.5622697417389,6.12383584060727));
#40095=CARTESIAN_POINT('Ctrl Pts',(-17.4925980312227,16.9109182299925,6.19267132448229));
#40096=CARTESIAN_POINT('Ctrl Pts',(-17.1571321085461,16.443595731894,6.65311644401699));
#40097=CARTESIAN_POINT('Ctrl Pts',(-17.1247289364465,16.5166242121387,6.11482380635895));
#40098=CARTESIAN_POINT('Ctrl Pts',(-17.5082525086683,16.8954100189695,6.18960945774325));
#40099=CARTESIAN_POINT('Ctrl Pts',(-17.1618355598308,16.4390246579602,6.6525440228328));
#40100=CARTESIAN_POINT('Ctrl Pts',(-17.1294344256378,16.5115867952363,6.11382924294728));
#40101=CARTESIAN_POINT('Ctrl Pts',(-17.5100163000558,16.8937051501344,6.18927285662447));
#40102=CARTESIAN_POINT('Ctrl Pts',(-17.171374097915,16.4299815745484,6.65141081135807));
#40103=CARTESIAN_POINT('Ctrl Pts',(-17.1390037634447,16.5016077877741,6.11185903561698));
#40104=CARTESIAN_POINT('Ctrl Pts',(-17.5135932548913,16.8903323645726,6.18860695003381));
#40105=CARTESIAN_POINT('Ctrl Pts',(-17.1762161790489,16.425503359408,6.65084924015553));
#40106=CARTESIAN_POINT('Ctrl Pts',(-17.1438746821593,16.4966594486413,6.11088205929252));
#40107=CARTESIAN_POINT('Ctrl Pts',(-17.5154090352215,16.8886621272269,6.18827718639005));
#40108=CARTESIAN_POINT('Ctrl Pts',(-17.190879548413,16.4122753689571,6.64918933918175));
#40109=CARTESIAN_POINT('Ctrl Pts',(-17.1586695817608,16.4820186331741,6.10799144696816));
#40110=CARTESIAN_POINT('Ctrl Pts',(-17.5209077944372,16.8837284797184,6.18730311070934));
#40111=CARTESIAN_POINT('Ctrl Pts',(-17.2008371206551,16.4037311294511,6.64811568767107));
#40112=CARTESIAN_POINT('Ctrl Pts',(-17.1687645001098,16.4725403371964,6.10612009770977));
#40113=CARTESIAN_POINT('Ctrl Pts',(-17.5246418887157,16.8805417313108,6.18667393440136));
#40114=CARTESIAN_POINT('Ctrl Pts',(-17.2312453506019,16.3789058423747,6.64499241842953));
#40115=CARTESIAN_POINT('Ctrl Pts',(-17.1997603324787,16.4449156410009,6.100666010302));
#40116=CARTESIAN_POINT('Ctrl Pts',(-17.5360449694744,16.8712825880367,6.18484585360074));
#40117=CARTESIAN_POINT('Ctrl Pts',(-17.2522302391352,16.3634303224513,6.64304026443391));
#40118=CARTESIAN_POINT('Ctrl Pts',(-17.2213294853766,16.4276216694408,6.09725157157484));
#40119=CARTESIAN_POINT('Ctrl Pts',(-17.5439143065422,16.8655106243265,6.18370626479344));
#40120=CARTESIAN_POINT('Ctrl Pts',(-17.2956019395641,16.3345930464113,6.63939537781673));
#40121=CARTESIAN_POINT('Ctrl Pts',(-17.2662656597083,16.3952572162235,6.09086168929334));
#40122=CARTESIAN_POINT('Ctrl Pts',(-17.5601786937626,16.8547550179788,6.18158272950716));
#40123=CARTESIAN_POINT('Ctrl Pts',(-17.3179887637184,16.3212313140015,6.63770263755943));
#40124=CARTESIAN_POINT('Ctrl Pts',(-17.2896291828443,16.3801970928505,6.08788829082891));
#40125=CARTESIAN_POINT('Ctrl Pts',(-17.5685737507052,16.8497713855231,6.18059878503843));
#40126=CARTESIAN_POINT('Ctrl Pts',(-17.3526333624528,16.3027934739649,6.63536298725943));
#40127=CARTESIAN_POINT('Ctrl Pts',(-17.3260026650614,16.3593493456032,6.08377221168955));
#40128=CARTESIAN_POINT('Ctrl Pts',(-17.5815654787338,16.8428944620486,6.17924103827948));
#40129=CARTESIAN_POINT('Ctrl Pts',(-17.364359267792,16.296915463442,6.63461640073939));
#40130=CARTESIAN_POINT('Ctrl Pts',(-17.3383566078206,16.3526877545169,6.08245697912365));
#40131=CARTESIAN_POINT('Ctrl Pts',(-17.5859626904173,16.8407020762296,6.17880818414767));
#40132=CARTESIAN_POINT('Ctrl Pts',(-17.3822192836592,16.2885072643732,6.6335476194421));
#40133=CARTESIAN_POINT('Ctrl Pts',(-17.3572223204219,16.3431449083558,6.08057288538689));
#40134=CARTESIAN_POINT('Ctrl Pts',(-17.5926601988439,16.8375659857744,6.17818900950262));
#40135=CARTESIAN_POINT('Ctrl Pts',(-17.3882178337638,16.285772701414,6.63319987789834));
#40136=CARTESIAN_POINT('Ctrl Pts',(-17.3635686188785,16.3400380551801,6.07995948320997));
#40137=CARTESIAN_POINT('Ctrl Pts',(-17.5949096533811,16.8365460418669,6.17798763667366));
#40138=CARTESIAN_POINT('Ctrl Pts',(-17.4003064009864,16.2804414700918,6.6325216769544));
#40139=CARTESIAN_POINT('Ctrl Pts',(-17.3763747964082,16.3339762671101,6.07876267287232));
#40140=CARTESIAN_POINT('Ctrl Pts',(-17.5994428679428,16.8345575960637,6.17759504747957));
#40141=CARTESIAN_POINT('Ctrl Pts',(-17.4064014619839,16.2778429556048,6.63219098038768));
#40142=CARTESIAN_POINT('Ctrl Pts',(-17.3828399484087,16.3310193192068,6.07817886727278));
#40143=CARTESIAN_POINT('Ctrl Pts',(-17.6017285156952,16.8335883975106,6.17740369356977));
#40144=CARTESIAN_POINT('Ctrl Pts',(-17.4613673391331,16.2552073371804,6.6293092707837));
#40145=CARTESIAN_POINT('Ctrl Pts',(-17.4412943532773,16.305207075037,6.07308262169252));
#40146=CARTESIAN_POINT('Ctrl Pts',(-17.6223407123812,16.8251457010694,6.17573680811258));
#40147=CARTESIAN_POINT('Ctrl Pts',(-17.5114824250486,16.2401548090555,6.62738600694331));
#40148=CARTESIAN_POINT('Ctrl Pts',(-17.4949832638486,16.2879639917577,6.06967823010323));
#40149=CARTESIAN_POINT('Ctrl Pts',(-17.6411338750825,16.8195313396363,6.17462833554231));
#40150=CARTESIAN_POINT('Ctrl Pts',(-17.5884810370651,16.2249404862174,6.62544067878907));
#40151=CARTESIAN_POINT('Ctrl Pts',(-17.5778953266643,16.270488978075,6.06622804728844));
#40152=CARTESIAN_POINT('Ctrl Pts',(-17.6700083560242,16.8138566171136,6.17350794556827));
#40153=CARTESIAN_POINT('Ctrl Pts',(-17.61445379365,16.2211054438284,6.6249498806517));
#40154=CARTESIAN_POINT('Ctrl Pts',(-17.6059331605785,16.2660757431219,6.06535671936452));
#40155=CARTESIAN_POINT('Ctrl Pts',(-17.6797481384879,16.8124261864561,6.17322552820585));
#40156=CARTESIAN_POINT('Ctrl Pts',(-17.6538857988551,16.217259998137,6.62445766257136));
#40157=CARTESIAN_POINT('Ctrl Pts',(-17.6485546296303,16.2616476106312,6.06448245014227));
#40158=CARTESIAN_POINT('Ctrl Pts',(-17.6945351416054,16.8109918968226,6.17294234894575));
#40159=CARTESIAN_POINT('Ctrl Pts',(-17.6671432193907,16.2162960247729,6.6243342451152));
#40160=CARTESIAN_POINT('Ctrl Pts',(-17.6628934486627,16.2605370299517,6.06426318242413));
#40161=CARTESIAN_POINT('Ctrl Pts',(-17.6995066741152,16.810632347174,6.1728713611891));
#40162=CARTESIAN_POINT('Ctrl Pts',(-17.6935540371893,16.2150298143844,6.62417212417057));
#40163=CARTESIAN_POINT('Ctrl Pts',(-17.691468213857,16.2590779435578,6.06397510741069));
#40164=CARTESIAN_POINT('Ctrl Pts',(-17.7094107303948,16.8101600586753,6.17277811481509));
#40165=CARTESIAN_POINT('Ctrl Pts',(-17.7067266210675,16.2147239146772,6.62413295366647));
#40166=CARTESIAN_POINT('Ctrl Pts',(-17.7057234775305,16.2587254085436,6.06390550458979));
#40167=CARTESIAN_POINT('Ctrl Pts',(-17.7143504495434,16.8100459686567,6.1727555894295));
#40168=CARTESIAN_POINT('Ctrl Pts',(-17.7724284272708,16.2148007635293,6.6241427921321));
#40169=CARTESIAN_POINT('Ctrl Pts',(-17.7768280969853,16.2588139364961,6.06392298312376));
#40170=CARTESIAN_POINT('Ctrl Pts',(-17.7389886268855,16.8100746189498,6.17276124600583));
#40171=CARTESIAN_POINT('Ctrl Pts',(-17.8244788813812,16.2199564028495,6.62480342778294));
#40172=CARTESIAN_POINT('Ctrl Pts',(-17.8331128420917,16.2647554475499,6.06509604654469));
#40173=CARTESIAN_POINT('Ctrl Pts',(-17.7585075492867,16.8119976109921,6.17314091232356));
#40174=CARTESIAN_POINT('Ctrl Pts',(-17.8889031485325,16.2327695523612,6.62644171019872));
#40175=CARTESIAN_POINT('Ctrl Pts',(-17.90254892953,16.2794864647711,6.06800446787037));
#40176=CARTESIAN_POINT('Ctrl Pts',(-17.7826666468153,16.816776749508,6.17408448249046));
#40177=CARTESIAN_POINT('Ctrl Pts',(-17.9017557691567,16.2356534961519,6.62681033151498));
#40178=CARTESIAN_POINT('Ctrl Pts',(-17.9163762099596,16.2827975605751,6.06865819473137));
#40179=CARTESIAN_POINT('Ctrl Pts',(-17.7874863810826,16.81785241274,6.1742968562754));
#40180=CARTESIAN_POINT('Ctrl Pts',(-17.9273953632276,16.2420759339317,6.62763082558797));
#40181=CARTESIAN_POINT('Ctrl Pts',(-17.9439205439042,16.2901643089726,6.07011265017177));
#40182=CARTESIAN_POINT('Ctrl Pts',(-17.797101226854,16.82024789507,6.17476980880739));
#40183=CARTESIAN_POINT('Ctrl Pts',(-17.9401902056257,16.2456190784938,6.62808328938417));
#40184=CARTESIAN_POINT('Ctrl Pts',(-17.9576446533942,16.294224513599,6.07091427748269));
#40185=CARTESIAN_POINT('Ctrl Pts',(-17.8018992926118,16.8215694340713,6.17503072712393));
#40186=CARTESIAN_POINT('Ctrl Pts',(-17.9780466892305,16.2571128882123,6.62955018787334));
#40187=CARTESIAN_POINT('Ctrl Pts',(-17.9981679747951,16.3073767581212,6.07351099350535));
#40188=CARTESIAN_POINT('Ctrl Pts',(-17.8160954773958,16.8258564334959,6.17587713171108));
#40189=CARTESIAN_POINT('Ctrl Pts',(-18.0027258637711,16.2659587403489,6.63067809312904));
#40190=CARTESIAN_POINT('Ctrl Pts',(-18.0244924260245,16.317478878484,6.07550550765576));
#40191=CARTESIAN_POINT('Ctrl Pts',(-17.825350164657,16.8291557994221,6.17652854268134));
#40192=CARTESIAN_POINT('Ctrl Pts',(-18.0751331263037,16.2959506337827,6.63449608491444));
#40193=CARTESIAN_POINT('Ctrl Pts',(-18.1013159720922,16.3516027063543,6.08224275242306));
#40194=CARTESIAN_POINT('Ctrl Pts',(-17.852502890817,16.8403422289135,6.17873713762098));
#40195=CARTESIAN_POINT('Ctrl Pts',(-18.1212467327399,16.3205175212379,6.63761658916437));
#40196=CARTESIAN_POINT('Ctrl Pts',(-18.1497601127687,16.3794086658638,6.0877326275894));
#40197=CARTESIAN_POINT('Ctrl Pts',(-17.8697955008785,16.8495051762018,6.18054622594794));
#40198=CARTESIAN_POINT('Ctrl Pts',(-18.1706160636699,16.3534706885993,6.6417813765152));
#40199=CARTESIAN_POINT('Ctrl Pts',(-18.2009972681976,16.4164599843371,6.09504786204832));
#40200=CARTESIAN_POINT('Ctrl Pts',(-17.8883089893406,16.8617959232122,6.18297285203741));
#40201=CARTESIAN_POINT('Ctrl Pts',(-18.1760670536863,16.3572075290665,6.64225340483513));
#40202=CARTESIAN_POINT('Ctrl Pts',(-18.2066322253776,16.4206486705888,6.09587485615456));
#40203=CARTESIAN_POINT('Ctrl Pts',(-17.8903531105129,16.863189672331,6.18324802717289));
#40204=CARTESIAN_POINT('Ctrl Pts',(-18.1868377701863,16.3647884998207,6.64321046159106));
#40205=CARTESIAN_POINT('Ctrl Pts',(-18.2177440408947,16.4291367290659,6.09755069767437));
#40206=CARTESIAN_POINT('Ctrl Pts',(-17.8943921317318,16.8660171798007,6.18380627667459));
#40207=CARTESIAN_POINT('Ctrl Pts',(-18.1921652410117,16.3686376965469,6.64369613249193));
#40208=CARTESIAN_POINT('Ctrl Pts',(-18.2232288896621,16.4334416698043,6.09840064450838));
#40209=CARTESIAN_POINT('Ctrl Pts',(-17.8963899309271,16.8674528346187,6.18408972547016));
#40210=CARTESIAN_POINT('Ctrl Pts',(-18.2079758853082,16.380359521441,6.64517424754474));
#40211=CARTESIAN_POINT('Ctrl Pts',(-18.2394674114616,16.4465321648978,6.10098516902028));
#40212=CARTESIAN_POINT('Ctrl Pts',(-17.902318925834,16.8718247643677,6.18495289829289));
#40213=CARTESIAN_POINT('Ctrl Pts',(-18.2182873888224,16.3884062672933,6.64618778634462));
#40214=CARTESIAN_POINT('Ctrl Pts',(-18.250014828929,16.4555003709746,6.10275580857727));
#40215=CARTESIAN_POINT('Ctrl Pts',(-17.9061857359879,16.8748259873231,6.18554544534619));
#40216=CARTESIAN_POINT('Ctrl Pts',(-18.2485461467234,16.4132319441657,6.6493107176117));
#40217=CARTESIAN_POINT('Ctrl Pts',(-18.2808046004885,16.4830834508249,6.10820167945361));
#40218=CARTESIAN_POINT('Ctrl Pts',(-17.917532774601,16.884085261647,6.18737355202065));
#40219=CARTESIAN_POINT('Ctrl Pts',(-18.2678192302634,16.4306946934602,6.65150224599118));
#40220=CARTESIAN_POINT('Ctrl Pts',(-18.3002353052696,16.5024028462849,6.11201600815278));
#40221=CARTESIAN_POINT('Ctrl Pts',(-17.9247601784908,16.8905983462382,6.18865946417705));
#40222=CARTESIAN_POINT('Ctrl Pts',(-18.304585320563,16.4674258171909,6.65609825686814));
#40223=CARTESIAN_POINT('Ctrl Pts',(-18.3369000788844,16.5428190986578,6.11999559900783));
#40224=CARTESIAN_POINT('Ctrl Pts',(-17.9385474613616,16.9042978717687,6.19136423273484));
#40225=CARTESIAN_POINT('Ctrl Pts',(-18.32207835827,16.4866941560064,6.65850274672427));
#40226=CARTESIAN_POINT('Ctrl Pts',(-18.3541350222299,16.5639050113827,6.12415870039582));
#40227=CARTESIAN_POINT('Ctrl Pts',(-17.9451073556682,16.9114842972485,6.19278308608398));
#40228=CARTESIAN_POINT('Ctrl Pts',(-18.3469582555341,16.5169758809527,6.6622690907101));
#40229=CARTESIAN_POINT('Ctrl Pts',(-18.3783360711151,16.5968717741023,6.13066749977414));
#40230=CARTESIAN_POINT('Ctrl Pts',(-17.9544373101362,16.9227782767883,6.1950129151889));
#40231=CARTESIAN_POINT('Ctrl Pts',(-18.3550268290823,16.5273031516405,6.66355157018222));
#40232=CARTESIAN_POINT('Ctrl Pts',(-18.3861205298441,16.6080723020181,6.13287887823903));
#40233=CARTESIAN_POINT('Ctrl Pts',(-17.9574630272311,16.9266299573578,6.19577337251102));
#40234=CARTESIAN_POINT('Ctrl Pts',(-18.3706915223259,16.5484153134749,6.66616886023153));
#40235=CARTESIAN_POINT('Ctrl Pts',(-18.4011144492354,16.6308981776041,6.13738550954182));
#40236=CARTESIAN_POINT('Ctrl Pts',(-17.9633372878401,16.934503971749,6.19732798011414));
#40237=CARTESIAN_POINT('Ctrl Pts',(-18.3782309891514,16.5591238170816,6.66749420161781));
#40238=CARTESIAN_POINT('Ctrl Pts',(-18.4082702147513,16.6424396756498,6.13966420751237));
#40239=CARTESIAN_POINT('Ctrl Pts',(-17.9661645847443,16.9384978169065,6.19811650573006));
#40240=CARTESIAN_POINT('Ctrl Pts',(-18.4144652239087,16.6133698763481,6.67419609590586));
#40241=CARTESIAN_POINT('Ctrl Pts',(-18.4422698693699,16.7005708871118,6.15114135485145));
#40242=CARTESIAN_POINT('Ctrl Pts',(-17.9797524369468,16.9587293525346,6.20211092300537));
#40243=CARTESIAN_POINT('Ctrl Pts',(-18.4388454391431,16.6590429087733,6.67980148969806));
#40244=CARTESIAN_POINT('Ctrl Pts',(-18.4642277040733,16.7490077862942,6.16070450371041));
#40245=CARTESIAN_POINT('Ctrl Pts',(-17.9888950132745,16.975763316277,6.20547402703715));
#40246=CARTESIAN_POINT('Ctrl Pts',(-18.4636539969267,16.7189339970101,6.68708985334279));
#40247=CARTESIAN_POINT('Ctrl Pts',(-18.4853233274594,16.811806410725,6.17310316266067));
#40248=CARTESIAN_POINT('Ctrl Pts',(-17.9981982137564,16.9980996869273,6.20988401283525));
#40249=CARTESIAN_POINT('Ctrl Pts',(-18.4683298236966,16.7310534611065,6.68856175184365));
#40250=CARTESIAN_POINT('Ctrl Pts',(-18.4892098083346,16.8244336013383,6.17559621456002));
#40251=CARTESIAN_POINT('Ctrl Pts',(-17.9999516535622,17.0026196231967,6.21077640735487));
#40252=CARTESIAN_POINT('Ctrl Pts',(-18.4771016880877,16.7555788545222,6.69153398968095));
#40253=CARTESIAN_POINT('Ctrl Pts',(-18.4963362162636,16.8498937457125,6.18062294324687));
#40254=CARTESIAN_POINT('Ctrl Pts',(-18.0032410966494,17.0117663114213,6.21258228557033));
#40255=CARTESIAN_POINT('Ctrl Pts',(-18.4812032176816,16.768003161379,6.69303654757409));
#40256=CARTESIAN_POINT('Ctrl Pts',(-18.4995813969772,16.8627446305905,6.18316016026802));
#40257=CARTESIAN_POINT('Ctrl Pts',(-18.0047791706222,17.0163999130041,6.21349712162379));
#40258=CARTESIAN_POINT('Ctrl Pts',(-18.4925821723103,16.8055904468549,6.69757219653477));
#40259=CARTESIAN_POINT('Ctrl Pts',(-18.5082993306589,16.9014403837458,6.19080006401661));
#40260=CARTESIAN_POINT('Ctrl Pts',(-18.0090462865719,17.030417917443,6.21626476912844));
#40261=CARTESIAN_POINT('Ctrl Pts',(-18.4988883625265,16.8308948943173,6.70061244451219));
#40262=CARTESIAN_POINT('Ctrl Pts',(-18.5127456724536,16.9273229004005,6.19591018385897));
#40263=CARTESIAN_POINT('Ctrl Pts',(-18.0114111023906,17.0398550445677,6.21812799020613));
#40264=CARTESIAN_POINT('Ctrl Pts',(-18.5089809331914,16.8819886542203,6.70672283022605));
#40265=CARTESIAN_POINT('Ctrl Pts',(-18.5189743166287,16.979189821447,6.20615053976939));
#40266=CARTESIAN_POINT('Ctrl Pts',(-18.0151958167961,17.0589100232433,6.22189011372466));
#40267=CARTESIAN_POINT('Ctrl Pts',(-18.5127673002267,16.9077779664103,6.70979297341625));
#40268=CARTESIAN_POINT('Ctrl Pts',(-18.5207667892184,17.0051710504343,6.21128014890083));
#40269=CARTESIAN_POINT('Ctrl Pts',(-18.0166157093195,17.0685278759537,6.22378901639444));
#40270=CARTESIAN_POINT('Ctrl Pts',(-18.51653149759,16.9468304737568,6.71441949514766));
#40271=CARTESIAN_POINT('Ctrl Pts',(-18.5214756795303,17.0442515895124,6.21899602293492));
#40272=CARTESIAN_POINT('Ctrl Pts',(-18.0180272756984,17.0830920314624,6.22666449334457));
#40273=CARTESIAN_POINT('Ctrl Pts',(-18.5174610536025,16.9598642331123,6.71595985693076));
#40274=CARTESIAN_POINT('Ctrl Pts',(-18.5213812087045,17.0572310011096,6.22155861565454));
#40275=CARTESIAN_POINT('Ctrl Pts',(-18.0183758583191,17.0879528012551,6.22762418039891));
#40276=CARTESIAN_POINT('Ctrl Pts',(-18.5186722537819,16.9858429775025,6.71902258829226));
#40277=CARTESIAN_POINT('Ctrl Pts',(-18.5205481857505,17.0830017716537,6.22664667288122));
#40278=CARTESIAN_POINT('Ctrl Pts',(-18.0188300652425,17.0976412129467,6.22953701389521));
#40279=CARTESIAN_POINT('Ctrl Pts',(-18.5189557766232,16.9988067822409,6.7205471885435));
#40280=CARTESIAN_POINT('Ctrl Pts',(-18.5198112791957,17.0958122032461,6.22917590299987));
#40281=CARTESIAN_POINT('Ctrl Pts',(-18.0189363807851,17.1024758738013,6.23049154612614));
#40282=CARTESIAN_POINT('Ctrl Pts',(-18.5187872011184,17.0634999017462,6.72813660661715));
#40283=CARTESIAN_POINT('Ctrl Pts',(-18.5145769287806,17.1593013447143,6.24171089431925));
#40284=CARTESIAN_POINT('Ctrl Pts',(-18.0188731754452,17.1266021766945,6.23525492755391));
#40285=CARTESIAN_POINT('Ctrl Pts',(-18.5136215290469,17.1148550403912,6.73410108134611));
#40286=CARTESIAN_POINT('Ctrl Pts',(-18.5054607669974,17.2090806073982,6.25153907298411));
#40287=CARTESIAN_POINT('Ctrl Pts',(-18.0169360523498,17.1457541379813,6.23903619885366));
#40288=CARTESIAN_POINT('Ctrl Pts',(-18.5008049385582,17.178543935026,6.74142244098528));
#40289=CARTESIAN_POINT('Ctrl Pts',(-18.4879750956344,17.2700726310465,6.26358104534826));
#40290=CARTESIAN_POINT('Ctrl Pts',(-18.0121298155278,17.1695056335805,6.24372558012852));
#40291=CARTESIAN_POINT('Ctrl Pts',(-18.4979208133035,17.1912562328885,6.74287997549926));
#40292=CARTESIAN_POINT('Ctrl Pts',(-18.4841868810595,17.2821639022754,6.26596828789697));
#40293=CARTESIAN_POINT('Ctrl Pts',(-18.0110482760138,17.1742464268863,6.24466157960121));
#40294=CARTESIAN_POINT('Ctrl Pts',(-18.4914973495927,17.2166287983916,6.74578145608233));
#40295=CARTESIAN_POINT('Ctrl Pts',(-18.4759981394833,17.3062060478485,6.27071505370745));
#40296=CARTESIAN_POINT('Ctrl Pts',(-18.0086394683647,17.1837085953516,6.24652974472097));
#40297=CARTESIAN_POINT('Ctrl Pts',(-18.4879753251126,17.2292171975606,6.74721717444261));
#40298=CARTESIAN_POINT('Ctrl Pts',(-18.4716211015665,17.3180893500614,6.27306123585199));
#40299=CARTESIAN_POINT('Ctrl Pts',(-18.0073187104683,17.1884031726981,6.24745661953651));
#40300=CARTESIAN_POINT('Ctrl Pts',(-18.4765353931923,17.2665465103297,6.75146357848355));
#40301=CARTESIAN_POINT('Ctrl Pts',(-18.4577271501903,17.3531629274733,6.27998599460963));
#40302=CARTESIAN_POINT('Ctrl Pts',(-18.0030287452838,17.2023243430448,6.25020514858282));
#40303=CARTESIAN_POINT('Ctrl Pts',(-18.4677297456344,17.2909162449736,6.75422091139731));
#40304=CARTESIAN_POINT('Ctrl Pts',(-18.4474068235007,17.3759132514684,6.28447770936899));
#40305=CARTESIAN_POINT('Ctrl Pts',(-17.9997266201643,17.2114124977806,6.25199947022725));
#40306=CARTESIAN_POINT('Ctrl Pts',(-18.4378487844442,17.3625079863937,6.76228026019661));
#40307=CARTESIAN_POINT('Ctrl Pts',(-18.4134691558281,17.4421491186173,6.29755500102144));
#40308=CARTESIAN_POINT('Ctrl Pts',(-17.9885212630024,17.2381110500616,6.25727070422638));
#40309=CARTESIAN_POINT('Ctrl Pts',(-18.413342249397,17.4082296127105,6.76737146292247));
#40310=CARTESIAN_POINT('Ctrl Pts',(-18.3868137642132,17.483931249389,6.30580426435083));
#40311=CARTESIAN_POINT('Ctrl Pts',(-17.979331323364,17.2551619032087,6.26063714282115));
#40312=CARTESIAN_POINT('Ctrl Pts',(-18.3693951615143,17.4736551525738,6.77458729194665));
#40313=CARTESIAN_POINT('Ctrl Pts',(-18.3405991802905,17.5430486220348,6.31747611462008));
#40314=CARTESIAN_POINT('Ctrl Pts',(-17.9628511456172,17.279560906992,6.26545436500358));
#40315=CARTESIAN_POINT('Ctrl Pts',(-18.3537632469114,17.4945975063259,6.77688492238546));
#40316=CARTESIAN_POINT('Ctrl Pts',(-18.3244286783927,17.5618163081471,6.32118151647404));
#40317=CARTESIAN_POINT('Ctrl Pts',(-17.9569891815114,17.2873709068913,6.26699633389272));
#40318=CARTESIAN_POINT('Ctrl Pts',(-18.3206591277799,17.5347184100098,6.78126667754031));
#40319=CARTESIAN_POINT('Ctrl Pts',(-18.2906282613387,17.5975559035035,6.32823777061752));
#40320=CARTESIAN_POINT('Ctrl Pts',(-17.9445751422903,17.3023331556006,6.26995040845338));
#40321=CARTESIAN_POINT('Ctrl Pts',(-18.3031766385638,17.5539118752031,6.78335243318941));
#40322=CARTESIAN_POINT('Ctrl Pts',(-18.2729880315817,17.6145513152006,6.33159326311853));
#40323=CARTESIAN_POINT('Ctrl Pts',(-17.9380192073362,17.3094909634119,6.27136361166745));
#40324=CARTESIAN_POINT('Ctrl Pts',(-18.2663596953146,17.590573120573,6.78731950209393));
#40325=CARTESIAN_POINT('Ctrl Pts',(-18.2362359266378,17.6468363652653,6.33796746842275));
#40326=CARTESIAN_POINT('Ctrl Pts',(-17.9242128511607,17.3231630449985,6.2740629618247));
#40327=CARTESIAN_POINT('Ctrl Pts',(-18.2470253297619,17.6080409781332,6.78920081264864));
#40328=CARTESIAN_POINT('Ctrl Pts',(-18.2171237375768,17.6621351487866,6.3409879868012));
#40329=CARTESIAN_POINT('Ctrl Pts',(-17.9169624698265,17.3296773557345,6.27534911606522));
#40330=CARTESIAN_POINT('Ctrl Pts',(-18.2166010903152,17.6329170950227,6.79186951328928));
#40331=CARTESIAN_POINT('Ctrl Pts',(-18.1872989485619,17.683828532514,6.34527102434781));
#40332=CARTESIAN_POINT('Ctrl Pts',(-17.9055533732547,17.3389544402554,6.27718073909949));
#40333=CARTESIAN_POINT('Ctrl Pts',(-18.2062168750825,17.6409916724233,6.79273390499216));
#40334=CARTESIAN_POINT('Ctrl Pts',(-18.1771687996823,17.6908479022576,6.34665689501433));
#40335=CARTESIAN_POINT('Ctrl Pts',(-17.9016592934025,17.3419657104848,6.27777526983833));
#40336=CARTESIAN_POINT('Ctrl Pts',(-18.1849835178449,17.656672005178,6.79440927725295));
#40337=CARTESIAN_POINT('Ctrl Pts',(-18.1565384222284,17.7044471017748,6.34934185568567));
#40338=CARTESIAN_POINT('Ctrl Pts',(-17.8936967872377,17.3478134207786,6.27892981368751));
#40339=CARTESIAN_POINT('Ctrl Pts',(-18.1742117514745,17.6642209160496,6.79521418404731));
#40340=CARTESIAN_POINT('Ctrl Pts',(-18.1461128939455,17.7109787537895,6.35063143370503));
#40341=CARTESIAN_POINT('Ctrl Pts',(-17.8896573717566,17.3506286544074,6.27948563990098));
#40342=CARTESIAN_POINT('Ctrl Pts',(-18.1196129973381,17.7005236924937,6.7990781174034));
#40343=CARTESIAN_POINT('Ctrl Pts',(-18.0935526247991,17.7422665507531,6.35680874614416));
#40344=CARTESIAN_POINT('Ctrl Pts',(-17.8691828474184,17.3641671857882,6.2821586225467));
#40345=CARTESIAN_POINT('Ctrl Pts',(-18.073566038191,17.7250092175285,6.8016618385873));
#40346=CARTESIAN_POINT('Ctrl Pts',(-18.0497217046225,17.7632251779753,6.36094671689349));
#40347=CARTESIAN_POINT('Ctrl Pts',(-17.8519152345038,17.3732987063331,6.2839615061283));
#40348=CARTESIAN_POINT('Ctrl Pts',(-18.0130701585827,17.7499642230801,6.80428434438707));
#40349=CARTESIAN_POINT('Ctrl Pts',(-17.9926453915806,17.7844819967742,6.36514356115633));
#40350=CARTESIAN_POINT('Ctrl Pts',(-17.8292292752308,17.3826053354479,6.28579896230536));
#40351=CARTESIAN_POINT('Ctrl Pts',(-18.0008227990897,17.7546700742571,6.80477818859267));
#40352=CARTESIAN_POINT('Ctrl Pts',(-17.9811297306172,17.7884796711135,6.36593284278751));
#40353=CARTESIAN_POINT('Ctrl Pts',(-17.8246365175473,17.3843603279786,6.28614545960597));
#40354=CARTESIAN_POINT('Ctrl Pts',(-17.9760268452319,17.7635021372388,6.80570402970065));
#40355=CARTESIAN_POINT('Ctrl Pts',(-17.9578627436139,17.7959726092415,6.36741221252255));
#40356=CARTESIAN_POINT('Ctrl Pts',(-17.8153380323659,17.3876541288755,6.28679577184356));
#40357=CARTESIAN_POINT('Ctrl Pts',(-17.9634548231814,17.7676353220123,6.80613675524105));
#40358=CARTESIAN_POINT('Ctrl Pts',(-17.9460886325703,17.7994744891973,6.36810360689066));
#40359=CARTESIAN_POINT('Ctrl Pts',(-17.8106235240595,17.3891955494437,6.28710010252115));
#40360=CARTESIAN_POINT('Ctrl Pts',(-17.9254344120959,17.7790973746866,6.80733565050496));
#40361=CARTESIAN_POINT('Ctrl Pts',(-17.9105547741728,17.8091716890774,6.37001817548471));
#40362=CARTESIAN_POINT('Ctrl Pts',(-17.7963658737417,17.3934701994542,6.28794406889925));
#40363=CARTESIAN_POINT('Ctrl Pts',(-17.8999087430931,17.7854283478246,6.80799626184293));
#40364=CARTESIAN_POINT('Ctrl Pts',(-17.886766663715,17.8145173455381,6.37107359623513));
#40365=CARTESIAN_POINT('Ctrl Pts',(-17.7867937446671,17.3958312544259,6.28841022425892));
#40366=CARTESIAN_POINT('Ctrl Pts',(-17.8228126864582,17.8006160211639,6.80957942969772));
#40367=CARTESIAN_POINT('Ctrl Pts',(-17.8151219476809,17.8273163816643,6.37360057648762));
#40368=CARTESIAN_POINT('Ctrl Pts',(-17.7578827253461,17.4014953443393,6.28952851498163));
#40369=CARTESIAN_POINT('Ctrl Pts',(-17.7707282072719,17.8057036316249,6.81010758629701));
#40370=CARTESIAN_POINT('Ctrl Pts',(-17.7668735570122,17.8315930628393,6.37444494388912));
#40371=CARTESIAN_POINT('Ctrl Pts',(-17.7383510443547,17.4033927296949,6.28990312563806));
#40372=CARTESIAN_POINT('Ctrl Pts',(-17.7113425373793,17.8056309224566,6.81010002580354));
#40373=CARTESIAN_POINT('Ctrl Pts',(-17.7119066821582,17.8315319119423,6.37443287054956));
#40374=CARTESIAN_POINT('Ctrl Pts',(-17.7160814181658,17.4033655966885,6.28989776862753));
#40375=CARTESIAN_POINT('Ctrl Pts',(-17.7047330456674,17.8055415663399,6.81009073748399));
#40376=CARTESIAN_POINT('Ctrl Pts',(-17.7057888706203,17.8314568157848,6.37441804392472));
#40377=CARTESIAN_POINT('Ctrl Pts',(-17.7136028587132,17.4033322762928,6.28989119000853));
#40378=CARTESIAN_POINT('Ctrl Pts',(-17.6914916361947,17.8051984797874,6.81005506963536));
#40379=CARTESIAN_POINT('Ctrl Pts',(-17.6935317272033,17.8311684204133,6.37436110452697));
#40380=CARTESIAN_POINT('Ctrl Pts',(-17.7086373302776,17.4032043210795,6.28986592714545));
#40381=CARTESIAN_POINT('Ctrl Pts',(-17.6848569462331,17.8049443436771,6.81002864903746));
#40382=CARTESIAN_POINT('Ctrl Pts',(-17.6873896796574,17.8309547927005,6.37431892689686));
#40383=CARTESIAN_POINT('Ctrl Pts',(-17.7061493215936,17.4031095435898,6.28984721473285));
#40384=CARTESIAN_POINT('Ctrl Pts',(-17.6650316986901,17.8039394480878,6.80992416632294));
#40385=CARTESIAN_POINT('Ctrl Pts',(-17.669033565516,17.8301099792034,6.37415213097543));
#40386=CARTESIAN_POINT('Ctrl Pts',(-17.6987148534351,17.402734784112,6.28977322402055));
#40387=CARTESIAN_POINT('Ctrl Pts',(-17.65188297285,17.8029458235526,6.80982084423287));
#40388=CARTESIAN_POINT('Ctrl Pts',(-17.6568553794863,17.8292744610696,6.37398717028588));
#40389=CARTESIAN_POINT('Ctrl Pts',(-17.6937840817574,17.4023642144883,6.28970006053293));
#40390=CARTESIAN_POINT('Ctrl Pts',(-17.6126371335032,17.7990126660086,6.80941167670247));
#40391=CARTESIAN_POINT('Ctrl Pts',(-17.6204837103719,17.825965596934,6.37333388403476));
#40392=CARTESIAN_POINT('Ctrl Pts',(-17.6790668911251,17.4008973914905,6.28941045804156));
#40393=CARTESIAN_POINT('Ctrl Pts',(-17.5867398984557,17.7951231176127,6.80900689352775));
#40394=CARTESIAN_POINT('Ctrl Pts',(-17.596453210412,17.8226910680451,6.37268737676991));
#40395=CARTESIAN_POINT('Ctrl Pts',(-17.6693554286528,17.3994468177432,6.28912406372419));
#40396=CARTESIAN_POINT('Ctrl Pts',(-17.5354697949089,17.7848516081068,6.80793609188225));
#40397=CARTESIAN_POINT('Ctrl Pts',(-17.5487818608033,17.8140306147149,6.37097749843788));
#40398=CARTESIAN_POINT('Ctrl Pts',(-17.6501291396514,17.3956161693061,6.28836775888534));
#40399=CARTESIAN_POINT('Ctrl Pts',(-17.5100969352081,17.7784696191355,6.80727007507948));
#40400=CARTESIAN_POINT('Ctrl Pts',(-17.5251318472474,17.8086411999732,6.36991343826254));
#40401=CARTESIAN_POINT('Ctrl Pts',(-17.6406143159052,17.3932360814621,6.28789784576675));
#40402=CARTESIAN_POINT('Ctrl Pts',(-17.4724356982661,17.7670045961486,6.80607073498154));
#40403=CARTESIAN_POINT('Ctrl Pts',(-17.4899271035391,17.7989402787506,6.36799813494449));
#40404=CARTESIAN_POINT('Ctrl Pts',(-17.6264913542181,17.3889603296644,6.28705366185705));
#40405=CARTESIAN_POINT('Ctrl Pts',(-17.4599484159706,17.7628670210704,6.80563750504227));
#40406=CARTESIAN_POINT('Ctrl Pts',(-17.4782302202683,17.7954342534171,6.36730592213287));
#40407=CARTESIAN_POINT('Ctrl Pts',(-17.6218086213275,17.3874172771144,6.28674900896883));
#40408=CARTESIAN_POINT('Ctrl Pts',(-17.4351090516651,17.7539492007634,6.8047025599668));
#40409=CARTESIAN_POINT('Ctrl Pts',(-17.454917776984,17.7878675018479,6.36581197902636));
#40410=CARTESIAN_POINT('Ctrl Pts',(-17.6124938623285,17.384091480323,6.28609237961543));
#40411=CARTESIAN_POINT('Ctrl Pts',(-17.4227335316578,17.7491576061505,6.804199652638));
#40412=CARTESIAN_POINT('Ctrl Pts',(-17.4432789672747,17.7837963825994,6.36500819678485));
#40413=CARTESIAN_POINT('Ctrl Pts',(-17.6078530426073,17.38230451645,6.28573957004644));
#40414=CARTESIAN_POINT('Ctrl Pts',(-17.3618547466598,17.7238403969658,6.8015386718093));
#40415=CARTESIAN_POINT('Ctrl Pts',(-17.3858250678238,17.7622268875734,6.36074961922872));
#40416=CARTESIAN_POINT('Ctrl Pts',(-17.5850234902864,17.3728628177143,6.28387544637182));
#40417=CARTESIAN_POINT('Ctrl Pts',(-17.3158627238175,17.6991343295047,6.79893094285691));
#40418=CARTESIAN_POINT('Ctrl Pts',(-17.3420267744581,17.7410737731548,6.35657324986094));
#40419=CARTESIAN_POINT('Ctrl Pts',(-17.5677764852266,17.3636490384775,6.28205632202897));
#40420=CARTESIAN_POINT('Ctrl Pts',(-17.2508193911024,17.6555966201116,6.7942958684358));
#40421=CARTESIAN_POINT('Ctrl Pts',(-17.2793471455071,17.7035182827478,6.34915847411566));
#40422=CARTESIAN_POINT('Ctrl Pts',(-17.5433852397352,17.3474123674201,6.27885063163761));
#40423=CARTESIAN_POINT('Ctrl Pts',(-17.2298005184759,17.6399964301089,6.79262936990691));
#40424=CARTESIAN_POINT('Ctrl Pts',(-17.2589173832124,17.6899870750125,6.34648693741537));
#40425=CARTESIAN_POINT('Ctrl Pts',(-17.5355031559793,17.3415945569023,6.27770199105668));
#40426=CARTESIAN_POINT('Ctrl Pts',(-17.204378613571,17.619097401045,6.79038682430432));
#40427=CARTESIAN_POINT('Ctrl Pts',(-17.2340263963876,17.6717874399427,6.34289368883238));
#40428=CARTESIAN_POINT('Ctrl Pts',(-17.5259699480092,17.3338006396197,6.27616319744218));
#40429=CARTESIAN_POINT('Ctrl Pts',(-17.1993309492766,17.6148421450605,6.78992974985876));
#40430=CARTESIAN_POINT('Ctrl Pts',(-17.2290682897225,17.6680734413416,6.34216041477718));
#40431=CARTESIAN_POINT('Ctrl Pts',(-17.5240770741103,17.3322137206402,6.27584988377669));
#40432=CARTESIAN_POINT('Ctrl Pts',(-17.1893716918988,17.6062334486389,6.78900404892269));
#40433=CARTESIAN_POINT('Ctrl Pts',(-17.2192636543449,17.6605500551435,6.34067503352136));
#40434=CARTESIAN_POINT('Ctrl Pts',(-17.5203423496229,17.3290032721058,6.27521602822943));
#40435=CARTESIAN_POINT('Ctrl Pts',(-17.1844557566987,17.6018767026284,6.78853506940883));
#40436=CARTESIAN_POINT('Ctrl Pts',(-17.2144128912708,17.6567376554324,6.33992233162338));
#40437=CARTESIAN_POINT('Ctrl Pts',(-17.5184988766973,17.3273785031339,6.27489524164313));
#40438=CARTESIAN_POINT('Ctrl Pts',(-17.169896855944,17.5886510409319,6.78710983089398));
#40439=CARTESIAN_POINT('Ctrl Pts',(-17.2000081285538,17.6451450983018,6.33763355279219));
#40440=CARTESIAN_POINT('Ctrl Pts',(-17.5130392850471,17.3224462500153,6.27392144126411));
#40441=CARTESIAN_POINT('Ctrl Pts',(-17.1604426857215,17.5796268087842,6.78613528430944));
#40442=CARTESIAN_POINT('Ctrl Pts',(-17.1906117770433,17.6372170607117,6.33606827910802));
#40443=CARTESIAN_POINT('Ctrl Pts',(-17.5094939755331,17.3190808343234,6.27325698974518));
#40444=CARTESIAN_POINT('Ctrl Pts',(-17.1144092624932,17.5334875838914,6.78114111890133));
#40445=CARTESIAN_POINT('Ctrl Pts',(-17.1445255959529,17.5964801911601,6.32802538713625));
#40446=CARTESIAN_POINT('Ctrl Pts',(-17.4922314331161,17.3018741366695,6.26985978195909));
#40447=CARTESIAN_POINT('Ctrl Pts',(-17.0815070486393,17.4933474524288,6.77676052830464));
#40448=CARTESIAN_POINT('Ctrl Pts',(-17.1109009441881,17.5607248183131,6.32096601796079));
#40449=CARTESIAN_POINT('Ctrl Pts',(-17.4798931004167,17.2869047271829,6.26690429360894));
#40450=CARTESIAN_POINT('Ctrl Pts',(-17.0453050933139,17.4391198002594,6.77077798629523));
#40451=CARTESIAN_POINT('Ctrl Pts',(-17.0729618602987,17.5119192000139,6.31133007096938));
#40452=CARTESIAN_POINT('Ctrl Pts',(-17.4663173790063,17.2666817095338,6.26291155808251));
#40453=CARTESIAN_POINT('Ctrl Pts',(-17.0383132060228,17.4280698300166,6.76955593094628));
#40454=CARTESIAN_POINT('Ctrl Pts',(-17.065556626733,17.5019159878677,6.30935508478244));
#40455=CARTESIAN_POINT('Ctrl Pts',(-17.4636954152817,17.2625608716606,6.2620979596344));
#40456=CARTESIAN_POINT('Ctrl Pts',(-17.0248360913008,17.4055530530904,6.76705920363801));
#40457=CARTESIAN_POINT('Ctrl Pts',(-17.0511605700457,17.4814635711966,6.30531705781432));
#40458=CARTESIAN_POINT('Ctrl Pts',(-17.4586415045071,17.2541637364834,6.26044006957447));
#40459=CARTESIAN_POINT('Ctrl Pts',(-17.018385745669,17.3941425328792,6.76579076471037));
#40460=CARTESIAN_POINT('Ctrl Pts',(-17.044207273457,17.4710642956499,6.30326387477087));
#40461=CARTESIAN_POINT('Ctrl Pts',(-17.4562226243632,17.2499084384684,6.25959992396146));
#40462=CARTESIAN_POINT('Ctrl Pts',(-16.9999748915757,17.3596229038005,6.76194338591157));
#40463=CARTESIAN_POINT('Ctrl Pts',(-17.0241507155953,17.4394666729185,6.29702539181943));
#40464=CARTESIAN_POINT('Ctrl Pts',(-17.449318544805,17.237035119937,6.25705827774745));
#40465=CARTESIAN_POINT('Ctrl Pts',(-16.9889119861745,17.3361594967524,6.75931504519851));
#40466=CARTESIAN_POINT('Ctrl Pts',(-17.0118468913603,17.4178612762011,6.29275972600569));
#40467=CARTESIAN_POINT('Ctrl Pts',(-17.4451699630122,17.2282849645212,6.25533068906623));
#40468=CARTESIAN_POINT('Ctrl Pts',(-16.969151536231,17.2883531218114,6.75393133468145));
#40469=CARTESIAN_POINT('Ctrl Pts',(-16.9893185039968,17.3735255531602,6.28400629367688));
#40470=CARTESIAN_POINT('Ctrl Pts',(-17.4377597911824,17.2104566385494,6.25181074996914));
#40471=CARTESIAN_POINT('Ctrl Pts',(-16.9604540998271,17.2640101175317,6.75117596780138));
#40472=CARTESIAN_POINT('Ctrl Pts',(-16.979100694343,17.3507885344851,6.27951720585606));
#40473=CARTESIAN_POINT('Ctrl Pts',(-17.4344982506951,17.2013784496697,6.25001839593549));
#40474=CARTESIAN_POINT('Ctrl Pts',(-16.9454368141968,17.2144400485736,6.74553518479638));
#40475=CARTESIAN_POINT('Ctrl Pts',(-16.9607944578447,17.3041453864073,6.27030820660447));
#40476=CARTESIAN_POINT('Ctrl Pts',(-17.4288667753564,17.1828923505283,6.24636858926135));
#40477=CARTESIAN_POINT('Ctrl Pts',(-16.9391152612491,17.1892056047591,6.74264892813991));
#40478=CARTESIAN_POINT('Ctrl Pts',(-16.9527111071462,17.2802251876746,6.26558551739275));
#40479=CARTESIAN_POINT('Ctrl Pts',(-17.4264961901478,17.173481691707,6.24451059395842));
#40480=CARTESIAN_POINT('Ctrl Pts',(-16.9340264307573,17.163528852123,6.73969634090002));
#40481=CARTESIAN_POINT('Ctrl Pts',(-16.9457712867961,17.2557485214382,6.26075296190838));
#40482=CARTESIAN_POINT('Ctrl Pts',(-17.4245878781802,17.16390605946,6.24262002709426));
#40483=CARTESIAN_POINT('Origin',(-37.718924746634,17.5,-2.5));
#40484=CARTESIAN_POINT('Ctrl Pts',(-36.918924746634,26.,0.));
#40485=CARTESIAN_POINT('Ctrl Pts',(-36.7522580799673,26.,5.19615242270663));
#40486=CARTESIAN_POINT('Ctrl Pts',(-36.5855914133007,30.5,7.79422863405995));
#40487=CARTESIAN_POINT('Ctrl Pts',(-36.418924746634,35.,10.3923048454133));
#40488=CARTESIAN_POINT('Ctrl Pts',(-36.2522580799673,39.5,7.79422863405995));
#40489=CARTESIAN_POINT('Ctrl Pts',(-36.0855914133007,44.,5.19615242270663));
#40490=CARTESIAN_POINT('Ctrl Pts',(-35.918924746634,44.,1.10218211923262E-15));
#40491=CARTESIAN_POINT('Ctrl Pts',(-35.7522580799673,44.,-5.19615242270663));
#40492=CARTESIAN_POINT('Ctrl Pts',(-35.5855914133007,39.5,-7.79422863405995));
#40493=CARTESIAN_POINT('Ctrl Pts',(-35.418924746634,35.,-10.3923048454133));
#40494=CARTESIAN_POINT('Ctrl Pts',(-35.2522580799673,30.5,-7.79422863405995));
#40495=CARTESIAN_POINT('Ctrl Pts',(-35.0855914133007,26.,-5.19615242270663));
#40496=CARTESIAN_POINT('Ctrl Pts',(-34.918924746634,26.,0.));
#40497=CARTESIAN_POINT('Ctrl Pts',(-34.7522580799673,26.,5.19615242270663));
#40498=CARTESIAN_POINT('Ctrl Pts',(-34.5855914133007,30.5,7.79422863405995));
#40499=CARTESIAN_POINT('Ctrl Pts',(-34.418924746634,35.,10.3923048454133));
#40500=CARTESIAN_POINT('Ctrl Pts',(-34.2522580799673,39.5,7.79422863405995));
#40501=CARTESIAN_POINT('Ctrl Pts',(-34.0855914133007,44.,5.19615242270663));
#40502=CARTESIAN_POINT('Ctrl Pts',(-33.918924746634,44.,1.10218211923262E-15));
#40503=CARTESIAN_POINT('Ctrl Pts',(-33.7522580799673,44.,-5.19615242270663));
#40504=CARTESIAN_POINT('Ctrl Pts',(-33.5855914133007,39.5,-7.79422863405995));
#40505=CARTESIAN_POINT('Ctrl Pts',(-33.418924746634,35.,-10.3923048454133));
#40506=CARTESIAN_POINT('Ctrl Pts',(-33.2522580799673,30.5,-7.79422863405995));
#40507=CARTESIAN_POINT('Ctrl Pts',(-33.0855914133007,26.,-5.19615242270663));
#40508=CARTESIAN_POINT('Ctrl Pts',(-32.918924746634,26.,0.));
#40509=CARTESIAN_POINT('Ctrl Pts',(-32.7522580799673,26.,5.19615242270663));
#40510=CARTESIAN_POINT('Ctrl Pts',(-32.5855914133007,30.5,7.79422863405995));
#40511=CARTESIAN_POINT('Ctrl Pts',(-32.418924746634,35.,10.3923048454133));
#40512=CARTESIAN_POINT('Ctrl Pts',(-32.2522580799673,39.5,7.79422863405995));
#40513=CARTESIAN_POINT('Ctrl Pts',(-32.0855914133007,44.,5.19615242270663));
#40514=CARTESIAN_POINT('Ctrl Pts',(-31.918924746634,44.,1.10218211923262E-15));
#40515=CARTESIAN_POINT('Ctrl Pts',(-31.7522580799673,44.,-5.19615242270663));
#40516=CARTESIAN_POINT('Ctrl Pts',(-31.5855914133007,39.5,-7.79422863405995));
#40517=CARTESIAN_POINT('Ctrl Pts',(-31.418924746634,35.,-10.3923048454133));
#40518=CARTESIAN_POINT('Ctrl Pts',(-31.2522580799673,30.5,-7.79422863405995));
#40519=CARTESIAN_POINT('Ctrl Pts',(-31.0855914133007,26.,-5.19615242270663));
#40520=CARTESIAN_POINT('Ctrl Pts',(-30.918924746634,26.,0.));
#40521=CARTESIAN_POINT('Ctrl Pts',(-30.7522580799673,26.,5.19615242270663));
#40522=CARTESIAN_POINT('Ctrl Pts',(-30.5855914133007,30.5,7.79422863405995));
#40523=CARTESIAN_POINT('Ctrl Pts',(-30.418924746634,35.,10.3923048454133));
#40524=CARTESIAN_POINT('Ctrl Pts',(-30.2522580799673,39.5,7.79422863405995));
#40525=CARTESIAN_POINT('Ctrl Pts',(-30.0855914133007,44.,5.19615242270663));
#40526=CARTESIAN_POINT('Ctrl Pts',(-29.918924746634,44.,1.10218211923262E-15));
#40527=CARTESIAN_POINT('Ctrl Pts',(-29.7522580799673,44.,-5.19615242270663));
#40528=CARTESIAN_POINT('Ctrl Pts',(-29.5855914133007,39.5,-7.79422863405995));
#40529=CARTESIAN_POINT('Ctrl Pts',(-29.418924746634,35.,-10.3923048454133));
#40530=CARTESIAN_POINT('Ctrl Pts',(-29.2522580799673,30.5,-7.79422863405995));
#40531=CARTESIAN_POINT('Ctrl Pts',(-29.0855914133007,26.,-5.19615242270663));
#40532=CARTESIAN_POINT('Ctrl Pts',(-28.918924746634,26.,0.));
#40533=CARTESIAN_POINT('Ctrl Pts',(-28.7522580799673,26.,5.19615242270663));
#40534=CARTESIAN_POINT('Ctrl Pts',(-28.5855914133007,30.5,7.79422863405995));
#40535=CARTESIAN_POINT('Ctrl Pts',(-28.418924746634,35.,10.3923048454133));
#40536=CARTESIAN_POINT('Ctrl Pts',(-28.2522580799673,39.5,7.79422863405995));
#40537=CARTESIAN_POINT('Ctrl Pts',(-28.0855914133007,44.,5.19615242270663));
#40538=CARTESIAN_POINT('Ctrl Pts',(-27.918924746634,44.,1.10218211923262E-15));
#40539=CARTESIAN_POINT('Ctrl Pts',(-27.7522580799673,44.,-5.19615242270663));
#40540=CARTESIAN_POINT('Ctrl Pts',(-27.5855914133007,39.5,-7.79422863405995));
#40541=CARTESIAN_POINT('Ctrl Pts',(-27.418924746634,35.,-10.3923048454133));
#40542=CARTESIAN_POINT('Ctrl Pts',(-27.2522580799673,30.5,-7.79422863405995));
#40543=CARTESIAN_POINT('Ctrl Pts',(-27.0855914133007,26.,-5.19615242270663));
#40544=CARTESIAN_POINT('Ctrl Pts',(-26.918924746634,26.,0.));
#40545=CARTESIAN_POINT('Ctrl Pts',(-26.7522580799673,26.,5.19615242270663));
#40546=CARTESIAN_POINT('Ctrl Pts',(-26.5855914133007,30.5,7.79422863405995));
#40547=CARTESIAN_POINT('Ctrl Pts',(-26.418924746634,35.,10.3923048454133));
#40548=CARTESIAN_POINT('Ctrl Pts',(-26.2522580799673,39.5,7.79422863405995));
#40549=CARTESIAN_POINT('Ctrl Pts',(-26.0855914133007,44.,5.19615242270663));
#40550=CARTESIAN_POINT('Ctrl Pts',(-25.918924746634,44.,1.10218211923262E-15));
#40551=CARTESIAN_POINT('Ctrl Pts',(-25.7522580799673,44.,-5.19615242270663));
#40552=CARTESIAN_POINT('Ctrl Pts',(-25.5855914133007,39.5,-7.79422863405995));
#40553=CARTESIAN_POINT('Ctrl Pts',(-25.418924746634,35.,-10.3923048454133));
#40554=CARTESIAN_POINT('Ctrl Pts',(-25.2522580799673,30.5,-7.79422863405995));
#40555=CARTESIAN_POINT('Ctrl Pts',(-25.0855914133007,26.,-5.19615242270663));
#40556=CARTESIAN_POINT('Ctrl Pts',(-24.918924746634,26.,0.));
#40557=CARTESIAN_POINT('Ctrl Pts',(-24.7522580799673,26.,5.19615242270663));
#40558=CARTESIAN_POINT('Ctrl Pts',(-24.5855914133007,30.5,7.79422863405995));
#40559=CARTESIAN_POINT('Ctrl Pts',(-24.418924746634,35.,10.3923048454133));
#40560=CARTESIAN_POINT('Ctrl Pts',(-24.2522580799673,39.5,7.79422863405995));
#40561=CARTESIAN_POINT('Ctrl Pts',(-24.0855914133007,44.,5.19615242270663));
#40562=CARTESIAN_POINT('Ctrl Pts',(-23.918924746634,44.,1.10218211923262E-15));
#40563=CARTESIAN_POINT('Ctrl Pts',(-23.7522580799673,44.,-5.19615242270663));
#40564=CARTESIAN_POINT('Ctrl Pts',(-23.5855914133007,39.5,-7.79422863405995));
#40565=CARTESIAN_POINT('Ctrl Pts',(-23.418924746634,35.,-10.3923048454133));
#40566=CARTESIAN_POINT('Ctrl Pts',(-23.2522580799673,30.5,-7.79422863405995));
#40567=CARTESIAN_POINT('Ctrl Pts',(-23.0855914133007,26.,-5.19615242270663));
#40568=CARTESIAN_POINT('Ctrl Pts',(-22.918924746634,26.,0.));
#40569=CARTESIAN_POINT('Ctrl Pts',(-22.7522580799673,26.,5.19615242270663));
#40570=CARTESIAN_POINT('Ctrl Pts',(-22.5855914133007,30.5,7.79422863405995));
#40571=CARTESIAN_POINT('Ctrl Pts',(-22.418924746634,35.,10.3923048454133));
#40572=CARTESIAN_POINT('Ctrl Pts',(-22.2522580799674,39.5,7.79422863405995));
#40573=CARTESIAN_POINT('Ctrl Pts',(-22.0855914133007,44.,5.19615242270663));
#40574=CARTESIAN_POINT('Ctrl Pts',(-21.918924746634,44.,1.10218211923262E-15));
#40575=CARTESIAN_POINT('Ctrl Pts',(-21.7522580799673,44.,-5.19615242270663));
#40576=CARTESIAN_POINT('Ctrl Pts',(-21.5855914133006,39.5,-7.79422863405995));
#40577=CARTESIAN_POINT('Ctrl Pts',(-21.418924746634,35.,-10.3923048454133));
#40578=CARTESIAN_POINT('Ctrl Pts',(-21.2522580799673,30.5,-7.79422863405995));
#40579=CARTESIAN_POINT('Ctrl Pts',(-21.0855914133007,26.,-5.19615242270663));
#40580=CARTESIAN_POINT('Ctrl Pts',(-20.918924746634,26.,0.));
#40581=CARTESIAN_POINT('Ctrl Pts',(-20.7522580799673,26.,5.19615242270663));
#40582=CARTESIAN_POINT('Ctrl Pts',(-20.5855914133006,30.5,7.79422863405995));
#40583=CARTESIAN_POINT('Ctrl Pts',(-20.418924746634,35.,10.3923048454133));
#40584=CARTESIAN_POINT('Ctrl Pts',(-20.2522580799673,39.5,7.79422863405995));
#40585=CARTESIAN_POINT('Ctrl Pts',(-20.0855914133007,44.,5.19615242270663));
#40586=CARTESIAN_POINT('Ctrl Pts',(-19.918924746634,44.,1.10218211923262E-15));
#40587=CARTESIAN_POINT('Ctrl Pts',(-19.7522580799674,44.,-5.19615242270663));
#40588=CARTESIAN_POINT('Ctrl Pts',(-19.5855914133006,39.5,-7.79422863405995));
#40589=CARTESIAN_POINT('Ctrl Pts',(-19.418924746634,35.,-10.3923048454133));
#40590=CARTESIAN_POINT('Ctrl Pts',(-19.2522580799674,30.5,-7.79422863405995));
#40591=CARTESIAN_POINT('Ctrl Pts',(-19.0855914133007,26.,-5.19615242270663));
#40592=CARTESIAN_POINT('Ctrl Pts',(-18.918924746634,26.,0.));
#40593=CARTESIAN_POINT('Ctrl Pts',(-18.7522580799673,26.,5.19615242270663));
#40594=CARTESIAN_POINT('Ctrl Pts',(-18.5855914133006,30.5,7.79422863405995));
#40595=CARTESIAN_POINT('Ctrl Pts',(-18.418924746634,35.,10.3923048454133));
#40596=CARTESIAN_POINT('Ctrl Pts',(-18.2522580799673,39.5,7.79422863405995));
#40597=CARTESIAN_POINT('Ctrl Pts',(-18.0855914133006,44.,5.19615242270663));
#40598=CARTESIAN_POINT('Ctrl Pts',(-17.918924746634,44.,1.10218211923262E-15));
#40599=CARTESIAN_POINT('Ctrl Pts',(-17.7522580799673,44.,-5.19615242270663));
#40600=CARTESIAN_POINT('Ctrl Pts',(-17.5855914133006,39.5,-7.79422863405995));
#40601=CARTESIAN_POINT('Ctrl Pts',(-17.418924746634,35.,-10.3923048454133));
#40602=CARTESIAN_POINT('Ctrl Pts',(-17.2522580799673,30.5,-7.79422863405995));
#40603=CARTESIAN_POINT('Ctrl Pts',(-17.0855914133007,26.,-5.19615242270663));
#40604=CARTESIAN_POINT('Ctrl Pts',(-16.918924746634,26.,0.));
#40605=CARTESIAN_POINT('Ctrl Pts',(-36.918924746634,24.4,0.));
#40606=CARTESIAN_POINT('Ctrl Pts',(-36.7522580799673,24.4,6.11991285341003));
#40607=CARTESIAN_POINT('Ctrl Pts',(-36.5855914133007,29.7,9.17986928011504));
#40608=CARTESIAN_POINT('Ctrl Pts',(-36.418924746634,35.,12.2398257068201));
#40609=CARTESIAN_POINT('Ctrl Pts',(-36.2522580799673,40.3,9.17986928011504));
#40610=CARTESIAN_POINT('Ctrl Pts',(-36.0855914133007,45.6,6.11991285341004));
#40611=CARTESIAN_POINT('Ctrl Pts',(-35.918924746634,45.6,1.29812560709619E-15));
#40612=CARTESIAN_POINT('Ctrl Pts',(-35.7522580799673,45.6,-6.11991285341003));
#40613=CARTESIAN_POINT('Ctrl Pts',(-35.5855914133007,40.3,-9.17986928011504));
#40614=CARTESIAN_POINT('Ctrl Pts',(-35.418924746634,35.,-12.2398257068201));
#40615=CARTESIAN_POINT('Ctrl Pts',(-35.2522580799673,29.7,-9.17986928011506));
#40616=CARTESIAN_POINT('Ctrl Pts',(-35.0855914133007,24.4,-6.11991285341004));
#40617=CARTESIAN_POINT('Ctrl Pts',(-34.918924746634,24.4,0.));
#40618=CARTESIAN_POINT('Ctrl Pts',(-34.7522580799673,24.4,6.11991285341003));
#40619=CARTESIAN_POINT('Ctrl Pts',(-34.5855914133007,29.7,9.17986928011504));
#40620=CARTESIAN_POINT('Ctrl Pts',(-34.418924746634,35.,12.2398257068201));
#40621=CARTESIAN_POINT('Ctrl Pts',(-34.2522580799673,40.3,9.17986928011504));
#40622=CARTESIAN_POINT('Ctrl Pts',(-34.0855914133007,45.6,6.11991285341004));
#40623=CARTESIAN_POINT('Ctrl Pts',(-33.918924746634,45.6,1.29812560709619E-15));
#40624=CARTESIAN_POINT('Ctrl Pts',(-33.7522580799673,45.6,-6.11991285341003));
#40625=CARTESIAN_POINT('Ctrl Pts',(-33.5855914133007,40.3,-9.17986928011504));
#40626=CARTESIAN_POINT('Ctrl Pts',(-33.418924746634,35.,-12.2398257068201));
#40627=CARTESIAN_POINT('Ctrl Pts',(-33.2522580799673,29.7,-9.17986928011506));
#40628=CARTESIAN_POINT('Ctrl Pts',(-33.0855914133007,24.4,-6.11991285341004));
#40629=CARTESIAN_POINT('Ctrl Pts',(-32.918924746634,24.4,0.));
#40630=CARTESIAN_POINT('Ctrl Pts',(-32.7522580799673,24.4,6.11991285341003));
#40631=CARTESIAN_POINT('Ctrl Pts',(-32.5855914133007,29.7,9.17986928011504));
#40632=CARTESIAN_POINT('Ctrl Pts',(-32.418924746634,35.,12.2398257068201));
#40633=CARTESIAN_POINT('Ctrl Pts',(-32.2522580799673,40.3,9.17986928011504));
#40634=CARTESIAN_POINT('Ctrl Pts',(-32.0855914133007,45.6,6.11991285341004));
#40635=CARTESIAN_POINT('Ctrl Pts',(-31.918924746634,45.6,1.29812560709619E-15));
#40636=CARTESIAN_POINT('Ctrl Pts',(-31.7522580799673,45.6,-6.11991285341003));
#40637=CARTESIAN_POINT('Ctrl Pts',(-31.5855914133007,40.3,-9.17986928011504));
#40638=CARTESIAN_POINT('Ctrl Pts',(-31.418924746634,35.,-12.2398257068201));
#40639=CARTESIAN_POINT('Ctrl Pts',(-31.2522580799673,29.7,-9.17986928011506));
#40640=CARTESIAN_POINT('Ctrl Pts',(-31.0855914133007,24.4,-6.11991285341004));
#40641=CARTESIAN_POINT('Ctrl Pts',(-30.918924746634,24.4,0.));
#40642=CARTESIAN_POINT('Ctrl Pts',(-30.7522580799673,24.4,6.11991285341003));
#40643=CARTESIAN_POINT('Ctrl Pts',(-30.5855914133007,29.7,9.17986928011504));
#40644=CARTESIAN_POINT('Ctrl Pts',(-30.418924746634,35.,12.2398257068201));
#40645=CARTESIAN_POINT('Ctrl Pts',(-30.2522580799673,40.3,9.17986928011504));
#40646=CARTESIAN_POINT('Ctrl Pts',(-30.0855914133007,45.6,6.11991285341004));
#40647=CARTESIAN_POINT('Ctrl Pts',(-29.918924746634,45.6,1.29812560709619E-15));
#40648=CARTESIAN_POINT('Ctrl Pts',(-29.7522580799673,45.6,-6.11991285341003));
#40649=CARTESIAN_POINT('Ctrl Pts',(-29.5855914133007,40.3,-9.17986928011504));
#40650=CARTESIAN_POINT('Ctrl Pts',(-29.418924746634,35.,-12.2398257068201));
#40651=CARTESIAN_POINT('Ctrl Pts',(-29.2522580799673,29.7,-9.17986928011506));
#40652=CARTESIAN_POINT('Ctrl Pts',(-29.0855914133007,24.4,-6.11991285341004));
#40653=CARTESIAN_POINT('Ctrl Pts',(-28.918924746634,24.4,0.));
#40654=CARTESIAN_POINT('Ctrl Pts',(-28.7522580799673,24.4,6.11991285341003));
#40655=CARTESIAN_POINT('Ctrl Pts',(-28.5855914133007,29.7,9.17986928011504));
#40656=CARTESIAN_POINT('Ctrl Pts',(-28.418924746634,35.,12.2398257068201));
#40657=CARTESIAN_POINT('Ctrl Pts',(-28.2522580799673,40.3,9.17986928011504));
#40658=CARTESIAN_POINT('Ctrl Pts',(-28.0855914133007,45.6,6.11991285341004));
#40659=CARTESIAN_POINT('Ctrl Pts',(-27.918924746634,45.6,1.29812560709619E-15));
#40660=CARTESIAN_POINT('Ctrl Pts',(-27.7522580799673,45.6,-6.11991285341003));
#40661=CARTESIAN_POINT('Ctrl Pts',(-27.5855914133007,40.3,-9.17986928011504));
#40662=CARTESIAN_POINT('Ctrl Pts',(-27.418924746634,35.,-12.2398257068201));
#40663=CARTESIAN_POINT('Ctrl Pts',(-27.2522580799673,29.7,-9.17986928011506));
#40664=CARTESIAN_POINT('Ctrl Pts',(-27.0855914133007,24.4,-6.11991285341004));
#40665=CARTESIAN_POINT('Ctrl Pts',(-26.918924746634,24.4,0.));
#40666=CARTESIAN_POINT('Ctrl Pts',(-26.7522580799673,24.4,6.11991285341003));
#40667=CARTESIAN_POINT('Ctrl Pts',(-26.5855914133007,29.7,9.17986928011504));
#40668=CARTESIAN_POINT('Ctrl Pts',(-26.418924746634,35.,12.2398257068201));
#40669=CARTESIAN_POINT('Ctrl Pts',(-26.2522580799673,40.3,9.17986928011504));
#40670=CARTESIAN_POINT('Ctrl Pts',(-26.0855914133007,45.6,6.11991285341004));
#40671=CARTESIAN_POINT('Ctrl Pts',(-25.918924746634,45.6,1.29812560709619E-15));
#40672=CARTESIAN_POINT('Ctrl Pts',(-25.7522580799673,45.6,-6.11991285341003));
#40673=CARTESIAN_POINT('Ctrl Pts',(-25.5855914133007,40.3,-9.17986928011504));
#40674=CARTESIAN_POINT('Ctrl Pts',(-25.418924746634,35.,-12.2398257068201));
#40675=CARTESIAN_POINT('Ctrl Pts',(-25.2522580799673,29.7,-9.17986928011506));
#40676=CARTESIAN_POINT('Ctrl Pts',(-25.0855914133007,24.4,-6.11991285341004));
#40677=CARTESIAN_POINT('Ctrl Pts',(-24.918924746634,24.4,0.));
#40678=CARTESIAN_POINT('Ctrl Pts',(-24.7522580799673,24.4,6.11991285341003));
#40679=CARTESIAN_POINT('Ctrl Pts',(-24.5855914133007,29.7,9.17986928011504));
#40680=CARTESIAN_POINT('Ctrl Pts',(-24.418924746634,35.,12.2398257068201));
#40681=CARTESIAN_POINT('Ctrl Pts',(-24.2522580799673,40.3,9.17986928011504));
#40682=CARTESIAN_POINT('Ctrl Pts',(-24.0855914133007,45.6,6.11991285341004));
#40683=CARTESIAN_POINT('Ctrl Pts',(-23.918924746634,45.6,1.29812560709619E-15));
#40684=CARTESIAN_POINT('Ctrl Pts',(-23.7522580799673,45.6,-6.11991285341003));
#40685=CARTESIAN_POINT('Ctrl Pts',(-23.5855914133007,40.3,-9.17986928011504));
#40686=CARTESIAN_POINT('Ctrl Pts',(-23.418924746634,35.,-12.2398257068201));
#40687=CARTESIAN_POINT('Ctrl Pts',(-23.2522580799673,29.7,-9.17986928011506));
#40688=CARTESIAN_POINT('Ctrl Pts',(-23.0855914133007,24.4,-6.11991285341004));
#40689=CARTESIAN_POINT('Ctrl Pts',(-22.918924746634,24.4,0.));
#40690=CARTESIAN_POINT('Ctrl Pts',(-22.7522580799673,24.4,6.11991285341003));
#40691=CARTESIAN_POINT('Ctrl Pts',(-22.5855914133007,29.7,9.17986928011504));
#40692=CARTESIAN_POINT('Ctrl Pts',(-22.418924746634,35.,12.2398257068201));
#40693=CARTESIAN_POINT('Ctrl Pts',(-22.2522580799673,40.3,9.17986928011504));
#40694=CARTESIAN_POINT('Ctrl Pts',(-22.0855914133007,45.6,6.11991285341004));
#40695=CARTESIAN_POINT('Ctrl Pts',(-21.918924746634,45.6,1.29812560709619E-15));
#40696=CARTESIAN_POINT('Ctrl Pts',(-21.7522580799673,45.6,-6.11991285341003));
#40697=CARTESIAN_POINT('Ctrl Pts',(-21.5855914133007,40.3,-9.17986928011504));
#40698=CARTESIAN_POINT('Ctrl Pts',(-21.418924746634,35.,-12.2398257068201));
#40699=CARTESIAN_POINT('Ctrl Pts',(-21.2522580799673,29.7,-9.17986928011506));
#40700=CARTESIAN_POINT('Ctrl Pts',(-21.0855914133007,24.4,-6.11991285341004));
#40701=CARTESIAN_POINT('Ctrl Pts',(-20.918924746634,24.4,0.));
#40702=CARTESIAN_POINT('Ctrl Pts',(-20.7522580799673,24.4,6.11991285341003));
#40703=CARTESIAN_POINT('Ctrl Pts',(-20.5855914133007,29.7,9.17986928011504));
#40704=CARTESIAN_POINT('Ctrl Pts',(-20.418924746634,35.,12.2398257068201));
#40705=CARTESIAN_POINT('Ctrl Pts',(-20.2522580799673,40.3,9.17986928011504));
#40706=CARTESIAN_POINT('Ctrl Pts',(-20.0855914133007,45.6,6.11991285341004));
#40707=CARTESIAN_POINT('Ctrl Pts',(-19.918924746634,45.6,1.29812560709619E-15));
#40708=CARTESIAN_POINT('Ctrl Pts',(-19.7522580799673,45.6,-6.11991285341003));
#40709=CARTESIAN_POINT('Ctrl Pts',(-19.5855914133007,40.3,-9.17986928011504));
#40710=CARTESIAN_POINT('Ctrl Pts',(-19.418924746634,35.,-12.2398257068201));
#40711=CARTESIAN_POINT('Ctrl Pts',(-19.2522580799673,29.7,-9.17986928011506));
#40712=CARTESIAN_POINT('Ctrl Pts',(-19.0855914133006,24.4,-6.11991285341004));
#40713=CARTESIAN_POINT('Ctrl Pts',(-18.918924746634,24.4,0.));
#40714=CARTESIAN_POINT('Ctrl Pts',(-18.7522580799673,24.4,6.11991285341003));
#40715=CARTESIAN_POINT('Ctrl Pts',(-18.5855914133007,29.7,9.17986928011504));
#40716=CARTESIAN_POINT('Ctrl Pts',(-18.418924746634,35.,12.2398257068201));
#40717=CARTESIAN_POINT('Ctrl Pts',(-18.2522580799673,40.3,9.17986928011504));
#40718=CARTESIAN_POINT('Ctrl Pts',(-18.0855914133007,45.6,6.11991285341004));
#40719=CARTESIAN_POINT('Ctrl Pts',(-17.918924746634,45.6,1.29812560709619E-15));
#40720=CARTESIAN_POINT('Ctrl Pts',(-17.7522580799674,45.6,-6.11991285341003));
#40721=CARTESIAN_POINT('Ctrl Pts',(-17.5855914133007,40.3,-9.17986928011504));
#40722=CARTESIAN_POINT('Ctrl Pts',(-17.418924746634,35.,-12.2398257068201));
#40723=CARTESIAN_POINT('Ctrl Pts',(-17.2522580799674,29.7,-9.17986928011506));
#40724=CARTESIAN_POINT('Ctrl Pts',(-17.0855914133007,24.4,-6.11991285341004));
#40725=CARTESIAN_POINT('Ctrl Pts',(-16.918924746634,24.4,0.));
#40726=CARTESIAN_POINT('Ctrl Pts',(-38.518924746634,24.4,0.));
#40727=CARTESIAN_POINT('Ctrl Pts',(-38.3522580799673,24.4,6.11991285341003));
#40728=CARTESIAN_POINT('Ctrl Pts',(-38.1855914133007,29.7,9.17986928011504));
#40729=CARTESIAN_POINT('Ctrl Pts',(-38.018924746634,35.,12.2398257068201));
#40730=CARTESIAN_POINT('Ctrl Pts',(-37.8522580799673,40.3,9.17986928011504));
#40731=CARTESIAN_POINT('Ctrl Pts',(-37.6855914133007,45.6,6.11991285341004));
#40732=CARTESIAN_POINT('Ctrl Pts',(-37.518924746634,45.6,1.29812560709619E-15));
#40733=CARTESIAN_POINT('Ctrl Pts',(-37.3522580799673,45.6,-6.11991285341003));
#40734=CARTESIAN_POINT('Ctrl Pts',(-37.1855914133007,40.3,-9.17986928011504));
#40735=CARTESIAN_POINT('Ctrl Pts',(-37.018924746634,35.,-12.2398257068201));
#40736=CARTESIAN_POINT('Ctrl Pts',(-36.8522580799673,29.7,-9.17986928011506));
#40737=CARTESIAN_POINT('Ctrl Pts',(-36.6855914133007,24.4,-6.11991285341004));
#40738=CARTESIAN_POINT('Ctrl Pts',(-36.518924746634,24.4,0.));
#40739=CARTESIAN_POINT('Ctrl Pts',(-36.3522580799673,24.4,6.11991285341003));
#40740=CARTESIAN_POINT('Ctrl Pts',(-36.1855914133007,29.7,9.17986928011504));
#40741=CARTESIAN_POINT('Ctrl Pts',(-36.018924746634,35.,12.2398257068201));
#40742=CARTESIAN_POINT('Ctrl Pts',(-35.8522580799673,40.3,9.17986928011504));
#40743=CARTESIAN_POINT('Ctrl Pts',(-35.6855914133007,45.6,6.11991285341004));
#40744=CARTESIAN_POINT('Ctrl Pts',(-35.518924746634,45.6,1.29812560709619E-15));
#40745=CARTESIAN_POINT('Ctrl Pts',(-35.3522580799673,45.6,-6.11991285341003));
#40746=CARTESIAN_POINT('Ctrl Pts',(-35.1855914133007,40.3,-9.17986928011504));
#40747=CARTESIAN_POINT('Ctrl Pts',(-35.018924746634,35.,-12.2398257068201));
#40748=CARTESIAN_POINT('Ctrl Pts',(-34.8522580799673,29.7,-9.17986928011506));
#40749=CARTESIAN_POINT('Ctrl Pts',(-34.6855914133007,24.4,-6.11991285341004));
#40750=CARTESIAN_POINT('Ctrl Pts',(-34.518924746634,24.4,0.));
#40751=CARTESIAN_POINT('Ctrl Pts',(-34.3522580799673,24.4,6.11991285341003));
#40752=CARTESIAN_POINT('Ctrl Pts',(-34.1855914133007,29.7,9.17986928011504));
#40753=CARTESIAN_POINT('Ctrl Pts',(-34.018924746634,35.,12.2398257068201));
#40754=CARTESIAN_POINT('Ctrl Pts',(-33.8522580799673,40.3,9.17986928011504));
#40755=CARTESIAN_POINT('Ctrl Pts',(-33.6855914133007,45.6,6.11991285341004));
#40756=CARTESIAN_POINT('Ctrl Pts',(-33.518924746634,45.6,1.29812560709619E-15));
#40757=CARTESIAN_POINT('Ctrl Pts',(-33.3522580799673,45.6,-6.11991285341003));
#40758=CARTESIAN_POINT('Ctrl Pts',(-33.1855914133007,40.3,-9.17986928011504));
#40759=CARTESIAN_POINT('Ctrl Pts',(-33.018924746634,35.,-12.2398257068201));
#40760=CARTESIAN_POINT('Ctrl Pts',(-32.8522580799673,29.7,-9.17986928011506));
#40761=CARTESIAN_POINT('Ctrl Pts',(-32.6855914133007,24.4,-6.11991285341004));
#40762=CARTESIAN_POINT('Ctrl Pts',(-32.518924746634,24.4,0.));
#40763=CARTESIAN_POINT('Ctrl Pts',(-32.3522580799673,24.4,6.11991285341003));
#40764=CARTESIAN_POINT('Ctrl Pts',(-32.1855914133007,29.7,9.17986928011504));
#40765=CARTESIAN_POINT('Ctrl Pts',(-32.018924746634,35.,12.2398257068201));
#40766=CARTESIAN_POINT('Ctrl Pts',(-31.8522580799674,40.3,9.17986928011504));
#40767=CARTESIAN_POINT('Ctrl Pts',(-31.6855914133007,45.6,6.11991285341004));
#40768=CARTESIAN_POINT('Ctrl Pts',(-31.518924746634,45.6,1.29812560709619E-15));
#40769=CARTESIAN_POINT('Ctrl Pts',(-31.3522580799673,45.6,-6.11991285341003));
#40770=CARTESIAN_POINT('Ctrl Pts',(-31.1855914133007,40.3,-9.17986928011504));
#40771=CARTESIAN_POINT('Ctrl Pts',(-31.018924746634,35.,-12.2398257068201));
#40772=CARTESIAN_POINT('Ctrl Pts',(-30.8522580799673,29.7,-9.17986928011506));
#40773=CARTESIAN_POINT('Ctrl Pts',(-30.6855914133007,24.4,-6.11991285341004));
#40774=CARTESIAN_POINT('Ctrl Pts',(-30.518924746634,24.4,0.));
#40775=CARTESIAN_POINT('Ctrl Pts',(-30.3522580799673,24.4,6.11991285341003));
#40776=CARTESIAN_POINT('Ctrl Pts',(-30.1855914133007,29.7,9.17986928011504));
#40777=CARTESIAN_POINT('Ctrl Pts',(-30.018924746634,35.,12.2398257068201));
#40778=CARTESIAN_POINT('Ctrl Pts',(-29.8522580799673,40.3,9.17986928011504));
#40779=CARTESIAN_POINT('Ctrl Pts',(-29.6855914133007,45.6,6.11991285341004));
#40780=CARTESIAN_POINT('Ctrl Pts',(-29.518924746634,45.6,1.29812560709619E-15));
#40781=CARTESIAN_POINT('Ctrl Pts',(-29.3522580799673,45.6,-6.11991285341003));
#40782=CARTESIAN_POINT('Ctrl Pts',(-29.1855914133007,40.3,-9.17986928011504));
#40783=CARTESIAN_POINT('Ctrl Pts',(-29.018924746634,35.,-12.2398257068201));
#40784=CARTESIAN_POINT('Ctrl Pts',(-28.8522580799673,29.7,-9.17986928011506));
#40785=CARTESIAN_POINT('Ctrl Pts',(-28.6855914133007,24.4,-6.11991285341004));
#40786=CARTESIAN_POINT('Ctrl Pts',(-28.518924746634,24.4,0.));
#40787=CARTESIAN_POINT('Ctrl Pts',(-28.3522580799673,24.4,6.11991285341003));
#40788=CARTESIAN_POINT('Ctrl Pts',(-28.1855914133007,29.7,9.17986928011504));
#40789=CARTESIAN_POINT('Ctrl Pts',(-28.018924746634,35.,12.2398257068201));
#40790=CARTESIAN_POINT('Ctrl Pts',(-27.8522580799673,40.3,9.17986928011504));
#40791=CARTESIAN_POINT('Ctrl Pts',(-27.6855914133007,45.6,6.11991285341004));
#40792=CARTESIAN_POINT('Ctrl Pts',(-27.518924746634,45.6,1.29812560709619E-15));
#40793=CARTESIAN_POINT('Ctrl Pts',(-27.3522580799673,45.6,-6.11991285341003));
#40794=CARTESIAN_POINT('Ctrl Pts',(-27.1855914133007,40.3,-9.17986928011504));
#40795=CARTESIAN_POINT('Ctrl Pts',(-27.018924746634,35.,-12.2398257068201));
#40796=CARTESIAN_POINT('Ctrl Pts',(-26.8522580799673,29.7,-9.17986928011506));
#40797=CARTESIAN_POINT('Ctrl Pts',(-26.6855914133007,24.4,-6.11991285341004));
#40798=CARTESIAN_POINT('Ctrl Pts',(-26.518924746634,24.4,0.));
#40799=CARTESIAN_POINT('Ctrl Pts',(-26.3522580799673,24.4,6.11991285341003));
#40800=CARTESIAN_POINT('Ctrl Pts',(-26.1855914133007,29.7,9.17986928011504));
#40801=CARTESIAN_POINT('Ctrl Pts',(-26.018924746634,35.,12.2398257068201));
#40802=CARTESIAN_POINT('Ctrl Pts',(-25.8522580799673,40.3,9.17986928011504));
#40803=CARTESIAN_POINT('Ctrl Pts',(-25.6855914133007,45.6,6.11991285341004));
#40804=CARTESIAN_POINT('Ctrl Pts',(-25.518924746634,45.6,1.29812560709619E-15));
#40805=CARTESIAN_POINT('Ctrl Pts',(-25.3522580799673,45.6,-6.11991285341003));
#40806=CARTESIAN_POINT('Ctrl Pts',(-25.1855914133007,40.3,-9.17986928011504));
#40807=CARTESIAN_POINT('Ctrl Pts',(-25.018924746634,35.,-12.2398257068201));
#40808=CARTESIAN_POINT('Ctrl Pts',(-24.8522580799673,29.7,-9.17986928011506));
#40809=CARTESIAN_POINT('Ctrl Pts',(-24.6855914133007,24.4,-6.11991285341004));
#40810=CARTESIAN_POINT('Ctrl Pts',(-24.518924746634,24.4,0.));
#40811=CARTESIAN_POINT('Ctrl Pts',(-24.3522580799673,24.4,6.11991285341003));
#40812=CARTESIAN_POINT('Ctrl Pts',(-24.1855914133007,29.7,9.17986928011504));
#40813=CARTESIAN_POINT('Ctrl Pts',(-24.018924746634,35.,12.2398257068201));
#40814=CARTESIAN_POINT('Ctrl Pts',(-23.8522580799674,40.3,9.17986928011504));
#40815=CARTESIAN_POINT('Ctrl Pts',(-23.6855914133007,45.6,6.11991285341004));
#40816=CARTESIAN_POINT('Ctrl Pts',(-23.518924746634,45.6,1.29812560709619E-15));
#40817=CARTESIAN_POINT('Ctrl Pts',(-23.3522580799673,45.6,-6.11991285341003));
#40818=CARTESIAN_POINT('Ctrl Pts',(-23.1855914133007,40.3,-9.17986928011504));
#40819=CARTESIAN_POINT('Ctrl Pts',(-23.018924746634,35.,-12.2398257068201));
#40820=CARTESIAN_POINT('Ctrl Pts',(-22.8522580799673,29.7,-9.17986928011506));
#40821=CARTESIAN_POINT('Ctrl Pts',(-22.6855914133007,24.4,-6.11991285341004));
#40822=CARTESIAN_POINT('Ctrl Pts',(-22.518924746634,24.4,0.));
#40823=CARTESIAN_POINT('Ctrl Pts',(-22.3522580799673,24.4,6.11991285341003));
#40824=CARTESIAN_POINT('Ctrl Pts',(-22.1855914133007,29.7,9.17986928011504));
#40825=CARTESIAN_POINT('Ctrl Pts',(-22.018924746634,35.,12.2398257068201));
#40826=CARTESIAN_POINT('Ctrl Pts',(-21.8522580799673,40.3,9.17986928011504));
#40827=CARTESIAN_POINT('Ctrl Pts',(-21.6855914133007,45.6,6.11991285341004));
#40828=CARTESIAN_POINT('Ctrl Pts',(-21.518924746634,45.6,1.29812560709619E-15));
#40829=CARTESIAN_POINT('Ctrl Pts',(-21.3522580799673,45.6,-6.11991285341003));
#40830=CARTESIAN_POINT('Ctrl Pts',(-21.1855914133007,40.3,-9.17986928011504));
#40831=CARTESIAN_POINT('Ctrl Pts',(-21.018924746634,35.,-12.2398257068201));
#40832=CARTESIAN_POINT('Ctrl Pts',(-20.8522580799674,29.7,-9.17986928011506));
#40833=CARTESIAN_POINT('Ctrl Pts',(-20.6855914133006,24.4,-6.11991285341004));
#40834=CARTESIAN_POINT('Ctrl Pts',(-20.518924746634,24.4,0.));
#40835=CARTESIAN_POINT('Ctrl Pts',(-20.3522580799673,24.4,6.11991285341003));
#40836=CARTESIAN_POINT('Ctrl Pts',(-20.1855914133007,29.7,9.17986928011504));
#40837=CARTESIAN_POINT('Ctrl Pts',(-20.018924746634,35.,12.2398257068201));
#40838=CARTESIAN_POINT('Ctrl Pts',(-19.8522580799673,40.3,9.17986928011504));
#40839=CARTESIAN_POINT('Ctrl Pts',(-19.6855914133007,45.6,6.11991285341004));
#40840=CARTESIAN_POINT('Ctrl Pts',(-19.518924746634,45.6,1.29812560709619E-15));
#40841=CARTESIAN_POINT('Ctrl Pts',(-19.3522580799673,45.6,-6.11991285341003));
#40842=CARTESIAN_POINT('Ctrl Pts',(-19.1855914133007,40.3,-9.17986928011504));
#40843=CARTESIAN_POINT('Ctrl Pts',(-19.018924746634,35.,-12.2398257068201));
#40844=CARTESIAN_POINT('Ctrl Pts',(-18.8522580799673,29.7,-9.17986928011506));
#40845=CARTESIAN_POINT('Ctrl Pts',(-18.6855914133007,24.4,-6.11991285341004));
#40846=CARTESIAN_POINT('Ctrl Pts',(-18.518924746634,24.4,0.));
#40847=CARTESIAN_POINT('Ctrl Pts',(-38.518924746634,26.,0.));
#40848=CARTESIAN_POINT('Ctrl Pts',(-38.3522580799673,26.,5.19615242270663));
#40849=CARTESIAN_POINT('Ctrl Pts',(-38.1855914133007,30.5,7.79422863405995));
#40850=CARTESIAN_POINT('Ctrl Pts',(-38.018924746634,35.,10.3923048454133));
#40851=CARTESIAN_POINT('Ctrl Pts',(-37.8522580799673,39.5,7.79422863405995));
#40852=CARTESIAN_POINT('Ctrl Pts',(-37.6855914133007,44.,5.19615242270663));
#40853=CARTESIAN_POINT('Ctrl Pts',(-37.518924746634,44.,1.10218211923262E-15));
#40854=CARTESIAN_POINT('Ctrl Pts',(-37.3522580799673,44.,-5.19615242270663));
#40855=CARTESIAN_POINT('Ctrl Pts',(-37.1855914133007,39.5,-7.79422863405995));
#40856=CARTESIAN_POINT('Ctrl Pts',(-37.018924746634,35.,-10.3923048454133));
#40857=CARTESIAN_POINT('Ctrl Pts',(-36.8522580799673,30.5,-7.79422863405995));
#40858=CARTESIAN_POINT('Ctrl Pts',(-36.6855914133007,26.,-5.19615242270663));
#40859=CARTESIAN_POINT('Ctrl Pts',(-36.518924746634,26.,0.));
#40860=CARTESIAN_POINT('Ctrl Pts',(-36.3522580799673,26.,5.19615242270663));
#40861=CARTESIAN_POINT('Ctrl Pts',(-36.1855914133007,30.5,7.79422863405995));
#40862=CARTESIAN_POINT('Ctrl Pts',(-36.018924746634,35.,10.3923048454133));
#40863=CARTESIAN_POINT('Ctrl Pts',(-35.8522580799673,39.5,7.79422863405995));
#40864=CARTESIAN_POINT('Ctrl Pts',(-35.6855914133007,44.,5.19615242270663));
#40865=CARTESIAN_POINT('Ctrl Pts',(-35.518924746634,44.,1.10218211923262E-15));
#40866=CARTESIAN_POINT('Ctrl Pts',(-35.3522580799673,44.,-5.19615242270663));
#40867=CARTESIAN_POINT('Ctrl Pts',(-35.1855914133007,39.5,-7.79422863405995));
#40868=CARTESIAN_POINT('Ctrl Pts',(-35.018924746634,35.,-10.3923048454133));
#40869=CARTESIAN_POINT('Ctrl Pts',(-34.8522580799673,30.5,-7.79422863405995));
#40870=CARTESIAN_POINT('Ctrl Pts',(-34.6855914133007,26.,-5.19615242270663));
#40871=CARTESIAN_POINT('Ctrl Pts',(-34.518924746634,26.,0.));
#40872=CARTESIAN_POINT('Ctrl Pts',(-34.3522580799673,26.,5.19615242270663));
#40873=CARTESIAN_POINT('Ctrl Pts',(-34.1855914133007,30.5,7.79422863405995));
#40874=CARTESIAN_POINT('Ctrl Pts',(-34.018924746634,35.,10.3923048454133));
#40875=CARTESIAN_POINT('Ctrl Pts',(-33.8522580799673,39.5,7.79422863405995));
#40876=CARTESIAN_POINT('Ctrl Pts',(-33.6855914133007,44.,5.19615242270663));
#40877=CARTESIAN_POINT('Ctrl Pts',(-33.518924746634,44.,1.10218211923262E-15));
#40878=CARTESIAN_POINT('Ctrl Pts',(-33.3522580799673,44.,-5.19615242270663));
#40879=CARTESIAN_POINT('Ctrl Pts',(-33.1855914133007,39.5,-7.79422863405995));
#40880=CARTESIAN_POINT('Ctrl Pts',(-33.018924746634,35.,-10.3923048454133));
#40881=CARTESIAN_POINT('Ctrl Pts',(-32.8522580799673,30.5,-7.79422863405995));
#40882=CARTESIAN_POINT('Ctrl Pts',(-32.6855914133007,26.,-5.19615242270663));
#40883=CARTESIAN_POINT('Ctrl Pts',(-32.518924746634,26.,0.));
#40884=CARTESIAN_POINT('Ctrl Pts',(-32.3522580799673,26.,5.19615242270663));
#40885=CARTESIAN_POINT('Ctrl Pts',(-32.1855914133007,30.5,7.79422863405995));
#40886=CARTESIAN_POINT('Ctrl Pts',(-32.018924746634,35.,10.3923048454133));
#40887=CARTESIAN_POINT('Ctrl Pts',(-31.8522580799673,39.5,7.79422863405995));
#40888=CARTESIAN_POINT('Ctrl Pts',(-31.6855914133007,44.,5.19615242270663));
#40889=CARTESIAN_POINT('Ctrl Pts',(-31.518924746634,44.,1.10218211923262E-15));
#40890=CARTESIAN_POINT('Ctrl Pts',(-31.3522580799673,44.,-5.19615242270663));
#40891=CARTESIAN_POINT('Ctrl Pts',(-31.1855914133007,39.5,-7.79422863405995));
#40892=CARTESIAN_POINT('Ctrl Pts',(-31.018924746634,35.,-10.3923048454133));
#40893=CARTESIAN_POINT('Ctrl Pts',(-30.8522580799673,30.5,-7.79422863405995));
#40894=CARTESIAN_POINT('Ctrl Pts',(-30.6855914133007,26.,-5.19615242270663));
#40895=CARTESIAN_POINT('Ctrl Pts',(-30.518924746634,26.,0.));
#40896=CARTESIAN_POINT('Ctrl Pts',(-30.3522580799673,26.,5.19615242270663));
#40897=CARTESIAN_POINT('Ctrl Pts',(-30.1855914133007,30.5,7.79422863405995));
#40898=CARTESIAN_POINT('Ctrl Pts',(-30.018924746634,35.,10.3923048454133));
#40899=CARTESIAN_POINT('Ctrl Pts',(-29.8522580799673,39.5,7.79422863405995));
#40900=CARTESIAN_POINT('Ctrl Pts',(-29.6855914133007,44.,5.19615242270663));
#40901=CARTESIAN_POINT('Ctrl Pts',(-29.518924746634,44.,1.10218211923262E-15));
#40902=CARTESIAN_POINT('Ctrl Pts',(-29.3522580799673,44.,-5.19615242270663));
#40903=CARTESIAN_POINT('Ctrl Pts',(-29.1855914133007,39.5,-7.79422863405995));
#40904=CARTESIAN_POINT('Ctrl Pts',(-29.018924746634,35.,-10.3923048454133));
#40905=CARTESIAN_POINT('Ctrl Pts',(-28.8522580799673,30.5,-7.79422863405995));
#40906=CARTESIAN_POINT('Ctrl Pts',(-28.6855914133007,26.,-5.19615242270663));
#40907=CARTESIAN_POINT('Ctrl Pts',(-28.518924746634,26.,0.));
#40908=CARTESIAN_POINT('Ctrl Pts',(-28.3522580799673,26.,5.19615242270663));
#40909=CARTESIAN_POINT('Ctrl Pts',(-28.1855914133007,30.5,7.79422863405995));
#40910=CARTESIAN_POINT('Ctrl Pts',(-28.018924746634,35.,10.3923048454133));
#40911=CARTESIAN_POINT('Ctrl Pts',(-27.8522580799673,39.5,7.79422863405995));
#40912=CARTESIAN_POINT('Ctrl Pts',(-27.6855914133007,44.,5.19615242270663));
#40913=CARTESIAN_POINT('Ctrl Pts',(-27.518924746634,44.,1.10218211923262E-15));
#40914=CARTESIAN_POINT('Ctrl Pts',(-27.3522580799673,44.,-5.19615242270663));
#40915=CARTESIAN_POINT('Ctrl Pts',(-27.1855914133007,39.5,-7.79422863405995));
#40916=CARTESIAN_POINT('Ctrl Pts',(-27.018924746634,35.,-10.3923048454133));
#40917=CARTESIAN_POINT('Ctrl Pts',(-26.8522580799673,30.5,-7.79422863405995));
#40918=CARTESIAN_POINT('Ctrl Pts',(-26.6855914133007,26.,-5.19615242270663));
#40919=CARTESIAN_POINT('Ctrl Pts',(-26.518924746634,26.,0.));
#40920=CARTESIAN_POINT('Ctrl Pts',(-26.3522580799673,26.,5.19615242270663));
#40921=CARTESIAN_POINT('Ctrl Pts',(-26.1855914133007,30.5,7.79422863405995));
#40922=CARTESIAN_POINT('Ctrl Pts',(-26.018924746634,35.,10.3923048454133));
#40923=CARTESIAN_POINT('Ctrl Pts',(-25.8522580799673,39.5,7.79422863405995));
#40924=CARTESIAN_POINT('Ctrl Pts',(-25.6855914133007,44.,5.19615242270663));
#40925=CARTESIAN_POINT('Ctrl Pts',(-25.518924746634,44.,1.10218211923262E-15));
#40926=CARTESIAN_POINT('Ctrl Pts',(-25.3522580799673,44.,-5.19615242270663));
#40927=CARTESIAN_POINT('Ctrl Pts',(-25.1855914133007,39.5,-7.79422863405995));
#40928=CARTESIAN_POINT('Ctrl Pts',(-25.018924746634,35.,-10.3923048454133));
#40929=CARTESIAN_POINT('Ctrl Pts',(-24.8522580799673,30.5,-7.79422863405995));
#40930=CARTESIAN_POINT('Ctrl Pts',(-24.6855914133007,26.,-5.19615242270663));
#40931=CARTESIAN_POINT('Ctrl Pts',(-24.518924746634,26.,0.));
#40932=CARTESIAN_POINT('Ctrl Pts',(-24.3522580799673,26.,5.19615242270663));
#40933=CARTESIAN_POINT('Ctrl Pts',(-24.1855914133007,30.5,7.79422863405995));
#40934=CARTESIAN_POINT('Ctrl Pts',(-24.018924746634,35.,10.3923048454133));
#40935=CARTESIAN_POINT('Ctrl Pts',(-23.8522580799673,39.5,7.79422863405995));
#40936=CARTESIAN_POINT('Ctrl Pts',(-23.6855914133007,44.,5.19615242270663));
#40937=CARTESIAN_POINT('Ctrl Pts',(-23.518924746634,44.,1.10218211923262E-15));
#40938=CARTESIAN_POINT('Ctrl Pts',(-23.3522580799673,44.,-5.19615242270663));
#40939=CARTESIAN_POINT('Ctrl Pts',(-23.1855914133007,39.5,-7.79422863405995));
#40940=CARTESIAN_POINT('Ctrl Pts',(-23.018924746634,35.,-10.3923048454133));
#40941=CARTESIAN_POINT('Ctrl Pts',(-22.8522580799673,30.5,-7.79422863405995));
#40942=CARTESIAN_POINT('Ctrl Pts',(-22.6855914133007,26.,-5.19615242270663));
#40943=CARTESIAN_POINT('Ctrl Pts',(-22.518924746634,26.,0.));
#40944=CARTESIAN_POINT('Ctrl Pts',(-22.3522580799673,26.,5.19615242270663));
#40945=CARTESIAN_POINT('Ctrl Pts',(-22.1855914133007,30.5,7.79422863405995));
#40946=CARTESIAN_POINT('Ctrl Pts',(-22.018924746634,35.,10.3923048454133));
#40947=CARTESIAN_POINT('Ctrl Pts',(-21.8522580799673,39.5,7.79422863405995));
#40948=CARTESIAN_POINT('Ctrl Pts',(-21.6855914133007,44.,5.19615242270663));
#40949=CARTESIAN_POINT('Ctrl Pts',(-21.518924746634,44.,1.10218211923262E-15));
#40950=CARTESIAN_POINT('Ctrl Pts',(-21.3522580799673,44.,-5.19615242270663));
#40951=CARTESIAN_POINT('Ctrl Pts',(-21.1855914133006,39.5,-7.79422863405995));
#40952=CARTESIAN_POINT('Ctrl Pts',(-21.018924746634,35.,-10.3923048454133));
#40953=CARTESIAN_POINT('Ctrl Pts',(-20.8522580799673,30.5,-7.79422863405995));
#40954=CARTESIAN_POINT('Ctrl Pts',(-20.6855914133007,26.,-5.19615242270663));
#40955=CARTESIAN_POINT('Ctrl Pts',(-20.518924746634,26.,0.));
#40956=CARTESIAN_POINT('Ctrl Pts',(-20.3522580799673,26.,5.19615242270663));
#40957=CARTESIAN_POINT('Ctrl Pts',(-20.1855914133006,30.5,7.79422863405995));
#40958=CARTESIAN_POINT('Ctrl Pts',(-20.018924746634,35.,10.3923048454133));
#40959=CARTESIAN_POINT('Ctrl Pts',(-19.8522580799674,39.5,7.79422863405995));
#40960=CARTESIAN_POINT('Ctrl Pts',(-19.6855914133006,44.,5.19615242270663));
#40961=CARTESIAN_POINT('Ctrl Pts',(-19.518924746634,44.,1.10218211923262E-15));
#40962=CARTESIAN_POINT('Ctrl Pts',(-19.3522580799673,44.,-5.19615242270663));
#40963=CARTESIAN_POINT('Ctrl Pts',(-19.1855914133007,39.5,-7.79422863405995));
#40964=CARTESIAN_POINT('Ctrl Pts',(-19.018924746634,35.,-10.3923048454133));
#40965=CARTESIAN_POINT('Ctrl Pts',(-18.8522580799674,30.5,-7.79422863405995));
#40966=CARTESIAN_POINT('Ctrl Pts',(-18.6855914133007,26.,-5.19615242270663));
#40967=CARTESIAN_POINT('Ctrl Pts',(-18.518924746634,26.,0.));
#40968=CARTESIAN_POINT('Ctrl Pts',(-38.518924746634,27.6,0.));
#40969=CARTESIAN_POINT('Ctrl Pts',(-38.3522580799673,27.6,4.27239199200323));
#40970=CARTESIAN_POINT('Ctrl Pts',(-38.1855914133007,31.3,6.40858798800485));
#40971=CARTESIAN_POINT('Ctrl Pts',(-38.018924746634,35.,8.54478398400645));
#40972=CARTESIAN_POINT('Ctrl Pts',(-37.8522580799673,38.7,6.40858798800485));
#40973=CARTESIAN_POINT('Ctrl Pts',(-37.6855914133007,42.4,4.27239199200323));
#40974=CARTESIAN_POINT('Ctrl Pts',(-37.518924746634,42.4,9.06238631369041E-16));
#40975=CARTESIAN_POINT('Ctrl Pts',(-37.3522580799673,42.4,-4.27239199200323));
#40976=CARTESIAN_POINT('Ctrl Pts',(-37.1855914133007,38.7,-6.40858798800485));
#40977=CARTESIAN_POINT('Ctrl Pts',(-37.018924746634,35.,-8.54478398400645));
#40978=CARTESIAN_POINT('Ctrl Pts',(-36.8522580799673,31.3,-6.40858798800485));
#40979=CARTESIAN_POINT('Ctrl Pts',(-36.6855914133007,27.6,-4.27239199200323));
#40980=CARTESIAN_POINT('Ctrl Pts',(-36.518924746634,27.6,0.));
#40981=CARTESIAN_POINT('Ctrl Pts',(-36.3522580799673,27.6,4.27239199200323));
#40982=CARTESIAN_POINT('Ctrl Pts',(-36.1855914133007,31.3,6.40858798800485));
#40983=CARTESIAN_POINT('Ctrl Pts',(-36.018924746634,35.,8.54478398400645));
#40984=CARTESIAN_POINT('Ctrl Pts',(-35.8522580799673,38.7,6.40858798800485));
#40985=CARTESIAN_POINT('Ctrl Pts',(-35.6855914133007,42.4,4.27239199200323));
#40986=CARTESIAN_POINT('Ctrl Pts',(-35.518924746634,42.4,9.06238631369041E-16));
#40987=CARTESIAN_POINT('Ctrl Pts',(-35.3522580799673,42.4,-4.27239199200323));
#40988=CARTESIAN_POINT('Ctrl Pts',(-35.1855914133007,38.7,-6.40858798800485));
#40989=CARTESIAN_POINT('Ctrl Pts',(-35.018924746634,35.,-8.54478398400645));
#40990=CARTESIAN_POINT('Ctrl Pts',(-34.8522580799673,31.3,-6.40858798800485));
#40991=CARTESIAN_POINT('Ctrl Pts',(-34.6855914133007,27.6,-4.27239199200323));
#40992=CARTESIAN_POINT('Ctrl Pts',(-34.518924746634,27.6,0.));
#40993=CARTESIAN_POINT('Ctrl Pts',(-34.3522580799673,27.6,4.27239199200323));
#40994=CARTESIAN_POINT('Ctrl Pts',(-34.1855914133007,31.3,6.40858798800485));
#40995=CARTESIAN_POINT('Ctrl Pts',(-34.018924746634,35.,8.54478398400645));
#40996=CARTESIAN_POINT('Ctrl Pts',(-33.8522580799673,38.7,6.40858798800485));
#40997=CARTESIAN_POINT('Ctrl Pts',(-33.6855914133007,42.4,4.27239199200323));
#40998=CARTESIAN_POINT('Ctrl Pts',(-33.518924746634,42.4,9.06238631369041E-16));
#40999=CARTESIAN_POINT('Ctrl Pts',(-33.3522580799673,42.4,-4.27239199200323));
#41000=CARTESIAN_POINT('Ctrl Pts',(-33.1855914133007,38.7,-6.40858798800485));
#41001=CARTESIAN_POINT('Ctrl Pts',(-33.018924746634,35.,-8.54478398400645));
#41002=CARTESIAN_POINT('Ctrl Pts',(-32.8522580799673,31.3,-6.40858798800485));
#41003=CARTESIAN_POINT('Ctrl Pts',(-32.6855914133007,27.6,-4.27239199200323));
#41004=CARTESIAN_POINT('Ctrl Pts',(-32.518924746634,27.6,0.));
#41005=CARTESIAN_POINT('Ctrl Pts',(-32.3522580799673,27.6,4.27239199200323));
#41006=CARTESIAN_POINT('Ctrl Pts',(-32.1855914133007,31.3,6.40858798800485));
#41007=CARTESIAN_POINT('Ctrl Pts',(-32.018924746634,35.,8.54478398400645));
#41008=CARTESIAN_POINT('Ctrl Pts',(-31.8522580799674,38.7,6.40858798800485));
#41009=CARTESIAN_POINT('Ctrl Pts',(-31.6855914133007,42.4,4.27239199200323));
#41010=CARTESIAN_POINT('Ctrl Pts',(-31.518924746634,42.4,9.06238631369041E-16));
#41011=CARTESIAN_POINT('Ctrl Pts',(-31.3522580799673,42.4,-4.27239199200323));
#41012=CARTESIAN_POINT('Ctrl Pts',(-31.1855914133007,38.7,-6.40858798800485));
#41013=CARTESIAN_POINT('Ctrl Pts',(-31.018924746634,35.,-8.54478398400645));
#41014=CARTESIAN_POINT('Ctrl Pts',(-30.8522580799673,31.3,-6.40858798800485));
#41015=CARTESIAN_POINT('Ctrl Pts',(-30.6855914133007,27.6,-4.27239199200323));
#41016=CARTESIAN_POINT('Ctrl Pts',(-30.518924746634,27.6,0.));
#41017=CARTESIAN_POINT('Ctrl Pts',(-30.3522580799673,27.6,4.27239199200323));
#41018=CARTESIAN_POINT('Ctrl Pts',(-30.1855914133007,31.3,6.40858798800485));
#41019=CARTESIAN_POINT('Ctrl Pts',(-30.018924746634,35.,8.54478398400645));
#41020=CARTESIAN_POINT('Ctrl Pts',(-29.8522580799673,38.7,6.40858798800485));
#41021=CARTESIAN_POINT('Ctrl Pts',(-29.6855914133007,42.4,4.27239199200323));
#41022=CARTESIAN_POINT('Ctrl Pts',(-29.518924746634,42.4,9.06238631369041E-16));
#41023=CARTESIAN_POINT('Ctrl Pts',(-29.3522580799673,42.4,-4.27239199200323));
#41024=CARTESIAN_POINT('Ctrl Pts',(-29.1855914133007,38.7,-6.40858798800485));
#41025=CARTESIAN_POINT('Ctrl Pts',(-29.018924746634,35.,-8.54478398400645));
#41026=CARTESIAN_POINT('Ctrl Pts',(-28.8522580799673,31.3,-6.40858798800485));
#41027=CARTESIAN_POINT('Ctrl Pts',(-28.6855914133007,27.6,-4.27239199200323));
#41028=CARTESIAN_POINT('Ctrl Pts',(-28.518924746634,27.6,0.));
#41029=CARTESIAN_POINT('Ctrl Pts',(-28.3522580799673,27.6,4.27239199200323));
#41030=CARTESIAN_POINT('Ctrl Pts',(-28.1855914133007,31.3,6.40858798800485));
#41031=CARTESIAN_POINT('Ctrl Pts',(-28.018924746634,35.,8.54478398400645));
#41032=CARTESIAN_POINT('Ctrl Pts',(-27.8522580799673,38.7,6.40858798800485));
#41033=CARTESIAN_POINT('Ctrl Pts',(-27.6855914133007,42.4,4.27239199200323));
#41034=CARTESIAN_POINT('Ctrl Pts',(-27.518924746634,42.4,9.06238631369041E-16));
#41035=CARTESIAN_POINT('Ctrl Pts',(-27.3522580799673,42.4,-4.27239199200323));
#41036=CARTESIAN_POINT('Ctrl Pts',(-27.1855914133007,38.7,-6.40858798800485));
#41037=CARTESIAN_POINT('Ctrl Pts',(-27.018924746634,35.,-8.54478398400645));
#41038=CARTESIAN_POINT('Ctrl Pts',(-26.8522580799673,31.3,-6.40858798800485));
#41039=CARTESIAN_POINT('Ctrl Pts',(-26.6855914133007,27.6,-4.27239199200323));
#41040=CARTESIAN_POINT('Ctrl Pts',(-26.518924746634,27.6,0.));
#41041=CARTESIAN_POINT('Ctrl Pts',(-26.3522580799673,27.6,4.27239199200323));
#41042=CARTESIAN_POINT('Ctrl Pts',(-26.1855914133007,31.3,6.40858798800485));
#41043=CARTESIAN_POINT('Ctrl Pts',(-26.018924746634,35.,8.54478398400645));
#41044=CARTESIAN_POINT('Ctrl Pts',(-25.8522580799673,38.7,6.40858798800485));
#41045=CARTESIAN_POINT('Ctrl Pts',(-25.6855914133007,42.4,4.27239199200323));
#41046=CARTESIAN_POINT('Ctrl Pts',(-25.518924746634,42.4,9.06238631369041E-16));
#41047=CARTESIAN_POINT('Ctrl Pts',(-25.3522580799673,42.4,-4.27239199200323));
#41048=CARTESIAN_POINT('Ctrl Pts',(-25.1855914133007,38.7,-6.40858798800485));
#41049=CARTESIAN_POINT('Ctrl Pts',(-25.018924746634,35.,-8.54478398400645));
#41050=CARTESIAN_POINT('Ctrl Pts',(-24.8522580799673,31.3,-6.40858798800485));
#41051=CARTESIAN_POINT('Ctrl Pts',(-24.6855914133007,27.6,-4.27239199200323));
#41052=CARTESIAN_POINT('Ctrl Pts',(-24.518924746634,27.6,0.));
#41053=CARTESIAN_POINT('Ctrl Pts',(-24.3522580799673,27.6,4.27239199200323));
#41054=CARTESIAN_POINT('Ctrl Pts',(-24.1855914133007,31.3,6.40858798800485));
#41055=CARTESIAN_POINT('Ctrl Pts',(-24.018924746634,35.,8.54478398400645));
#41056=CARTESIAN_POINT('Ctrl Pts',(-23.8522580799674,38.7,6.40858798800485));
#41057=CARTESIAN_POINT('Ctrl Pts',(-23.6855914133007,42.4,4.27239199200323));
#41058=CARTESIAN_POINT('Ctrl Pts',(-23.518924746634,42.4,9.06238631369041E-16));
#41059=CARTESIAN_POINT('Ctrl Pts',(-23.3522580799673,42.4,-4.27239199200323));
#41060=CARTESIAN_POINT('Ctrl Pts',(-23.1855914133007,38.7,-6.40858798800485));
#41061=CARTESIAN_POINT('Ctrl Pts',(-23.018924746634,35.,-8.54478398400645));
#41062=CARTESIAN_POINT('Ctrl Pts',(-22.8522580799673,31.3,-6.40858798800485));
#41063=CARTESIAN_POINT('Ctrl Pts',(-22.6855914133007,27.6,-4.27239199200323));
#41064=CARTESIAN_POINT('Ctrl Pts',(-22.518924746634,27.6,0.));
#41065=CARTESIAN_POINT('Ctrl Pts',(-22.3522580799673,27.6,4.27239199200323));
#41066=CARTESIAN_POINT('Ctrl Pts',(-22.1855914133007,31.3,6.40858798800485));
#41067=CARTESIAN_POINT('Ctrl Pts',(-22.018924746634,35.,8.54478398400645));
#41068=CARTESIAN_POINT('Ctrl Pts',(-21.8522580799673,38.7,6.40858798800485));
#41069=CARTESIAN_POINT('Ctrl Pts',(-21.6855914133007,42.4,4.27239199200323));
#41070=CARTESIAN_POINT('Ctrl Pts',(-21.518924746634,42.4,9.06238631369041E-16));
#41071=CARTESIAN_POINT('Ctrl Pts',(-21.3522580799673,42.4,-4.27239199200323));
#41072=CARTESIAN_POINT('Ctrl Pts',(-21.1855914133007,38.7,-6.40858798800485));
#41073=CARTESIAN_POINT('Ctrl Pts',(-21.018924746634,35.,-8.54478398400645));
#41074=CARTESIAN_POINT('Ctrl Pts',(-20.8522580799674,31.3,-6.40858798800485));
#41075=CARTESIAN_POINT('Ctrl Pts',(-20.6855914133006,27.6,-4.27239199200323));
#41076=CARTESIAN_POINT('Ctrl Pts',(-20.518924746634,27.6,0.));
#41077=CARTESIAN_POINT('Ctrl Pts',(-20.3522580799673,27.6,4.27239199200323));
#41078=CARTESIAN_POINT('Ctrl Pts',(-20.1855914133007,31.3,6.40858798800485));
#41079=CARTESIAN_POINT('Ctrl Pts',(-20.018924746634,35.,8.54478398400645));
#41080=CARTESIAN_POINT('Ctrl Pts',(-19.8522580799673,38.7,6.40858798800485));
#41081=CARTESIAN_POINT('Ctrl Pts',(-19.6855914133007,42.4,4.27239199200323));
#41082=CARTESIAN_POINT('Ctrl Pts',(-19.518924746634,42.4,9.06238631369041E-16));
#41083=CARTESIAN_POINT('Ctrl Pts',(-19.3522580799673,42.4,-4.27239199200323));
#41084=CARTESIAN_POINT('Ctrl Pts',(-19.1855914133007,38.7,-6.40858798800485));
#41085=CARTESIAN_POINT('Ctrl Pts',(-19.018924746634,35.,-8.54478398400645));
#41086=CARTESIAN_POINT('Ctrl Pts',(-18.8522580799673,31.3,-6.40858798800485));
#41087=CARTESIAN_POINT('Ctrl Pts',(-18.6855914133007,27.6,-4.27239199200323));
#41088=CARTESIAN_POINT('Ctrl Pts',(-18.518924746634,27.6,0.));
#41089=CARTESIAN_POINT('Ctrl Pts',(-36.918924746634,27.6,0.));
#41090=CARTESIAN_POINT('Ctrl Pts',(-36.7522580799673,27.6,4.27239199200323));
#41091=CARTESIAN_POINT('Ctrl Pts',(-36.5855914133007,31.3,6.40858798800485));
#41092=CARTESIAN_POINT('Ctrl Pts',(-36.418924746634,35.,8.54478398400645));
#41093=CARTESIAN_POINT('Ctrl Pts',(-36.2522580799673,38.7,6.40858798800485));
#41094=CARTESIAN_POINT('Ctrl Pts',(-36.0855914133007,42.4,4.27239199200323));
#41095=CARTESIAN_POINT('Ctrl Pts',(-35.918924746634,42.4,9.06238631369041E-16));
#41096=CARTESIAN_POINT('Ctrl Pts',(-35.7522580799673,42.4,-4.27239199200323));
#41097=CARTESIAN_POINT('Ctrl Pts',(-35.5855914133007,38.7,-6.40858798800485));
#41098=CARTESIAN_POINT('Ctrl Pts',(-35.418924746634,35.,-8.54478398400645));
#41099=CARTESIAN_POINT('Ctrl Pts',(-35.2522580799673,31.3,-6.40858798800485));
#41100=CARTESIAN_POINT('Ctrl Pts',(-35.0855914133007,27.6,-4.27239199200323));
#41101=CARTESIAN_POINT('Ctrl Pts',(-34.918924746634,27.6,0.));
#41102=CARTESIAN_POINT('Ctrl Pts',(-34.7522580799673,27.6,4.27239199200323));
#41103=CARTESIAN_POINT('Ctrl Pts',(-34.5855914133007,31.3,6.40858798800485));
#41104=CARTESIAN_POINT('Ctrl Pts',(-34.418924746634,35.,8.54478398400645));
#41105=CARTESIAN_POINT('Ctrl Pts',(-34.2522580799673,38.7,6.40858798800485));
#41106=CARTESIAN_POINT('Ctrl Pts',(-34.0855914133007,42.4,4.27239199200323));
#41107=CARTESIAN_POINT('Ctrl Pts',(-33.918924746634,42.4,9.06238631369041E-16));
#41108=CARTESIAN_POINT('Ctrl Pts',(-33.7522580799673,42.4,-4.27239199200323));
#41109=CARTESIAN_POINT('Ctrl Pts',(-33.5855914133007,38.7,-6.40858798800485));
#41110=CARTESIAN_POINT('Ctrl Pts',(-33.418924746634,35.,-8.54478398400645));
#41111=CARTESIAN_POINT('Ctrl Pts',(-33.2522580799673,31.3,-6.40858798800485));
#41112=CARTESIAN_POINT('Ctrl Pts',(-33.0855914133007,27.6,-4.27239199200323));
#41113=CARTESIAN_POINT('Ctrl Pts',(-32.918924746634,27.6,0.));
#41114=CARTESIAN_POINT('Ctrl Pts',(-32.7522580799673,27.6,4.27239199200323));
#41115=CARTESIAN_POINT('Ctrl Pts',(-32.5855914133007,31.3,6.40858798800485));
#41116=CARTESIAN_POINT('Ctrl Pts',(-32.418924746634,35.,8.54478398400645));
#41117=CARTESIAN_POINT('Ctrl Pts',(-32.2522580799673,38.7,6.40858798800485));
#41118=CARTESIAN_POINT('Ctrl Pts',(-32.0855914133007,42.4,4.27239199200323));
#41119=CARTESIAN_POINT('Ctrl Pts',(-31.918924746634,42.4,9.06238631369041E-16));
#41120=CARTESIAN_POINT('Ctrl Pts',(-31.7522580799673,42.4,-4.27239199200323));
#41121=CARTESIAN_POINT('Ctrl Pts',(-31.5855914133007,38.7,-6.40858798800485));
#41122=CARTESIAN_POINT('Ctrl Pts',(-31.418924746634,35.,-8.54478398400645));
#41123=CARTESIAN_POINT('Ctrl Pts',(-31.2522580799673,31.3,-6.40858798800485));
#41124=CARTESIAN_POINT('Ctrl Pts',(-31.0855914133007,27.6,-4.27239199200323));
#41125=CARTESIAN_POINT('Ctrl Pts',(-30.918924746634,27.6,0.));
#41126=CARTESIAN_POINT('Ctrl Pts',(-30.7522580799673,27.6,4.27239199200323));
#41127=CARTESIAN_POINT('Ctrl Pts',(-30.5855914133007,31.3,6.40858798800485));
#41128=CARTESIAN_POINT('Ctrl Pts',(-30.418924746634,35.,8.54478398400645));
#41129=CARTESIAN_POINT('Ctrl Pts',(-30.2522580799673,38.7,6.40858798800485));
#41130=CARTESIAN_POINT('Ctrl Pts',(-30.0855914133007,42.4,4.27239199200323));
#41131=CARTESIAN_POINT('Ctrl Pts',(-29.918924746634,42.4,9.06238631369041E-16));
#41132=CARTESIAN_POINT('Ctrl Pts',(-29.7522580799673,42.4,-4.27239199200323));
#41133=CARTESIAN_POINT('Ctrl Pts',(-29.5855914133007,38.7,-6.40858798800485));
#41134=CARTESIAN_POINT('Ctrl Pts',(-29.418924746634,35.,-8.54478398400645));
#41135=CARTESIAN_POINT('Ctrl Pts',(-29.2522580799673,31.3,-6.40858798800485));
#41136=CARTESIAN_POINT('Ctrl Pts',(-29.0855914133007,27.6,-4.27239199200323));
#41137=CARTESIAN_POINT('Ctrl Pts',(-28.918924746634,27.6,0.));
#41138=CARTESIAN_POINT('Ctrl Pts',(-28.7522580799673,27.6,4.27239199200323));
#41139=CARTESIAN_POINT('Ctrl Pts',(-28.5855914133007,31.3,6.40858798800485));
#41140=CARTESIAN_POINT('Ctrl Pts',(-28.418924746634,35.,8.54478398400645));
#41141=CARTESIAN_POINT('Ctrl Pts',(-28.2522580799673,38.7,6.40858798800485));
#41142=CARTESIAN_POINT('Ctrl Pts',(-28.0855914133007,42.4,4.27239199200323));
#41143=CARTESIAN_POINT('Ctrl Pts',(-27.918924746634,42.4,9.06238631369041E-16));
#41144=CARTESIAN_POINT('Ctrl Pts',(-27.7522580799673,42.4,-4.27239199200323));
#41145=CARTESIAN_POINT('Ctrl Pts',(-27.5855914133007,38.7,-6.40858798800485));
#41146=CARTESIAN_POINT('Ctrl Pts',(-27.418924746634,35.,-8.54478398400645));
#41147=CARTESIAN_POINT('Ctrl Pts',(-27.2522580799673,31.3,-6.40858798800485));
#41148=CARTESIAN_POINT('Ctrl Pts',(-27.0855914133007,27.6,-4.27239199200323));
#41149=CARTESIAN_POINT('Ctrl Pts',(-26.918924746634,27.6,0.));
#41150=CARTESIAN_POINT('Ctrl Pts',(-26.7522580799673,27.6,4.27239199200323));
#41151=CARTESIAN_POINT('Ctrl Pts',(-26.5855914133007,31.3,6.40858798800485));
#41152=CARTESIAN_POINT('Ctrl Pts',(-26.418924746634,35.,8.54478398400645));
#41153=CARTESIAN_POINT('Ctrl Pts',(-26.2522580799673,38.7,6.40858798800485));
#41154=CARTESIAN_POINT('Ctrl Pts',(-26.0855914133007,42.4,4.27239199200323));
#41155=CARTESIAN_POINT('Ctrl Pts',(-25.918924746634,42.4,9.06238631369041E-16));
#41156=CARTESIAN_POINT('Ctrl Pts',(-25.7522580799673,42.4,-4.27239199200323));
#41157=CARTESIAN_POINT('Ctrl Pts',(-25.5855914133007,38.7,-6.40858798800485));
#41158=CARTESIAN_POINT('Ctrl Pts',(-25.418924746634,35.,-8.54478398400645));
#41159=CARTESIAN_POINT('Ctrl Pts',(-25.2522580799673,31.3,-6.40858798800485));
#41160=CARTESIAN_POINT('Ctrl Pts',(-25.0855914133007,27.6,-4.27239199200323));
#41161=CARTESIAN_POINT('Ctrl Pts',(-24.918924746634,27.6,0.));
#41162=CARTESIAN_POINT('Ctrl Pts',(-24.7522580799673,27.6,4.27239199200323));
#41163=CARTESIAN_POINT('Ctrl Pts',(-24.5855914133007,31.3,6.40858798800485));
#41164=CARTESIAN_POINT('Ctrl Pts',(-24.418924746634,35.,8.54478398400645));
#41165=CARTESIAN_POINT('Ctrl Pts',(-24.2522580799673,38.7,6.40858798800485));
#41166=CARTESIAN_POINT('Ctrl Pts',(-24.0855914133007,42.4,4.27239199200323));
#41167=CARTESIAN_POINT('Ctrl Pts',(-23.918924746634,42.4,9.06238631369041E-16));
#41168=CARTESIAN_POINT('Ctrl Pts',(-23.7522580799673,42.4,-4.27239199200323));
#41169=CARTESIAN_POINT('Ctrl Pts',(-23.5855914133007,38.7,-6.40858798800485));
#41170=CARTESIAN_POINT('Ctrl Pts',(-23.418924746634,35.,-8.54478398400645));
#41171=CARTESIAN_POINT('Ctrl Pts',(-23.2522580799673,31.3,-6.40858798800485));
#41172=CARTESIAN_POINT('Ctrl Pts',(-23.0855914133007,27.6,-4.27239199200323));
#41173=CARTESIAN_POINT('Ctrl Pts',(-22.918924746634,27.6,0.));
#41174=CARTESIAN_POINT('Ctrl Pts',(-22.7522580799673,27.6,4.27239199200323));
#41175=CARTESIAN_POINT('Ctrl Pts',(-22.5855914133007,31.3,6.40858798800485));
#41176=CARTESIAN_POINT('Ctrl Pts',(-22.418924746634,35.,8.54478398400645));
#41177=CARTESIAN_POINT('Ctrl Pts',(-22.2522580799673,38.7,6.40858798800485));
#41178=CARTESIAN_POINT('Ctrl Pts',(-22.0855914133007,42.4,4.27239199200323));
#41179=CARTESIAN_POINT('Ctrl Pts',(-21.918924746634,42.4,9.06238631369041E-16));
#41180=CARTESIAN_POINT('Ctrl Pts',(-21.7522580799673,42.4,-4.27239199200323));
#41181=CARTESIAN_POINT('Ctrl Pts',(-21.5855914133007,38.7,-6.40858798800485));
#41182=CARTESIAN_POINT('Ctrl Pts',(-21.418924746634,35.,-8.54478398400645));
#41183=CARTESIAN_POINT('Ctrl Pts',(-21.2522580799673,31.3,-6.40858798800485));
#41184=CARTESIAN_POINT('Ctrl Pts',(-21.0855914133007,27.6,-4.27239199200323));
#41185=CARTESIAN_POINT('Ctrl Pts',(-20.918924746634,27.6,0.));
#41186=CARTESIAN_POINT('Ctrl Pts',(-20.7522580799673,27.6,4.27239199200323));
#41187=CARTESIAN_POINT('Ctrl Pts',(-20.5855914133007,31.3,6.40858798800485));
#41188=CARTESIAN_POINT('Ctrl Pts',(-20.418924746634,35.,8.54478398400645));
#41189=CARTESIAN_POINT('Ctrl Pts',(-20.2522580799673,38.7,6.40858798800485));
#41190=CARTESIAN_POINT('Ctrl Pts',(-20.0855914133007,42.4,4.27239199200323));
#41191=CARTESIAN_POINT('Ctrl Pts',(-19.918924746634,42.4,9.06238631369041E-16));
#41192=CARTESIAN_POINT('Ctrl Pts',(-19.7522580799673,42.4,-4.27239199200323));
#41193=CARTESIAN_POINT('Ctrl Pts',(-19.5855914133007,38.7,-6.40858798800485));
#41194=CARTESIAN_POINT('Ctrl Pts',(-19.418924746634,35.,-8.54478398400645));
#41195=CARTESIAN_POINT('Ctrl Pts',(-19.2522580799673,31.3,-6.40858798800485));
#41196=CARTESIAN_POINT('Ctrl Pts',(-19.0855914133006,27.6,-4.27239199200323));
#41197=CARTESIAN_POINT('Ctrl Pts',(-18.918924746634,27.6,0.));
#41198=CARTESIAN_POINT('Ctrl Pts',(-18.7522580799673,27.6,4.27239199200323));
#41199=CARTESIAN_POINT('Ctrl Pts',(-18.5855914133007,31.3,6.40858798800485));
#41200=CARTESIAN_POINT('Ctrl Pts',(-18.418924746634,35.,8.54478398400645));
#41201=CARTESIAN_POINT('Ctrl Pts',(-18.2522580799673,38.7,6.40858798800485));
#41202=CARTESIAN_POINT('Ctrl Pts',(-18.0855914133007,42.4,4.27239199200323));
#41203=CARTESIAN_POINT('Ctrl Pts',(-17.918924746634,42.4,9.06238631369041E-16));
#41204=CARTESIAN_POINT('Ctrl Pts',(-17.7522580799673,42.4,-4.27239199200323));
#41205=CARTESIAN_POINT('Ctrl Pts',(-17.5855914133007,38.7,-6.40858798800485));
#41206=CARTESIAN_POINT('Ctrl Pts',(-17.418924746634,35.,-8.54478398400645));
#41207=CARTESIAN_POINT('Ctrl Pts',(-17.2522580799674,31.3,-6.40858798800485));
#41208=CARTESIAN_POINT('Ctrl Pts',(-17.0855914133007,27.6,-4.27239199200323));
#41209=CARTESIAN_POINT('Ctrl Pts',(-16.918924746634,27.6,0.));
#41210=CARTESIAN_POINT('Ctrl Pts',(-36.918924746634,26.,0.));
#41211=CARTESIAN_POINT('Ctrl Pts',(-36.7522580799673,26.,5.19615242270663));
#41212=CARTESIAN_POINT('Ctrl Pts',(-36.5855914133007,30.5,7.79422863405995));
#41213=CARTESIAN_POINT('Ctrl Pts',(-36.418924746634,35.,10.3923048454133));
#41214=CARTESIAN_POINT('Ctrl Pts',(-36.2522580799673,39.5,7.79422863405995));
#41215=CARTESIAN_POINT('Ctrl Pts',(-36.0855914133007,44.,5.19615242270663));
#41216=CARTESIAN_POINT('Ctrl Pts',(-35.918924746634,44.,1.10218211923262E-15));
#41217=CARTESIAN_POINT('Ctrl Pts',(-35.7522580799673,44.,-5.19615242270663));
#41218=CARTESIAN_POINT('Ctrl Pts',(-35.5855914133007,39.5,-7.79422863405995));
#41219=CARTESIAN_POINT('Ctrl Pts',(-35.418924746634,35.,-10.3923048454133));
#41220=CARTESIAN_POINT('Ctrl Pts',(-35.2522580799673,30.5,-7.79422863405995));
#41221=CARTESIAN_POINT('Ctrl Pts',(-35.0855914133007,26.,-5.19615242270663));
#41222=CARTESIAN_POINT('Ctrl Pts',(-34.918924746634,26.,0.));
#41223=CARTESIAN_POINT('Ctrl Pts',(-34.7522580799673,26.,5.19615242270663));
#41224=CARTESIAN_POINT('Ctrl Pts',(-34.5855914133007,30.5,7.79422863405995));
#41225=CARTESIAN_POINT('Ctrl Pts',(-34.418924746634,35.,10.3923048454133));
#41226=CARTESIAN_POINT('Ctrl Pts',(-34.2522580799673,39.5,7.79422863405995));
#41227=CARTESIAN_POINT('Ctrl Pts',(-34.0855914133007,44.,5.19615242270663));
#41228=CARTESIAN_POINT('Ctrl Pts',(-33.918924746634,44.,1.10218211923262E-15));
#41229=CARTESIAN_POINT('Ctrl Pts',(-33.7522580799673,44.,-5.19615242270663));
#41230=CARTESIAN_POINT('Ctrl Pts',(-33.5855914133007,39.5,-7.79422863405995));
#41231=CARTESIAN_POINT('Ctrl Pts',(-33.418924746634,35.,-10.3923048454133));
#41232=CARTESIAN_POINT('Ctrl Pts',(-33.2522580799673,30.5,-7.79422863405995));
#41233=CARTESIAN_POINT('Ctrl Pts',(-33.0855914133007,26.,-5.19615242270663));
#41234=CARTESIAN_POINT('Ctrl Pts',(-32.918924746634,26.,0.));
#41235=CARTESIAN_POINT('Ctrl Pts',(-32.7522580799673,26.,5.19615242270663));
#41236=CARTESIAN_POINT('Ctrl Pts',(-32.5855914133007,30.5,7.79422863405995));
#41237=CARTESIAN_POINT('Ctrl Pts',(-32.418924746634,35.,10.3923048454133));
#41238=CARTESIAN_POINT('Ctrl Pts',(-32.2522580799673,39.5,7.79422863405995));
#41239=CARTESIAN_POINT('Ctrl Pts',(-32.0855914133007,44.,5.19615242270663));
#41240=CARTESIAN_POINT('Ctrl Pts',(-31.918924746634,44.,1.10218211923262E-15));
#41241=CARTESIAN_POINT('Ctrl Pts',(-31.7522580799673,44.,-5.19615242270663));
#41242=CARTESIAN_POINT('Ctrl Pts',(-31.5855914133007,39.5,-7.79422863405995));
#41243=CARTESIAN_POINT('Ctrl Pts',(-31.418924746634,35.,-10.3923048454133));
#41244=CARTESIAN_POINT('Ctrl Pts',(-31.2522580799673,30.5,-7.79422863405995));
#41245=CARTESIAN_POINT('Ctrl Pts',(-31.0855914133007,26.,-5.19615242270663));
#41246=CARTESIAN_POINT('Ctrl Pts',(-30.918924746634,26.,0.));
#41247=CARTESIAN_POINT('Ctrl Pts',(-30.7522580799673,26.,5.19615242270663));
#41248=CARTESIAN_POINT('Ctrl Pts',(-30.5855914133007,30.5,7.79422863405995));
#41249=CARTESIAN_POINT('Ctrl Pts',(-30.418924746634,35.,10.3923048454133));
#41250=CARTESIAN_POINT('Ctrl Pts',(-30.2522580799673,39.5,7.79422863405995));
#41251=CARTESIAN_POINT('Ctrl Pts',(-30.0855914133007,44.,5.19615242270663));
#41252=CARTESIAN_POINT('Ctrl Pts',(-29.918924746634,44.,1.10218211923262E-15));
#41253=CARTESIAN_POINT('Ctrl Pts',(-29.7522580799673,44.,-5.19615242270663));
#41254=CARTESIAN_POINT('Ctrl Pts',(-29.5855914133007,39.5,-7.79422863405995));
#41255=CARTESIAN_POINT('Ctrl Pts',(-29.418924746634,35.,-10.3923048454133));
#41256=CARTESIAN_POINT('Ctrl Pts',(-29.2522580799673,30.5,-7.79422863405995));
#41257=CARTESIAN_POINT('Ctrl Pts',(-29.0855914133007,26.,-5.19615242270663));
#41258=CARTESIAN_POINT('Ctrl Pts',(-28.918924746634,26.,0.));
#41259=CARTESIAN_POINT('Ctrl Pts',(-28.7522580799673,26.,5.19615242270663));
#41260=CARTESIAN_POINT('Ctrl Pts',(-28.5855914133007,30.5,7.79422863405995));
#41261=CARTESIAN_POINT('Ctrl Pts',(-28.418924746634,35.,10.3923048454133));
#41262=CARTESIAN_POINT('Ctrl Pts',(-28.2522580799673,39.5,7.79422863405995));
#41263=CARTESIAN_POINT('Ctrl Pts',(-28.0855914133007,44.,5.19615242270663));
#41264=CARTESIAN_POINT('Ctrl Pts',(-27.918924746634,44.,1.10218211923262E-15));
#41265=CARTESIAN_POINT('Ctrl Pts',(-27.7522580799673,44.,-5.19615242270663));
#41266=CARTESIAN_POINT('Ctrl Pts',(-27.5855914133007,39.5,-7.79422863405995));
#41267=CARTESIAN_POINT('Ctrl Pts',(-27.418924746634,35.,-10.3923048454133));
#41268=CARTESIAN_POINT('Ctrl Pts',(-27.2522580799673,30.5,-7.79422863405995));
#41269=CARTESIAN_POINT('Ctrl Pts',(-27.0855914133007,26.,-5.19615242270663));
#41270=CARTESIAN_POINT('Ctrl Pts',(-26.918924746634,26.,0.));
#41271=CARTESIAN_POINT('Ctrl Pts',(-26.7522580799673,26.,5.19615242270663));
#41272=CARTESIAN_POINT('Ctrl Pts',(-26.5855914133007,30.5,7.79422863405995));
#41273=CARTESIAN_POINT('Ctrl Pts',(-26.418924746634,35.,10.3923048454133));
#41274=CARTESIAN_POINT('Ctrl Pts',(-26.2522580799673,39.5,7.79422863405995));
#41275=CARTESIAN_POINT('Ctrl Pts',(-26.0855914133007,44.,5.19615242270663));
#41276=CARTESIAN_POINT('Ctrl Pts',(-25.918924746634,44.,1.10218211923262E-15));
#41277=CARTESIAN_POINT('Ctrl Pts',(-25.7522580799673,44.,-5.19615242270663));
#41278=CARTESIAN_POINT('Ctrl Pts',(-25.5855914133007,39.5,-7.79422863405995));
#41279=CARTESIAN_POINT('Ctrl Pts',(-25.418924746634,35.,-10.3923048454133));
#41280=CARTESIAN_POINT('Ctrl Pts',(-25.2522580799673,30.5,-7.79422863405995));
#41281=CARTESIAN_POINT('Ctrl Pts',(-25.0855914133007,26.,-5.19615242270663));
#41282=CARTESIAN_POINT('Ctrl Pts',(-24.918924746634,26.,0.));
#41283=CARTESIAN_POINT('Ctrl Pts',(-24.7522580799673,26.,5.19615242270663));
#41284=CARTESIAN_POINT('Ctrl Pts',(-24.5855914133007,30.5,7.79422863405995));
#41285=CARTESIAN_POINT('Ctrl Pts',(-24.418924746634,35.,10.3923048454133));
#41286=CARTESIAN_POINT('Ctrl Pts',(-24.2522580799673,39.5,7.79422863405995));
#41287=CARTESIAN_POINT('Ctrl Pts',(-24.0855914133007,44.,5.19615242270663));
#41288=CARTESIAN_POINT('Ctrl Pts',(-23.918924746634,44.,1.10218211923262E-15));
#41289=CARTESIAN_POINT('Ctrl Pts',(-23.7522580799673,44.,-5.19615242270663));
#41290=CARTESIAN_POINT('Ctrl Pts',(-23.5855914133007,39.5,-7.79422863405995));
#41291=CARTESIAN_POINT('Ctrl Pts',(-23.418924746634,35.,-10.3923048454133));
#41292=CARTESIAN_POINT('Ctrl Pts',(-23.2522580799673,30.5,-7.79422863405995));
#41293=CARTESIAN_POINT('Ctrl Pts',(-23.0855914133007,26.,-5.19615242270663));
#41294=CARTESIAN_POINT('Ctrl Pts',(-22.918924746634,26.,0.));
#41295=CARTESIAN_POINT('Ctrl Pts',(-22.7522580799673,26.,5.19615242270663));
#41296=CARTESIAN_POINT('Ctrl Pts',(-22.5855914133007,30.5,7.79422863405995));
#41297=CARTESIAN_POINT('Ctrl Pts',(-22.418924746634,35.,10.3923048454133));
#41298=CARTESIAN_POINT('Ctrl Pts',(-22.2522580799674,39.5,7.79422863405995));
#41299=CARTESIAN_POINT('Ctrl Pts',(-22.0855914133007,44.,5.19615242270663));
#41300=CARTESIAN_POINT('Ctrl Pts',(-21.918924746634,44.,1.10218211923262E-15));
#41301=CARTESIAN_POINT('Ctrl Pts',(-21.7522580799673,44.,-5.19615242270663));
#41302=CARTESIAN_POINT('Ctrl Pts',(-21.5855914133006,39.5,-7.79422863405995));
#41303=CARTESIAN_POINT('Ctrl Pts',(-21.418924746634,35.,-10.3923048454133));
#41304=CARTESIAN_POINT('Ctrl Pts',(-21.2522580799673,30.5,-7.79422863405995));
#41305=CARTESIAN_POINT('Ctrl Pts',(-21.0855914133007,26.,-5.19615242270663));
#41306=CARTESIAN_POINT('Ctrl Pts',(-20.918924746634,26.,0.));
#41307=CARTESIAN_POINT('Ctrl Pts',(-20.7522580799673,26.,5.19615242270663));
#41308=CARTESIAN_POINT('Ctrl Pts',(-20.5855914133006,30.5,7.79422863405995));
#41309=CARTESIAN_POINT('Ctrl Pts',(-20.418924746634,35.,10.3923048454133));
#41310=CARTESIAN_POINT('Ctrl Pts',(-20.2522580799673,39.5,7.79422863405995));
#41311=CARTESIAN_POINT('Ctrl Pts',(-20.0855914133007,44.,5.19615242270663));
#41312=CARTESIAN_POINT('Ctrl Pts',(-19.918924746634,44.,1.10218211923262E-15));
#41313=CARTESIAN_POINT('Ctrl Pts',(-19.7522580799674,44.,-5.19615242270663));
#41314=CARTESIAN_POINT('Ctrl Pts',(-19.5855914133006,39.5,-7.79422863405995));
#41315=CARTESIAN_POINT('Ctrl Pts',(-19.418924746634,35.,-10.3923048454133));
#41316=CARTESIAN_POINT('Ctrl Pts',(-19.2522580799674,30.5,-7.79422863405995));
#41317=CARTESIAN_POINT('Ctrl Pts',(-19.0855914133007,26.,-5.19615242270663));
#41318=CARTESIAN_POINT('Ctrl Pts',(-18.918924746634,26.,0.));
#41319=CARTESIAN_POINT('Ctrl Pts',(-18.7522580799673,26.,5.19615242270663));
#41320=CARTESIAN_POINT('Ctrl Pts',(-18.5855914133006,30.5,7.79422863405995));
#41321=CARTESIAN_POINT('Ctrl Pts',(-18.418924746634,35.,10.3923048454133));
#41322=CARTESIAN_POINT('Ctrl Pts',(-18.2522580799673,39.5,7.79422863405995));
#41323=CARTESIAN_POINT('Ctrl Pts',(-18.0855914133006,44.,5.19615242270663));
#41324=CARTESIAN_POINT('Ctrl Pts',(-17.918924746634,44.,1.10218211923262E-15));
#41325=CARTESIAN_POINT('Ctrl Pts',(-17.7522580799673,44.,-5.19615242270663));
#41326=CARTESIAN_POINT('Ctrl Pts',(-17.5855914133006,39.5,-7.79422863405995));
#41327=CARTESIAN_POINT('Ctrl Pts',(-17.418924746634,35.,-10.3923048454133));
#41328=CARTESIAN_POINT('Ctrl Pts',(-17.2522580799673,30.5,-7.79422863405995));
#41329=CARTESIAN_POINT('Ctrl Pts',(-17.0855914133007,26.,-5.19615242270663));
#41330=CARTESIAN_POINT('Ctrl Pts',(-16.918924746634,26.,0.));
#41331=CARTESIAN_POINT('Origin',(-42.,34.999999994595,6.55E-10));
#41332=CARTESIAN_POINT('',(-42.,38.0494565603535,5.1672831023974));
#41333=CARTESIAN_POINT('',(-42.,40.65404535889,-2.00792704445741));
#41334=CARTESIAN_POINT('Origin',(-46.,44.2399040040528,-4.98740151676925));
#41335=CARTESIAN_POINT('',(-42.5,40.1413699032525,-3.09294608072936));
#41336=CARTESIAN_POINT('',(-42.5,40.1413699032525,-3.09294608072936));
#41337=CARTESIAN_POINT('',(-45.5,40.1413699032525,-3.09294608072936));
#41338=CARTESIAN_POINT('',(-42.,40.1413699032525,-3.09294608072936));
#41339=CARTESIAN_POINT('',(-45.5,44.2399040040528,-4.98740151676925));
#41340=CARTESIAN_POINT('Origin',(-46.,44.7486243140984,-3.90055430318255));
#41341=CARTESIAN_POINT('',(-42.5,44.7486243140985,-3.90055430318256));
#41342=CARTESIAN_POINT('',(-46.,44.7486243140984,-3.90055430318255));
#41343=CARTESIAN_POINT('',(-45.5,44.7486243140984,-3.90055430318255));
#41344=CARTESIAN_POINT('Origin',(-46.,35.7752519450148,0.24718575365908));
#41345=CARTESIAN_POINT('',(-46.,39.9429588225849,9.26375507215795));
#41346=CARTESIAN_POINT('',(-42.5,38.0494565603535,5.1672831023974));
#41347=CARTESIAN_POINT('',(-45.5,35.7752519450148,0.24718575365908));
#41348=CARTESIAN_POINT('Origin',(-46.,34.6859864596583,0.750674286210626));
#41349=CARTESIAN_POINT('',(-45.5,36.9601910749969,5.67077163494895));
#41350=CARTESIAN_POINT('',(-42.5,36.9601910749969,5.67077163494895));
#41351=CARTESIAN_POINT('',(-42.,36.9601910749969,5.67077163494895));
#41352=CARTESIAN_POINT('',(-42.5,38.8536933372283,9.7672436047095));
#41353=CARTESIAN_POINT('',(-42.5,38.8536933372283,9.7672436047095));
#41354=CARTESIAN_POINT('',(-45.5,38.8536933372283,9.7672436047095));
#41355=CARTESIAN_POINT('',(-46.,38.8536933372283,9.7672436047095));
#41356=CARTESIAN_POINT('',(-45.5,34.6859864596583,0.750674286210626));
#41357=CARTESIAN_POINT('Origin',(-46.,32.151915435741,0.600000000655));
#41358=CARTESIAN_POINT('',(-45.5,29.3128914363174,1.91227514988591));
#41359=CARTESIAN_POINT('',(-42.5,29.3128914363174,1.91227514988591));
#41360=CARTESIAN_POINT('',(-42.,29.3128914363174,1.91227514988591));
#41361=CARTESIAN_POINT('',(-42.5,25.2143573355172,3.80673058592581));
#41362=CARTESIAN_POINT('',(-42.5,25.6691348322782,3.59651989114122));
#41363=CARTESIAN_POINT('',(-45.5,25.2143573355172,3.80673058592581));
#41364=CARTESIAN_POINT('',(-46.,25.2143573355172,3.80673058592581));
#41365=CARTESIAN_POINT('',(-45.5,32.151915435741,0.600000000655));
#41366=CARTESIAN_POINT('Origin',(-46.,34.6859864596583,0.750674286210626));
#41367=CARTESIAN_POINT('',(-45.5,25.7126140905746,4.89841434305227));
#41368=CARTESIAN_POINT('',(-42.5,25.7126140905746,4.89841434305227));
#41369=CARTESIAN_POINT('',(-46.,25.7126140905746,4.89841434305227));
#41370=CARTESIAN_POINT('',(-42.5,29.807193045783,3.00578708432712));
#41371=CARTESIAN_POINT('',(-42.5,29.807193045783,3.00578708432712));
#41372=CARTESIAN_POINT('',(-45.5,29.807193045783,3.00578708432712));
#41373=CARTESIAN_POINT('',(-42.,29.807193045783,3.00578708432712));
#41374=CARTESIAN_POINT('',(-45.5,34.6859864596583,0.750674286210626));
#41375=CARTESIAN_POINT('Origin',(-34.5,20.2255401693197,-2.54750793782168));
#41376=CARTESIAN_POINT('',(-38.5,20.2255401693197,-0.0980181950384988));
#41377=CARTESIAN_POINT('Origin',(-45.5,35.0208323137734,0.0450694010362789));
#41378=CARTESIAN_POINT('',(-46.,35.0208323137734,0.0450694010362797));
#41379=CARTESIAN_POINT('Origin',(-45.5,35.0907721183747,-0.0419573770576284));
#41380=CARTESIAN_POINT('',(-46.,35.0907721183747,-0.0419573770576286));
#41381=CARTESIAN_POINT('Origin',(-45.5,34.999999994595,6.55E-10));
#41382=CARTESIAN_POINT('',(-46.,25.0360004143143,4.66033393334341));
#41383=CARTESIAN_POINT('Ctrl Pts',(-46.,25.0360004143144,4.66033393334341));
#41384=CARTESIAN_POINT('Ctrl Pts',(-46.,25.0374024690213,4.66084598634663));
#41385=CARTESIAN_POINT('Ctrl Pts',(-45.9999966731511,25.0388045641603,4.66135793950374));
#41386=CARTESIAN_POINT('Ctrl Pts',(-45.9996492133389,25.1120391418205,4.68809241397306));
#41387=CARTESIAN_POINT('Ctrl Pts',(-45.9905781028549,25.1844197231217,4.7142058989083));
#41388=CARTESIAN_POINT('Ctrl Pts',(-45.9554702797948,25.3212199515064,4.76299808794914));
#41389=CARTESIAN_POINT('Ctrl Pts',(-45.929938447608,25.386863762187,4.78613722556436));
#41390=CARTESIAN_POINT('Ctrl Pts',(-45.8613791715261,25.5071706542225,4.82812523107859));
#41391=CARTESIAN_POINT('Ctrl Pts',(-45.8179795164162,25.5630011722499,4.84738471823477));
#41392=CARTESIAN_POINT('Ctrl Pts',(-45.7258076109511,25.6418150671328,4.87438209952366));
#41393=CARTESIAN_POINT('Ctrl Pts',(-45.6815277725054,25.6694803280007,4.88379024826762));
#41394=CARTESIAN_POINT('Ctrl Pts',(-45.5903579073579,25.7039748155375,4.89549515091947));
#41395=CARTESIAN_POINT('Ctrl Pts',(-45.5458624658048,25.712577506522,4.89840196573932));
#41396=CARTESIAN_POINT('Ctrl Pts',(-45.5001938310099,25.7126140518,4.8984143299332));
#41397=CARTESIAN_POINT('Ctrl Pts',(-45.5000969130038,25.7126140905746,4.89841434305228));
#41398=CARTESIAN_POINT('Ctrl Pts',(-45.5,25.7126140905746,4.89841434305228));
#41399=CARTESIAN_POINT('',(-46.,39.5243486999107,10.0264783850484));
#41400=CARTESIAN_POINT('Origin',(-46.,34.999999994595,6.55E-10));
#41401=CARTESIAN_POINT('Ctrl Pts',(-45.5,38.8536933372283,9.76724360470951));
#41402=CARTESIAN_POINT('Ctrl Pts',(-45.5475202328384,38.8536933372283,9.76724360470951));
#41403=CARTESIAN_POINT('Ctrl Pts',(-45.5938300790285,38.8628412828318,9.77091254431395));
#41404=CARTESIAN_POINT('Ctrl Pts',(-45.6926831164288,38.9011133206408,9.78620047778414));
#41405=CARTESIAN_POINT('Ctrl Pts',(-45.7416688429774,38.9337902963357,9.79922369582153));
#41406=CARTESIAN_POINT('Ctrl Pts',(-45.8419265836025,39.0270141336349,9.83609034985595));
#41407=CARTESIAN_POINT('Ctrl Pts',(-45.8908401903905,39.0968099336531,9.86350378153489));
#41408=CARTESIAN_POINT('Ctrl Pts',(-45.9741804024576,39.2809978199734,9.93476534492679));
#41409=CARTESIAN_POINT('Ctrl Pts',(-45.999416722443,39.399345156675,9.9798386246279));
#41410=CARTESIAN_POINT('Ctrl Pts',(-45.9999966732101,39.5215452282668,10.0254327281341));
#41411=CARTESIAN_POINT('Ctrl Pts',(-46.,39.5229469469093,10.0259556080299));
#41412=CARTESIAN_POINT('Ctrl Pts',(-46.,39.5243486999107,10.0264783850484));
#41413=CARTESIAN_POINT('Origin',(-45.5,34.999999994595,6.55E-10));
#41414=CARTESIAN_POINT('Origin',(-45.5,34.9092278708153,0.0419573783676288));
#41415=CARTESIAN_POINT('',(-46.,37.216502182775,5.03359891691694));
#41416=CARTESIAN_POINT('',(-46.,34.9092278708153,0.0419573783676291));
#41417=CARTESIAN_POINT('Ctrl Pts',(-45.5,36.9601910749969,5.67077163494895));
#41418=CARTESIAN_POINT('Ctrl Pts',(-45.548970157778,36.9601910749969,5.67077163494895));
#41419=CARTESIAN_POINT('Ctrl Pts',(-45.5969081567834,36.9639934004896,5.66185790620149));
#41420=CARTESIAN_POINT('Ctrl Pts',(-45.6935221969332,36.9791200174418,5.62617368236302));
#41421=CARTESIAN_POINT('Ctrl Pts',(-45.7398209612911,36.9910294096094,5.59799230724864));
#41422=CARTESIAN_POINT('Ctrl Pts',(-45.8328892935188,37.0240200249968,5.51906769418711));
#41423=CARTESIAN_POINT('Ctrl Pts',(-45.8753161788561,37.0465011132908,5.46473906324288));
#41424=CARTESIAN_POINT('Ctrl Pts',(-45.9385897729845,37.0925851272751,5.35135036405417));
#41425=CARTESIAN_POINT('Ctrl Pts',(-45.9609910872761,37.1161401001897,5.29255243634324));
#41426=CARTESIAN_POINT('Ctrl Pts',(-45.9918589780635,37.164790965817,5.16888552792546));
#41427=CARTESIAN_POINT('Ctrl Pts',(-45.9996751413526,37.1901469176321,5.10324005942292));
#41428=CARTESIAN_POINT('Ctrl Pts',(-45.9999966939211,37.2154612250376,5.03635122598603));
#41429=CARTESIAN_POINT('Ctrl Pts',(-46.,37.2159818012366,5.03497510643485));
#41430=CARTESIAN_POINT('Ctrl Pts',(-46.,37.2165021827753,5.03359891691704));
#41431=CARTESIAN_POINT('Origin',(-45.5,35.0208323137734,0.0450694010362796));
#41432=CARTESIAN_POINT('',(-46.,30.0285689416169,2.35263114162986));
#41433=CARTESIAN_POINT('Ctrl Pts',(-46.,30.0285689416169,2.35263114162986));
#41434=CARTESIAN_POINT('Ctrl Pts',(-46.,30.0280650993038,2.3540204371795));
#41435=CARTESIAN_POINT('Ctrl Pts',(-45.9999966944273,30.0275614528911,2.35540980745037));
#41436=CARTESIAN_POINT('Ctrl Pts',(-45.9996738586582,30.0029878258742,2.42322916399792));
#41437=CARTESIAN_POINT('Ctrl Pts',(-45.9917939389854,29.979263333268,2.49014276072554));
#41438=CARTESIAN_POINT('Ctrl Pts',(-45.9606603025493,29.9352867624643,2.61669625614254));
#41439=CARTESIAN_POINT('Ctrl Pts',(-45.938073114642,29.914713691535,2.67712605416832));
#41440=CARTESIAN_POINT('Ctrl Pts',(-45.8744779446781,29.8757270841149,2.79357023434024));
#41441=CARTESIAN_POINT('Ctrl Pts',(-45.8320302750286,29.8574143381371,2.84943977548591));
#41442=CARTESIAN_POINT('Ctrl Pts',(-45.7390416503862,29.8311027950442,2.93069950697313));
#41443=CARTESIAN_POINT('Ctrl Pts',(-45.6928616793168,29.8218160767511,2.95976786559309));
#41444=CARTESIAN_POINT('Ctrl Pts',(-45.5965455901766,29.8101006897299,2.9965789582576));
#41445=CARTESIAN_POINT('Ctrl Pts',(-45.5487893624249,29.807193045783,3.00578708432712));
#41446=CARTESIAN_POINT('Ctrl Pts',(-45.5,29.807193045783,3.00578708432712));
#41447=CARTESIAN_POINT('',(-46.,35.0208323137734,0.0450694010362801));
#41448=CARTESIAN_POINT('Origin',(-42.5,44.9584112026616,-3.44669368428398));
#41449=CARTESIAN_POINT('',(-42.,40.8638322474532,-1.55406642555884));
#41450=CARTESIAN_POINT('Origin',(-42.5,36.2291125639134,0.0373988650959357));
#41451=CARTESIAN_POINT('',(-42.,40.3968194414835,9.05396818359482));
#41452=CARTESIAN_POINT('Origin',(-42.5,34.999999994595,6.55E-10));
#41453=CARTESIAN_POINT('',(-42.,28.7102900092541,1.63998423847662));
#41454=CARTESIAN_POINT('Ctrl Pts',(-42.,28.7102900092541,1.63998423847662));
#41455=CARTESIAN_POINT('Ctrl Pts',(-42.,28.7115300500983,1.64057011650148));
#41456=CARTESIAN_POINT('Ctrl Pts',(-42.0000033207593,28.7127701523771,1.64115586956709));
#41457=CARTESIAN_POINT('Ctrl Pts',(-42.0004541950922,28.796981233661,1.68092188321178));
#41458=CARTESIAN_POINT('Ctrl Pts',(-42.0157573105942,28.8807676884173,1.71976480349444));
#41459=CARTESIAN_POINT('Ctrl Pts',(-42.0728019198682,29.0291511352119,1.78736590420412));
#41460=CARTESIAN_POINT('Ctrl Pts',(-42.1117195110958,29.0957873621205,1.81719592643935));
#41461=CARTESIAN_POINT('Ctrl Pts',(-42.2018967293794,29.195960411313,1.86148481105511));
#41462=CARTESIAN_POINT('Ctrl Pts',(-42.2479008339596,29.2336465552485,1.87794439145772));
#41463=CARTESIAN_POINT('Ctrl Pts',(-42.3442168820676,29.2851395596278,1.90031310744936));
#41464=CARTESIAN_POINT('Ctrl Pts',(-42.3916288820851,29.3014155492391,1.90732915008605));
#41465=CARTESIAN_POINT('Ctrl Pts',(-42.4610040616797,29.3114870702353,1.91167044475591));
#41466=CARTESIAN_POINT('Ctrl Pts',(-42.4805205119926,29.3128914363174,1.91227514988591));
#41467=CARTESIAN_POINT('Ctrl Pts',(-42.5,29.3128914363174,1.91227514988591));
#41468=CARTESIAN_POINT('',(-42.5,29.0300753719553,0.600000000655));
#41469=CARTESIAN_POINT('Origin',(-42.5,34.999999994595,6.55E-10));
#41470=CARTESIAN_POINT('',(-42.,28.5937530433762,1.100000000655));
#41471=CARTESIAN_POINT('Ctrl Pts',(-42.,28.5937530433762,1.100000000655));
#41472=CARTESIAN_POINT('Ctrl Pts',(-42.,28.5946398535677,1.09894794045397));
#41473=CARTESIAN_POINT('Ctrl Pts',(-42.0000033204919,28.5955267728317,1.0978959693116));
#41474=CARTESIAN_POINT('Ctrl Pts',(-42.0004662363704,28.6573726864835,1.02455603604737));
#41475=CARTESIAN_POINT('Ctrl Pts',(-42.0165992209748,28.7192952337357,0.952209618319868));
#41476=CARTESIAN_POINT('Ctrl Pts',(-42.0758441660175,28.8273260851525,0.82772417571545));
#41477=CARTESIAN_POINT('Ctrl Pts',(-42.1151456113167,28.8751198610887,0.773377665751314));
#41478=CARTESIAN_POINT('Ctrl Pts',(-42.2056695167071,28.9469442910977,0.692456560469139));
#41479=CARTESIAN_POINT('Ctrl Pts',(-42.2516602512676,28.9739516189116,0.662301438777017));
#41480=CARTESIAN_POINT('Ctrl Pts',(-42.34779518891,29.0107522579474,0.621371214703135));
#41481=CARTESIAN_POINT('Ctrl Pts',(-42.3950686181707,29.0223139734333,0.608583817890182));
#41482=CARTESIAN_POINT('Ctrl Pts',(-42.4631644468274,29.029156829769,0.601015248913021));
#41483=CARTESIAN_POINT('Ctrl Pts',(-42.4816022135789,29.0300753719553,0.600000000655));
#41484=CARTESIAN_POINT('Ctrl Pts',(-42.5,29.0300753719553,0.600000000655));
#41485=CARTESIAN_POINT('Origin',(-42.,34.999999994595,6.55E-10));
#41486=CARTESIAN_POINT('Origin',(-41.5,25.2185048259584,-6.04750793782168));
#41487=CARTESIAN_POINT('',(-41.5,25.2185048259584,-5.04750793782168));
#41488=CARTESIAN_POINT('',(-42.,25.2185048259584,-4.54750793782168));
#41489=CARTESIAN_POINT('Origin',(-41.5,25.2185048259584,-4.54750793782167));
#41490=CARTESIAN_POINT('',(-42.,26.4943520218675,-5.25870255454211));
#41491=CARTESIAN_POINT('Origin',(-42.,25.2185048259584,-6.04750793782168));
#41492=CARTESIAN_POINT('',(-41.5,26.0690696232311,-5.52163768230196));
#41493=CARTESIAN_POINT('Origin',(-41.5,26.4943520218675,-5.25870255454211));
#41494=CARTESIAN_POINT('Origin',(-41.5,25.2185048259584,-6.04750793782168));
#41495=CARTESIAN_POINT('Origin',(-41.5,34.999999994595,-4.54750793782168));
#41496=CARTESIAN_POINT('',(-42.,34.999999994595,-4.54750793782168));
#41497=CARTESIAN_POINT('',(-41.5,20.7255401693197,-5.04750793782167));
#41498=CARTESIAN_POINT('Origin',(-40.,34.999999994595,6.55E-10));
#41499=CARTESIAN_POINT('',(-40.,52.6486129734088,-3.5392739254555));
#41500=CARTESIAN_POINT('',(-40.,52.9941026808875,0.460726074544506));
#41501=CARTESIAN_POINT('Origin',(-40.,34.999999994595,6.54998265276524E-10));
#41502=CARTESIAN_POINT('',(-40.,56.5946168001448,0.460726074544506));
#41503=CARTESIAN_POINT('',(-40.,56.5946168001448,0.460726074544506));
#41504=CARTESIAN_POINT('',(-40.,56.5946168001448,-3.5392739254555));
#41505=CARTESIAN_POINT('',(-40.,56.5946168001448,-3.5392739254555));
#41506=CARTESIAN_POINT('',(-40.,48.5946168001447,-3.5392739254555));
#41507=CARTESIAN_POINT('Ctrl Pts',(-38.8535045584117,49.0947070026403,3.3142306281657));
#41508=CARTESIAN_POINT('Ctrl Pts',(-39.,49.09474437335,3.46068560589431));
#41509=CARTESIAN_POINT('Ctrl Pts',(-39.,49.0947972300504,3.66783283265958));
#41510=CARTESIAN_POINT('Ctrl Pts',(-38.8535080713606,49.067246177754,3.31424116296626));
#41511=CARTESIAN_POINT('Ctrl Pts',(-38.9999999999999,49.0559066742947,3.46069849069773));
#41512=CARTESIAN_POINT('Ctrl Pts',(-39.,49.0398679954685,3.66784688025153));
#41513=CARTESIAN_POINT('Ctrl Pts',(-38.8519073632856,49.0397855966119,3.30944090472416));
#41514=CARTESIAN_POINT('Ctrl Pts',(-39.,49.0169980247426,3.45482188858408));
#41515=CARTESIAN_POINT('Ctrl Pts',(-39.,48.9849392151471,3.66144599708733));
#41516=CARTESIAN_POINT('Ctrl Pts',(-38.8455443417981,48.9856360525285,3.29035917900804));
#41517=CARTESIAN_POINT('Ctrl Pts',(-39.,48.9409553642149,3.43158518892926));
#41518=CARTESIAN_POINT('Ctrl Pts',(-39.,48.8766256560199,3.63600161677062));
#41519=CARTESIAN_POINT('Ctrl Pts',(-38.8407855746403,48.9589470995131,3.27608834575365));
#41520=CARTESIAN_POINT('Ctrl Pts',(-39.,48.9036879387245,3.4141524411812));
#41521=CARTESIAN_POINT('Ctrl Pts',(-39.,48.8232408334419,3.61697226872685));
#41522=CARTESIAN_POINT('Ctrl Pts',(-38.8282385003299,48.9070311494151,3.23846128171868));
#41523=CARTESIAN_POINT('Ctrl Pts',(-39.,48.8324120146563,3.36848126327577));
#41524=CARTESIAN_POINT('Ctrl Pts',(-39.,48.7193964919575,3.56679887235799));
#41525=CARTESIAN_POINT('Ctrl Pts',(-38.8204503561327,48.8818047904229,3.21510553874763));
#41526=CARTESIAN_POINT('Ctrl Pts',(-39.,48.798299096021,3.34007866638608));
#41527=CARTESIAN_POINT('Ctrl Pts',(-39.,48.6689381953401,3.53565541494599));
#41528=CARTESIAN_POINT('Ctrl Pts',(-38.8020550847506,48.8334958478087,3.15993971871678));
#41529=CARTESIAN_POINT('Ctrl Pts',(-39.,48.7347624479236,3.27350216862877));
#41530=CARTESIAN_POINT('Ctrl Pts',(-39.,48.5723110828561,3.46209545845528));
#41531=CARTESIAN_POINT('Ctrl Pts',(-38.7914481963086,48.8104138547599,3.12813035637803));
#41532=CARTESIAN_POINT('Ctrl Pts',(-39.,48.7052783560689,3.2350973112));
#41533=CARTESIAN_POINT('Ctrl Pts',(-39.,48.5261434083848,3.41967982872211));
#41534=CARTESIAN_POINT('Ctrl Pts',(-38.7677022294448,48.7670175509742,3.05691688025654));
#41535=CARTESIAN_POINT('Ctrl Pts',(-39.,48.6522917384422,3.14989967862306));
#41536=CARTESIAN_POINT('Ctrl Pts',(-39.,48.4393457551925,3.32472194096288));
#41537=CARTESIAN_POINT('Ctrl Pts',(-38.754563458535,48.7467037654173,3.01751368713769));
#41538=CARTESIAN_POINT('Ctrl Pts',(-39.,48.6287878978116,3.10282744096632));
#41539=CARTESIAN_POINT('Ctrl Pts',(-39.,48.3987168054773,3.2721808091293));
#41540=CARTESIAN_POINT('Ctrl Pts',(-38.7261089954399,48.7093930151617,2.93217742113975));
#41541=CARTESIAN_POINT('Ctrl Pts',(-39.,48.5888782841862,3.00200407984343));
#41542=CARTESIAN_POINT('Ctrl Pts',(-39.,48.3240951111972,3.15839209372811));
#41543=CARTESIAN_POINT('Ctrl Pts',(-38.7107936702028,48.6923964942063,2.88624544697246));
#41544=CARTESIAN_POINT('Ctrl Pts',(-39.,48.5725424429904,2.94794928112244));
#41545=CARTESIAN_POINT('Ctrl Pts',(-39.,48.2901032541095,3.09714586388256));
#41546=CARTESIAN_POINT('Ctrl Pts',(-38.6784002298215,48.6621798063133,2.78909300074232));
#41547=CARTESIAN_POINT('Ctrl Pts',(-39.,48.5478707626514,2.83517053538946));
#41548=CARTESIAN_POINT('Ctrl Pts',(-39.,48.2296748519216,2.96760249981115));
#41549=CARTESIAN_POINT('Ctrl Pts',(-38.6613225297323,48.6489599882654,2.73787377156343));
#41550=CARTESIAN_POINT('Ctrl Pts',(-39.,48.5396844114206,2.77614897370115));
#41551=CARTESIAN_POINT('Ctrl Pts',(-39.,48.2032390273215,2.89930691056257));
#41552=CARTESIAN_POINT('Ctrl Pts',(-38.6258661281208,48.6266542170724,2.63153115721682));
#41553=CARTESIAN_POINT('Ctrl Pts',(-39.0000000000001,48.5319565439657,2.65572283557889));
#41554=CARTESIAN_POINT('Ctrl Pts',(-39.,48.1586375470106,2.75751099023676));
#41555=CARTESIAN_POINT('Ctrl Pts',(-38.6074878768702,48.6175685077662,2.57640912054356));
#41556=CARTESIAN_POINT('Ctrl Pts',(-39.,48.5326470103469,2.59406293637931));
#41557=CARTESIAN_POINT('Ctrl Pts',(-39.,48.140472424078,2.68401235333488));
#41558=CARTESIAN_POINT('Ctrl Pts',(-38.5699273237463,48.60377678196,2.46375077843951));
#41559=CARTESIAN_POINT('Ctrl Pts',(-39.,48.543008106918,2.47090089780404));
#41560=CARTESIAN_POINT('Ctrl Pts',(-39.,48.1129036282315,2.53379720651331));
#41561=CARTESIAN_POINT('Ctrl Pts',(-38.5507454934032,48.5990708976697,2.40621588532438));
#41562=CARTESIAN_POINT('Ctrl Pts',(-38.9999999999999,48.5529886102347,2.40922780847103));
#41563=CARTESIAN_POINT('Ctrl Pts',(-39.,48.1035002850315,2.4570824934803));
#41564=CARTESIAN_POINT('Ctrl Pts',(-38.5120964494218,48.5941663241322,2.29028699517654));
#41565=CARTESIAN_POINT('Ctrl Pts',(-39.0000000000001,48.5818825838363,2.28881570408228));
#41566=CARTESIAN_POINT('Ctrl Pts',(-39.,48.0937094722848,2.30250905646815));
#41567=CARTESIAN_POINT('Ctrl Pts',(-38.49262971406,48.5939676527499,2.23189443078616));
#41568=CARTESIAN_POINT('Ctrl Pts',(-38.9999999999999,48.6011682984858,2.23003752380745));
#41569=CARTESIAN_POINT('Ctrl Pts',(-39.,48.0933221199033,2.22465218259804));
#41570=CARTESIAN_POINT('Ctrl Pts',(-38.4539372108061,48.5980832374213,2.11582860920987));
#41571=CARTESIAN_POINT('Ctrl Pts',(-39.0000000000001,48.6481312853257,2.11840511180508));
#41572=CARTESIAN_POINT('Ctrl Pts',(-39.,48.1015739764395,2.06989921432186));
#41573=CARTESIAN_POINT('Ctrl Pts',(-38.4347119133934,48.6023973982706,2.05815676133583));
#41574=CARTESIAN_POINT('Ctrl Pts',(-38.9999999999999,48.6762114086241,2.06569441899641));
#41575=CARTESIAN_POINT('Ctrl Pts',(-39.,48.1102130866064,1.99300497221786));
#41576=CARTESIAN_POINT('Ctrl Pts',(-38.3970220794501,48.6154224582525,1.94509137355602));
#41577=CARTESIAN_POINT('Ctrl Pts',(-39.0000000000001,48.7395494710663,1.9693555563745));
#41578=CARTESIAN_POINT('Ctrl Pts',(-39.,48.1362845305971,1.84225608507716));
#41579=CARTESIAN_POINT('Ctrl Pts',(-38.3785579915537,48.6241331544289,1.88969917736693));
#41580=CARTESIAN_POINT('Ctrl Pts',(-38.9999999999999,48.7751847398666,1.92610272382598));
#41581=CARTESIAN_POINT('Ctrl Pts',(-39.,48.153716552592,1.76840324344311));
#41582=CARTESIAN_POINT('Ctrl Pts',(-38.3518067382149,48.6403205713055,1.80944249844404));
#41583=CARTESIAN_POINT('Ctrl Pts',(-39.,48.8316806212018,1.87113650918206));
#41584=CARTESIAN_POINT('Ctrl Pts',(-39.,48.1861062119123,1.66140116307555));
#41585=CARTESIAN_POINT('Ctrl Pts',(-38.3430469593461,48.6462356653694,1.78316168828865));
#41586=CARTESIAN_POINT('Ctrl Pts',(-39.,48.8514141523639,1.85423124984201));
#41587=CARTESIAN_POINT('Ctrl Pts',(-39.,48.1979412146227,1.62636250356297));
#41588=CARTESIAN_POINT('Ctrl Pts',(-38.3259012464104,48.6590644974859,1.73172063147388));
#41589=CARTESIAN_POINT('Ctrl Pts',(-39.,48.8917573484389,1.82394074538817));
#41590=CARTESIAN_POINT('Ctrl Pts',(-39.,48.2236080194775,1.55777972874027));
#41591=CARTESIAN_POINT('Ctrl Pts',(-38.3175153184177,48.6659782242293,1.70656040296349));
#41592=CARTESIAN_POINT('Ctrl Pts',(-39.,48.912387085206,1.81065038969406));
#41593=CARTESIAN_POINT('Ctrl Pts',(-39.,48.2374398092193,1.52423564661872));
#41594=CARTESIAN_POINT('Ctrl Pts',(-38.3011740677622,48.6807575825497,1.6575308483829));
#41595=CARTESIAN_POINT('Ctrl Pts',(-39.,48.9540184168853,1.78795051379182));
#41596=CARTESIAN_POINT('Ctrl Pts',(-39.,48.2670065486315,1.45886912201177));
#41597=CARTESIAN_POINT('Ctrl Pts',(-38.2932187499813,48.6886232026976,1.63366153687808));
#41598=CARTESIAN_POINT('Ctrl Pts',(-39.,48.9750223828953,1.7786505831365));
#41599=CARTESIAN_POINT('Ctrl Pts',(-39.,48.2827414843619,1.4270467103952));
#41600=CARTESIAN_POINT('Ctrl Pts',(-38.2777925604244,48.7052531688598,1.5873754255043));
#41601=CARTESIAN_POINT('Ctrl Pts',(-39.,49.0167801391035,1.76422804457118));
#41602=CARTESIAN_POINT('Ctrl Pts',(-39.,48.3160079917187,1.3653389668037));
#41603=CARTESIAN_POINT('Ctrl Pts',(-38.2703216923166,48.7140175036481,1.56495863655659));
#41604=CARTESIAN_POINT('Ctrl Pts',(-39.,49.0375135780982,1.75922619646151));
#41605=CARTESIAN_POINT('Ctrl Pts',(-39.,48.3335395481203,1.33545366312211));
#41606=CARTESIAN_POINT('Ctrl Pts',(-38.255914958235,48.7323856389745,1.52172935831263));
#41607=CARTESIAN_POINT('Ctrl Pts',(-39.,49.0779804973326,1.75359046880955));
#41608=CARTESIAN_POINT('Ctrl Pts',(-39.,48.370280609407,1.27782246142017));
#41609=CARTESIAN_POINT('Ctrl Pts',(-38.2489790947276,48.741989428833,1.50091687634094));
#41610=CARTESIAN_POINT('Ctrl Pts',(-39.,49.0976661851908,1.75308248268751));
#41611=CARTESIAN_POINT('Ctrl Pts',(-39.,48.3894900980617,1.25007658891254));
#41612=CARTESIAN_POINT('Ctrl Pts',(-38.2356892991005,48.7619715317674,1.46103715437746));
#41613=CARTESIAN_POINT('Ctrl Pts',(-39.,49.1351612200714,1.75646310440614));
#41614=CARTESIAN_POINT('Ctrl Pts',(-39.,48.4294569765608,1.19691209180873));
#41615=CARTESIAN_POINT('Ctrl Pts',(-38.2293353682963,48.7723498350628,1.44196991828834));
#41616=CARTESIAN_POINT('Ctrl Pts',(-39.,49.1528920190527,1.76047367398439));
#41617=CARTESIAN_POINT('Ctrl Pts',(-39.,48.4502143494671,1.17149348979916));
#41618=CARTESIAN_POINT('Ctrl Pts',(-38.2172524228879,48.7938107755338,1.40570983381058));
#41619=CARTESIAN_POINT('Ctrl Pts',(-39.,49.1854965841077,1.77268752052089));
#41620=CARTESIAN_POINT('Ctrl Pts',(-39.,48.4931364697057,1.12315562043586));
#41621=CARTESIAN_POINT('Ctrl Pts',(-38.2115234085426,48.8048934041713,1.38851698622487));
#41622=CARTESIAN_POINT('Ctrl Pts',(-39.,49.2002608324643,1.78099665448271));
#41623=CARTESIAN_POINT('Ctrl Pts',(-39.,48.5153011996989,1.10023637266547));
#41624=CARTESIAN_POINT('Ctrl Pts',(-38.2007290458784,48.8276880282294,1.35612215636338));
#41625=CARTESIAN_POINT('Ctrl Pts',(-39.,49.2259038684558,1.80129243318477));
#41626=CARTESIAN_POINT('Ctrl Pts',(-39.,48.5608879792475,1.05705237794022));
#41627=CARTESIAN_POINT('Ctrl Pts',(-38.195663662783,48.8394001036726,1.34092007054188));
#41628=CARTESIAN_POINT('Ctrl Pts',(-39.0000000000001,49.236644940001,1.81335075777812));
#41629=CARTESIAN_POINT('Ctrl Pts',(-39.,48.5843100738694,1.03678759836947));
#41630=CARTESIAN_POINT('Ctrl Pts',(-38.190947298471,48.851387088898,1.32676510440455));
#41631=CARTESIAN_POINT('Ctrl Pts',(-39.,49.2448593423298,1.82664018134291));
#41632=CARTESIAN_POINT('Ctrl Pts',(-39.,48.6082814197213,1.01791876511632));
#41633=CARTESIAN_POINT('',(-38.5000013347617,48.5946171140508,2.25361874077735));
#41634=CARTESIAN_POINT('',(-39.,48.5946168149163,1.02887446815399));
#41635=CARTESIAN_POINT('Ctrl Pts',(-38.5000036709582,48.5946177418629,2.25361738261186));
#41636=CARTESIAN_POINT('Ctrl Pts',(-38.5088353775067,48.5946177418629,2.23831416931868));
#41637=CARTESIAN_POINT('Ctrl Pts',(-38.5118644338839,48.5946168001396,2.23312624335332));
#41638=CARTESIAN_POINT('Ctrl Pts',(-38.6044346062607,48.5946168001396,2.07241374470279));
#41639=CARTESIAN_POINT('Ctrl Pts',(-38.7257091353047,48.5946168001447,1.86441097587205));
#41640=CARTESIAN_POINT('Ctrl Pts',(-38.8689400035351,48.5946168001447,1.56477839703979));
#41641=CARTESIAN_POINT('Ctrl Pts',(-38.916056425514,48.5946168001447,1.45350707240695));
#41642=CARTESIAN_POINT('Ctrl Pts',(-38.979760764433,48.5946168001447,1.24081758397416));
#41643=CARTESIAN_POINT('Ctrl Pts',(-39.000000003693,48.5946168001447,1.13498028931347));
#41644=CARTESIAN_POINT('Ctrl Pts',(-39.,48.5946168001447,1.02887446815399));
#41645=CARTESIAN_POINT('',(-38.8535533905933,49.0946168001447,3.31427946513778));
#41646=CARTESIAN_POINT('Origin',(-38.4999999999997,49.0946168001451,2.25361929335716));
#41647=CARTESIAN_POINT('',(-39.,49.0946168001447,3.66783285573106));
#41648=CARTESIAN_POINT('Origin',(-38.5,49.0946168001447,3.66783285573106));
#41649=CARTESIAN_POINT('Origin',(-39.,49.0946260151291,2.25361684509152));
#41650=CARTESIAN_POINT('Origin',(-38.5,34.999999994595,3.66783285573106));
#41651=CARTESIAN_POINT('',(-38.8535533905933,51.0871688613417,3.31427946513778));
#41652=CARTESIAN_POINT('',(-38.8535533905933,48.5946168001447,3.31427946513778));
#41653=CARTESIAN_POINT('',(-39.,51.0871688613417,3.66783285573106));
#41654=CARTESIAN_POINT('Origin',(-38.5,51.0871688613417,3.66783285573106));
#41655=CARTESIAN_POINT('',(-39.,34.999999994595,3.66783285573106));
#41656=CARTESIAN_POINT('Ctrl Pts',(-39.0004132136994,51.0650382190915,3.67320198015863));
#41657=CARTESIAN_POINT('Ctrl Pts',(-39.0026470813632,51.0568537778256,3.46336368637365));
#41658=CARTESIAN_POINT('Ctrl Pts',(-38.8543685602191,51.045166200389,3.31509463512307));
#41659=CARTESIAN_POINT('Ctrl Pts',(-38.9993650281416,51.0933835567273,3.66532101541981));
#41660=CARTESIAN_POINT('Ctrl Pts',(-38.9983197911702,51.0954158980446,3.45903672724059));
#41661=CARTESIAN_POINT('Ctrl Pts',(-38.8522723311024,51.0987408007483,3.31299840599475));
#41662=CARTESIAN_POINT('Ctrl Pts',(-39.0003073665066,51.1207747726147,3.6614931211168));
#41663=CARTESIAN_POINT('Ctrl Pts',(-38.9976874728413,51.1334658286751,3.45840463886212));
#41664=CARTESIAN_POINT('Ctrl Pts',(-38.8541571729459,51.1513558166005,3.31488324783015));
#41665=CARTESIAN_POINT('Ctrl Pts',(-39.0054754132473,51.1666975933268,3.66193564327231));
#41666=CARTESIAN_POINT('Ctrl Pts',(-39.0031011742983,51.1978659396949,3.46381856720568));
#41667=CARTESIAN_POINT('Ctrl Pts',(-38.8644936257713,51.2410601515156,3.32521970064757));
#41668=CARTESIAN_POINT('Ctrl Pts',(-39.0087733936485,51.1856684908119,3.66434215081685));
#41669=CARTESIAN_POINT('Ctrl Pts',(-39.0074314446558,51.2247144410629,3.46814888026069));
#41670=CARTESIAN_POINT('Ctrl Pts',(-38.8710897498968,51.2785995319265,3.33181582477153));
#41671=CARTESIAN_POINT('Ctrl Pts',(-39.0143549183491,51.2087029404423,3.6702511952005));
#41672=CARTESIAN_POINT('Ctrl Pts',(-39.0154875060493,51.2574656215126,3.47620492597015));
#41673=CARTESIAN_POINT('Ctrl Pts',(-38.8822530434418,51.3248177772951,3.34297911831711));
#41674=CARTESIAN_POINT('Ctrl Pts',(-39.0155448251913,51.2132751460628,3.67157941317018));
#41675=CARTESIAN_POINT('Ctrl Pts',(-39.0172324883617,51.2639770516779,3.47794990165795));
#41676=CARTESIAN_POINT('Ctrl Pts',(-38.8846329063861,51.3340250290864,3.3453589812617));
#41677=CARTESIAN_POINT('Ctrl Pts',(-39.0180473737812,51.2222620687329,3.67449946007851));
#41678=CARTESIAN_POINT('Ctrl Pts',(-39.0209519414425,51.2767911867937,3.48166933473724));
#41679=CARTESIAN_POINT('Ctrl Pts',(-38.8896381011801,51.3521883956118,3.35036417605639));
#41680=CARTESIAN_POINT('Ctrl Pts',(-39.019362676268,51.2266883046425,3.67609400270875));
#41681=CARTESIAN_POINT('Ctrl Pts',(-39.0229304708662,51.2831109734046,3.48364785077913));
#41682=CARTESIAN_POINT('Ctrl Pts',(-38.8922687593557,51.3611675700846,3.35299483423247));
#41683=CARTESIAN_POINT('Ctrl Pts',(-39.0234967000298,51.2397696792542,3.68127177968089));
#41684=CARTESIAN_POINT('Ctrl Pts',(-39.0292136522808,51.3018106261032,3.48993098214682));
#41685=CARTESIAN_POINT('Ctrl Pts',(-38.9005369597166,51.3878039362001,3.36126303459511));
#41686=CARTESIAN_POINT('Ctrl Pts',(-39.0265033515949,51.248227685921,3.68524877806938));
#41687=CARTESIAN_POINT('Ctrl Pts',(-39.0338657297898,51.3139294225388,3.49458301308925));
#41688=CARTESIAN_POINT('Ctrl Pts',(-38.9065503741551,51.4051602537286,3.36727644903522));
#41689=CARTESIAN_POINT('Ctrl Pts',(-39.0362506360782,51.2728396274532,3.69869584278333));
#41690=CARTESIAN_POINT('Ctrl Pts',(-39.0491554140162,51.3492559657486,3.50987251941062));
#41691=CARTESIAN_POINT('Ctrl Pts',(-38.9260452743275,51.4560647988364,3.38677134921394));
#41692=CARTESIAN_POINT('Ctrl Pts',(-39.0437160920884,51.2882342797459,3.7096765772377));
#41693=CARTESIAN_POINT('Ctrl Pts',(-39.0611272669598,51.3714257050568,3.52184420280592));
#41694=CARTESIAN_POINT('Ctrl Pts',(-38.9409764285494,51.4884526127531,3.40170250344182));
#41695=CARTESIAN_POINT('Ctrl Pts',(-39.0542165012263,51.306253347527,3.72581511285224));
#41696=CARTESIAN_POINT('Ctrl Pts',(-39.0781424378334,51.3973171852378,3.53885910063643));
#41697=CARTESIAN_POINT('Ctrl Pts',(-38.9619775702996,51.5270665421227,3.42270364520152));
#41698=CARTESIAN_POINT('Ctrl Pts',(-39.0563797411747,51.3098026213536,3.72917101376348));
#41699=CARTESIAN_POINT('Ctrl Pts',(-39.0816629307715,51.4024242807893,3.54237953564933));
#41700=CARTESIAN_POINT('Ctrl Pts',(-38.9663041175394,51.5347104471688,3.42703019244338));
#41701=CARTESIAN_POINT('Ctrl Pts',(-39.0607958470836,51.3167363106842,3.73608090526937));
#41702=CARTESIAN_POINT('Ctrl Pts',(-39.0888670320053,51.4123984763779,3.54958351557072));
#41703=CARTESIAN_POINT('Ctrl Pts',(-38.975136458622,51.5497194020163,3.43586253353023));
#41704=CARTESIAN_POINT('Ctrl Pts',(-39.0630486386578,51.3201214581943,3.73963462669351));
#41705=CARTESIAN_POINT('Ctrl Pts',(-39.0925510010862,51.4172668812864,3.55326742126279));
#41706=CARTESIAN_POINT('Ctrl Pts',(-38.9796421118285,51.5570858174706,3.44036818673893));
#41707=CARTESIAN_POINT('Ctrl Pts',(-39.0699366073489,51.3300401544233,3.75058117469492));
#41708=CARTESIAN_POINT('Ctrl Pts',(-39.1038433226588,51.4315326049623,3.56455954462027));
#41709=CARTESIAN_POINT('Ctrl Pts',(-38.9934182473023,51.5787851825119,3.45414432221952));
#41710=CARTESIAN_POINT('Ctrl Pts',(-39.0747012126549,51.3363372494979,3.75825902842783));
#41711=CARTESIAN_POINT('Ctrl Pts',(-39.1116821357186,51.4405754880574,3.57239821496679));
#41712=CARTESIAN_POINT('Ctrl Pts',(-39.0029476009635,51.5927187236375,3.46367367588575));
#41713=CARTESIAN_POINT('Ctrl Pts',(-39.0894825144253,51.3543368021546,3.78236118822114));
#41714=CARTESIAN_POINT('Ctrl Pts',(-39.1360937469245,51.4664061341308,3.5968093671278));
#41715=CARTESIAN_POINT('Ctrl Pts',(-39.0325106179011,51.6330150924322,3.49323669283907));
#41716=CARTESIAN_POINT('Ctrl Pts',(-39.099984848889,51.3651509597073,3.79984981751613));
#41717=CARTESIAN_POINT('Ctrl Pts',(-39.1535206447848,51.4818344395588,3.61423591843403));
#41718=CARTESIAN_POINT('Ctrl Pts',(-39.0535155850355,51.657879312988,3.51424165998539));
#41719=CARTESIAN_POINT('Ctrl Pts',(-39.1166298330874,51.3797350133674,3.82802206864364));
#41720=CARTESIAN_POINT('Ctrl Pts',(-39.1811244902722,51.5024247355477,3.64183918729206));
#41721=CARTESIAN_POINT('Ctrl Pts',(-39.0868060117716,51.6924247339652,3.54753208674103));
#41722=CARTESIAN_POINT('Ctrl Pts',(-39.1223391592955,51.3843292933444,3.83775804229266));
#41723=CARTESIAN_POINT('Ctrl Pts',(-39.1906195944728,51.5088870560383,3.6513340886733));
#41724=CARTESIAN_POINT('Ctrl Pts',(-39.0982248234841,51.7034975154818,3.55895089846032));
#41725=CARTESIAN_POINT('Ctrl Pts',(-39.1339020438763,51.3928845223354,3.85760749410021));
#41726=CARTESIAN_POINT('Ctrl Pts',(-39.2098534044357,51.5208432398919,3.67056747890522));
#41727=CARTESIAN_POINT('Ctrl Pts',(-39.1213509013222,51.7244996054785,3.58207697631249));
#41728=CARTESIAN_POINT('Ctrl Pts',(-39.1397709861723,51.396860516286,3.8677467521508));
#41729=CARTESIAN_POINT('Ctrl Pts',(-39.2196213133971,51.5263568494977,3.68033517032777));
#41730=CARTESIAN_POINT('Ctrl Pts',(-39.1330889487652,51.7344638113003,3.59381502376268));
#41731=CARTESIAN_POINT('Ctrl Pts',(-39.157621772381,51.4079454815182,3.89876073152793));
#41732=CARTESIAN_POINT('Ctrl Pts',(-39.2493801680053,51.5416207945294,3.71009334903438));
#41733=CARTESIAN_POINT('Ctrl Pts',(-39.1687909902807,51.7628597814416,3.62951706530047));
#41734=CARTESIAN_POINT('Ctrl Pts',(-39.1698466131479,51.4142147039408,3.92022917339187));
#41735=CARTESIAN_POINT('Ctrl Pts',(-39.269729837374,51.5500260923023,3.7304425387748));
#41736=CARTESIAN_POINT('Ctrl Pts',(-39.1932410033856,51.7798007004865,3.65396707842107));
#41737=CARTESIAN_POINT('Ctrl Pts',(-39.1948753371907,51.4247405914866,3.96457564423585));
#41738=CARTESIAN_POINT('Ctrl Pts',(-39.3112907465306,51.5636693356107,3.77200243192297));
#41739=CARTESIAN_POINT('Ctrl Pts',(-39.2432991138983,51.8101301358283,3.70402518896648));
#41740=CARTESIAN_POINT('Ctrl Pts',(-39.2076795776735,51.4289960250896,3.98745463026039));
#41741=CARTESIAN_POINT('Ctrl Pts',(-39.3325285954283,51.5688838290406,3.79323974347319));
#41742=CARTESIAN_POINT('Ctrl Pts',(-39.2689079376051,51.8235164183283,3.72963401269037));
#41743=CARTESIAN_POINT('Ctrl Pts',(-39.2240205469469,51.4331410531779,4.01687032803402));
#41744=CARTESIAN_POINT('Ctrl Pts',(-39.3594337885762,51.573511040252,3.82014423116445));
#41745=CARTESIAN_POINT('Ctrl Pts',(-39.3015903184586,51.8381899496214,3.76231639356608));
#41746=CARTESIAN_POINT('Ctrl Pts',(-39.2273055765702,51.433911163606,4.02279445562467));
#41747=CARTESIAN_POINT('Ctrl Pts',(-39.3648581334168,51.5743449115587,3.82556843254212));
#41748=CARTESIAN_POINT('Ctrl Pts',(-39.3081604657371,51.8410213644416,3.76888654084901));
#41749=CARTESIAN_POINT('Ctrl Pts',(-39.2339088376195,51.435335041245,4.03472357381184));
#41750=CARTESIAN_POINT('Ctrl Pts',(-39.375751971054,51.5758253293304,3.83646197951802));
#41751=CARTESIAN_POINT('Ctrl Pts',(-39.3213671634083,51.8464805041875,3.78209323852921));
#41752=CARTESIAN_POINT('Ctrl Pts',(-39.2372263299055,51.4359884597313,4.04072726345858));
#41753=CARTESIAN_POINT('Ctrl Pts',(-39.3812205639743,51.5764709767064,3.84193042525364));
#41754=CARTESIAN_POINT('Ctrl Pts',(-39.3280022373104,51.8491072615919,3.78872831243597));
#41755=CARTESIAN_POINT('Ctrl Pts',(-39.247178880307,51.4377685199949,4.05876895738201));
#41756=CARTESIAN_POINT('Ctrl Pts',(-39.3976316833915,51.5781249620217,3.8583410990863));
#41757=CARTESIAN_POINT('Ctrl Pts',(-39.3479076001771,51.8566508805564,3.8086336753163));
#41758=CARTESIAN_POINT('Ctrl Pts',(-39.2538303336714,51.4387188350674,4.07086701947127));
#41759=CARTESIAN_POINT('Ctrl Pts',(-39.408566396275,51.5788476114369,3.86927550987494));
#41760=CARTESIAN_POINT('Ctrl Pts',(-39.3612106868366,51.8612452314633,3.82193676198504));
#41761=CARTESIAN_POINT('Ctrl Pts',(-39.2738310197503,51.4409006831208,4.10736021368593));
#41762=CARTESIAN_POINT('Ctrl Pts',(-39.4414609831924,51.579951033028,3.90216917193513));
#41763=CARTESIAN_POINT('Ctrl Pts',(-39.4012125847243,51.8738020065102,3.86193865990074));
#41764=CARTESIAN_POINT('Ctrl Pts',(-39.287226430121,51.4414651042384,4.13195370041893));
#41765=CARTESIAN_POINT('Ctrl Pts',(-39.4633483665596,51.5792419677428,3.92405591822746));
#41766=CARTESIAN_POINT('Ctrl Pts',(-39.4280037683589,51.8805418579184,3.88872984355429));
#41767=CARTESIAN_POINT('Ctrl Pts',(-39.3141290116621,51.4409682547149,4.1816268682295));
#41768=CARTESIAN_POINT('Ctrl Pts',(-39.5070603581384,51.575219794606,3.9677665909243));
#41769=CARTESIAN_POINT('Ctrl Pts',(-39.481809658417,51.891062996906,3.94253573365096));
#41770=CARTESIAN_POINT('Ctrl Pts',(-39.3276362284429,51.4399063106198,4.20670677175969));
#41771=CARTESIAN_POINT('Ctrl Pts',(-39.5288968108741,51.5718749448291,3.98960236096735));
#41772=CARTESIAN_POINT('Ctrl Pts',(-39.5088244614836,51.8948429910834,3.9695505367372));
#41773=CARTESIAN_POINT('Ctrl Pts',(-39.354755051824,51.4362532171509,4.25732900698769));
#41774=CARTESIAN_POINT('Ctrl Pts',(-39.5724437164635,51.5627206322971,4.03314785302545));
#41775=CARTESIAN_POINT('Ctrl Pts',(-39.5630628536111,51.8996395002578,4.02378892890451));
#41776=CARTESIAN_POINT('Ctrl Pts',(-39.3683666837519,51.4336617002444,4.28287145663512));
#41777=CARTESIAN_POINT('Ctrl Pts',(-39.5941655928019,51.556877959299,4.05486899752503));
#41778=CARTESIAN_POINT('Ctrl Pts',(-39.5902864954815,51.9006553017652,4.05101257079516));
#41779=CARTESIAN_POINT('Ctrl Pts',(-39.3888590555512,51.428669185987,4.32152453598587));
#41780=CARTESIAN_POINT('Ctrl Pts',(-39.6265016106641,51.5463603767316,4.08720388162891));
#41781=CARTESIAN_POINT('Ctrl Pts',(-39.6312718225881,51.9001955452795,4.09199789793255));
#41782=CARTESIAN_POINT('Ctrl Pts',(-39.3957023535762,51.4268205187815,4.33446556245966));
#41783=CARTESIAN_POINT('Ctrl Pts',(-39.6372928076184,51.5425385825794,4.09799469263457));
#41784=CARTESIAN_POINT('Ctrl Pts',(-39.6449586117414,51.8997111781368,4.10568468709613));
#41785=CARTESIAN_POINT('Ctrl Pts',(-39.4094136202798,51.4227580259902,4.36046079000117));
#41786=CARTESIAN_POINT('Ctrl Pts',(-39.6588203038909,51.5342999415303,4.11952140291209));
#41787=CARTESIAN_POINT('Ctrl Pts',(-39.6723815340093,51.8980893379141,4.13310760938484));
#41788=CARTESIAN_POINT('Ctrl Pts',(-39.4162677663881,51.4205477358223,4.37348889242158));
#41789=CARTESIAN_POINT('Ctrl Pts',(-39.669535476702,51.5298861426874,4.13023617631423));
#41790=CARTESIAN_POINT('Ctrl Pts',(-39.6860900219729,51.8969524844333,4.146816097359));
#41791=CARTESIAN_POINT('Ctrl Pts',(-39.4503663607577,51.4086820482238,4.43846668905814));
#41792=CARTESIAN_POINT('Ctrl Pts',(-39.7231418979962,51.5062754902456,4.18384055660646));
#41793=CARTESIAN_POINT('Ctrl Pts',(-39.7542881428281,51.8897219185405,4.2150142182665));
#41794=CARTESIAN_POINT('Ctrl Pts',(-39.4772582375367,51.3965556312517,4.49023496260712));
#41795=CARTESIAN_POINT('Ctrl Pts',(-39.7642005002811,51.4831753452374,4.22489745473237));
#41796=CARTESIAN_POINT('Ctrl Pts',(-39.8080718615601,51.8790082051072,4.26879793704068));
#41797=CARTESIAN_POINT('Ctrl Pts',(-39.5038019361007,51.3820343130569,4.54185646265653));
#41798=CARTESIAN_POINT('Ctrl Pts',(-39.803134320195,51.4567542175855,4.26382949617694));
#41799=CARTESIAN_POINT('Ctrl Pts',(-39.861160938566,51.8638711179526,4.32188701408911));
#41800=CARTESIAN_POINT('Ctrl Pts',(-39.,51.0871688613417,3.66783285573106));
#41801=CARTESIAN_POINT('Ctrl Pts',(-39.,51.0995964745295,3.66526623270042));
#41802=CARTESIAN_POINT('Ctrl Pts',(-39.0003980980124,51.1120315517898,3.66346660688227));
#41803=CARTESIAN_POINT('Ctrl Pts',(-39.0012397064956,51.1244742900618,3.66251648874842));
#41804=CARTESIAN_POINT('Ctrl Pts',(-39.0017520306939,51.132048733567,3.66193810994057));
#41805=CARTESIAN_POINT('Ctrl Pts',(-39.0024288183487,51.1396258232086,3.66167471989657));
#41806=CARTESIAN_POINT('Ctrl Pts',(-39.0032819045167,51.1472062783665,3.66174775116153));
#41807=CARTESIAN_POINT('Ctrl Pts',(-39.003830205514,51.152078436981,3.66179469028316));
#41808=CARTESIAN_POINT('Ctrl Pts',(-39.0044513162621,51.1569520679716,3.66198055458152));
#41809=CARTESIAN_POINT('Ctrl Pts',(-39.0051494245821,51.1618268948852,3.66231306057799));
#41810=CARTESIAN_POINT('Ctrl Pts',(-39.0055954934587,51.1649417532861,3.66252552126937));
#41811=CARTESIAN_POINT('Ctrl Pts',(-39.006073011082,51.1680571554945,3.66279782153449));
#41812=CARTESIAN_POINT('Ctrl Pts',(-39.0065831559074,51.1711730884579,3.6631321412611));
#41813=CARTESIAN_POINT('Ctrl Pts',(-39.0070933007329,51.1742890214214,3.66346646098771));
#41814=CARTESIAN_POINT('Ctrl Pts',(-39.0076356421744,51.1774019318785,3.6638627061799));
#41815=CARTESIAN_POINT('Ctrl Pts',(-39.0082068784871,51.1804909131394,3.66431876730514));
#41816=CARTESIAN_POINT('Ctrl Pts',(-39.0093493511126,51.186668875661,3.66523088955563));
#41817=CARTESIAN_POINT('Ctrl Pts',(-39.0106111129066,51.1927743436604,3.66638458995328));
#41818=CARTESIAN_POINT('Ctrl Pts',(-39.0119924837342,51.1988072949574,3.66777962771153));
#41819=CARTESIAN_POINT('Ctrl Pts',(-39.0123974891622,51.2005761016917,3.66818864015996));
#41820=CARTESIAN_POINT('Ctrl Pts',(-39.0128129276482,51.2023393171679,3.66861857412582));
#41821=CARTESIAN_POINT('Ctrl Pts',(-39.0132386139189,51.2040960879642,3.66906923077199));
#41822=CARTESIAN_POINT('Ctrl Pts',(-39.0142648355865,51.2083312169324,3.67015564968387));
#41823=CARTESIAN_POINT('Ctrl Pts',(-39.0153512215115,51.2125280987449,3.67136380075719));
#41824=CARTESIAN_POINT('Ctrl Pts',(-39.0164841144222,51.216642004501,3.67267657739539));
#41825=CARTESIAN_POINT('Ctrl Pts',(-39.0165877103608,51.2170181953343,3.67279662257064));
#41826=CARTESIAN_POINT('Ctrl Pts',(-39.0166917083802,51.2173937442946,3.67291755655674));
#41827=CARTESIAN_POINT('Ctrl Pts',(-39.0167961002917,51.2177686258567,3.67303936883383));
#41828=CARTESIAN_POINT('Ctrl Pts',(-39.0180523386729,51.2222799007215,3.67450524157719));
#41829=CARTESIAN_POINT('Ctrl Pts',(-39.0193683093485,51.2267061299586,3.67610105605805));
#41830=CARTESIAN_POINT('Ctrl Pts',(-39.0207406841958,51.2310487629442,3.67781992804404));
#41831=CARTESIAN_POINT('Ctrl Pts',(-39.0210187256343,51.2319285749902,3.67816816937228));
#41832=CARTESIAN_POINT('Ctrl Pts',(-39.0212990800108,51.232804958106,3.67852145716376));
#41833=CARTESIAN_POINT('Ctrl Pts',(-39.0215817215748,51.2336779220825,3.6788797386022));
#41834=CARTESIAN_POINT('Ctrl Pts',(-39.0241236459549,51.2415288849186,3.68210192684084));
#41835=CARTESIAN_POINT('Ctrl Pts',(-39.0268515468469,51.2491069283234,3.68572893466199));
#41836=CARTESIAN_POINT('Ctrl Pts',(-39.0297524567615,51.2564317442274,3.68973091949866));
#41837=CARTESIAN_POINT('Ctrl Pts',(-39.0309454699727,51.2594441101403,3.6913767550888));
#41838=CARTESIAN_POINT('Ctrl Pts',(-39.0321676781911,51.2624137209571,3.6930858697691));
#41839=CARTESIAN_POINT('Ctrl Pts',(-39.0334184549677,51.2653416363956,3.69485679380877));
#41840=CARTESIAN_POINT('Ctrl Pts',(-39.0355645267475,51.2703653279237,3.69789532968244));
#41841=CARTESIAN_POINT('Ctrl Pts',(-39.0377946841974,51.2752663367985,3.70111548255788));
#41842=CARTESIAN_POINT('Ctrl Pts',(-39.0401058114859,51.2800494365045,3.70451004803446));
#41843=CARTESIAN_POINT('Ctrl Pts',(-39.0424169387745,51.2848325362106,3.70790461351104));
#41844=CARTESIAN_POINT('Ctrl Pts',(-39.0448144637063,51.2895066993963,3.71148200120225));
#41845=CARTESIAN_POINT('Ctrl Pts',(-39.0472643549682,51.294022166229,3.71518767696938));
#41846=CARTESIAN_POINT('Ctrl Pts',(-39.0488581606738,51.2969597565267,3.71759844812181));
#41847=CARTESIAN_POINT('Ctrl Pts',(-39.0504759635781,51.2998344601907,3.72006609450073));
#41848=CARTESIAN_POINT('Ctrl Pts',(-39.0521164252352,51.3026495570621,3.72258735743621));
#41849=CARTESIAN_POINT('Ctrl Pts',(-39.0529975712403,51.304161638342,3.72394161082802));
#41850=CARTESIAN_POINT('Ctrl Pts',(-39.053886084437,51.305657685124,3.72531266237347));
#41851=CARTESIAN_POINT('Ctrl Pts',(-39.0547804720049,51.307136108471,3.72669801456886));
#41852=CARTESIAN_POINT('Ctrl Pts',(-39.0560387467964,51.3092160376823,3.72864700604342));
#41853=CARTESIAN_POINT('Ctrl Pts',(-39.0573092698283,51.3112620946395,3.73062532617036));
#41854=CARTESIAN_POINT('Ctrl Pts',(-39.0585878042399,51.3132695017008,3.73262588877138));
#41855=CARTESIAN_POINT('Ctrl Pts',(-39.0599099821681,51.3153454327708,3.73469474174153));
#41856=CARTESIAN_POINT('Ctrl Pts',(-39.0612407201129,51.3173803278842,3.73678731392401));
#41857=CARTESIAN_POINT('Ctrl Pts',(-39.0625790831881,51.3193756616965,3.73890147686224));
#41858=CARTESIAN_POINT('Ctrl Pts',(-39.0634971743549,51.3207444220738,3.74035175172014));
#41859=CARTESIAN_POINT('Ctrl Pts',(-39.0644190730827,51.3220948885419,3.74181255620632));
#41860=CARTESIAN_POINT('Ctrl Pts',(-39.0653446285659,51.3234276913672,3.74328347395578));
#41861=CARTESIAN_POINT('Ctrl Pts',(-39.0697269764318,51.3297382861638,3.75024801943863));
#41862=CARTESIAN_POINT('Ctrl Pts',(-39.0741907292571,51.335653921141,3.75743801365242));
#41863=CARTESIAN_POINT('Ctrl Pts',(-39.0787251755062,51.3412317605606,3.7648214335795));
#41864=CARTESIAN_POINT('Ctrl Pts',(-39.0790259119933,51.3416016976466,3.7653111215478));
#41865=CARTESIAN_POINT('Ctrl Pts',(-39.0793269611165,51.3419701450682,3.76580166465627));
#41866=CARTESIAN_POINT('Ctrl Pts',(-39.0796283193631,51.3423371166535,3.76629305339742));
#41867=CARTESIAN_POINT('Ctrl Pts',(-39.0848304408808,51.3486718720562,3.77477552890059));
#41868=CARTESIAN_POINT('Ctrl Pts',(-39.0901237073089,51.3545686231568,3.78350778594277));
#41869=CARTESIAN_POINT('Ctrl Pts',(-39.095497076649,51.3600855765314,3.79245708285084));
#41870=CARTESIAN_POINT('Ctrl Pts',(-39.1006217790422,51.3653472182263,3.80099222726015));
#41871=CARTESIAN_POINT('Ctrl Pts',(-39.1058203796004,51.3702639537623,3.80972667229477));
#41872=CARTESIAN_POINT('Ctrl Pts',(-39.1110815409305,51.3748737334003,3.81863120842067));
#41873=CARTESIAN_POINT('Ctrl Pts',(-39.1116563965401,51.375377416431,3.81960415378795));
#41874=CARTESIAN_POINT('Ctrl Pts',(-39.1122321348346,51.3758774922222,3.82057937166501));
#41875=CARTESIAN_POINT('Ctrl Pts',(-39.1128086511915,51.376373938695,3.82155667121885));
#41876=CARTESIAN_POINT('Ctrl Pts',(-39.1157350897341,51.3788939367406,3.82651751412991));
#41877=CARTESIAN_POINT('Ctrl Pts',(-39.1186865170056,51.3813245163271,3.8315404301615));
#41878=CARTESIAN_POINT('Ctrl Pts',(-39.1216416073541,51.3836558244275,3.83658791440293));
#41879=CARTESIAN_POINT('Ctrl Pts',(-39.1237991846949,51.385357964443,3.84027319517036));
#41880=CARTESIAN_POINT('Ctrl Pts',(-39.1259597623763,51.3870081589385,3.84397323953785));
#41881=CARTESIAN_POINT('Ctrl Pts',(-39.1281206119593,51.388606926004,3.84768274132748));
#41882=CARTESIAN_POINT('Ctrl Pts',(-39.1289193344976,51.3891978839766,3.8490538977043));
#41883=CARTESIAN_POINT('Ctrl Pts',(-39.129718392079,51.3897821006618,3.85042684643276));
#41884=CARTESIAN_POINT('Ctrl Pts',(-39.130517872912,51.3903597745074,3.85180170705767));
#41885=CARTESIAN_POINT('Ctrl Pts',(-39.1355759629898,51.3940145542418,3.86050006303806));
#41886=CARTESIAN_POINT('Ctrl Pts',(-39.1406441791352,51.3974027997912,3.86926363808882));
#41887=CARTESIAN_POINT('Ctrl Pts',(-39.1457212999534,51.4005555854721,3.87808462932063));
#41888=CARTESIAN_POINT('Ctrl Pts',(-39.1465912344662,51.4010957965826,3.87959605380399));
#41889=CARTESIAN_POINT('Ctrl Pts',(-39.1474614280801,51.4016291023346,3.88110915797035));
#41890=CARTESIAN_POINT('Ctrl Pts',(-39.1483318837667,51.4021556272645,3.88262392648645));
#41891=CARTESIAN_POINT('Ctrl Pts',(-39.1586945751745,51.4084238560221,3.90065710029224));
#41892=CARTESIAN_POINT('Ctrl Pts',(-39.1690947653013,51.4137357364453,3.91892451423044));
#41893=CARTESIAN_POINT('Ctrl Pts',(-39.179525285691,51.4182657071134,3.93738118482275));
#41894=CARTESIAN_POINT('Ctrl Pts',(-39.1804702750404,51.4186761155949,3.93905333122413));
#41895=CARTESIAN_POINT('Ctrl Pts',(-39.1814155213493,51.4190800785542,3.9407270510575));
#41896=CARTESIAN_POINT('Ctrl Pts',(-39.1823610239388,51.4194777096985,3.9424023224895));
#41897=CARTESIAN_POINT('Ctrl Pts',(-39.1829649779349,51.4197317025709,3.94347242730691));
#41898=CARTESIAN_POINT('Ctrl Pts',(-39.1835690373468,51.4199831090079,3.944543167478));
#41899=CARTESIAN_POINT('Ctrl Pts',(-39.184173203649,51.4202319529509,3.94561454164697));
#41900=CARTESIAN_POINT('Ctrl Pts',(-39.1961630588975,51.4251703330717,3.96687627232667));
#41901=CARTESIAN_POINT('Ctrl Pts',(-39.2081930739204,51.4291022904702,3.98838303756631));
#41902=CARTESIAN_POINT('Ctrl Pts',(-39.2202572512408,51.4321859850981,4.01009600071619));
#41903=CARTESIAN_POINT('Ctrl Pts',(-39.2204222834166,51.4322281685657,4.01039302366748));
#41904=CARTESIAN_POINT('Ctrl Pts',(-39.2205873201454,51.4322701922361,4.01069008198365));
#41905=CARTESIAN_POINT('Ctrl Pts',(-39.2207523616119,51.4323120565271,4.01098717593383));
#41906=CARTESIAN_POINT('Ctrl Pts',(-39.2240348618836,51.4331446930114,4.01689606048839));
#41907=CARTESIAN_POINT('Ctrl Pts',(-39.2273192800592,51.4339141314245,4.02281915981079));
#41908=CARTESIAN_POINT('Ctrl Pts',(-39.2306072248842,51.4346231203129,4.02875898953522));
#41909=CARTESIAN_POINT('Ctrl Pts',(-39.2331963988375,51.435181431252,4.03343645622905));
#41910=CARTESIAN_POINT('Ctrl Pts',(-39.2357872865129,51.4357020312782,4.03812346513848));
#41911=CARTESIAN_POINT('Ctrl Pts',(-39.2383733317665,51.4361850310234,4.04280792575837));
#41912=CARTESIAN_POINT('Ctrl Pts',(-39.239097131351,51.4363202162118,4.04411904382396));
#41913=CARTESIAN_POINT('Ctrl Pts',(-39.2398206954841,51.4364524822294,4.04543022127291));
#41914=CARTESIAN_POINT('Ctrl Pts',(-39.2405438557811,51.436581821874,4.04674114905286));
#41915=CARTESIAN_POINT('Ctrl Pts',(-39.2458504974744,51.4375309325395,4.0563609028517));
#41916=CARTESIAN_POINT('Ctrl Pts',(-39.251145838485,51.4383249425886,4.06598604764607));
#41917=CARTESIAN_POINT('Ctrl Pts',(-39.2564276221927,51.4389741257984,4.07561075929201));
#41918=CARTESIAN_POINT('Ctrl Pts',(-39.2577849792638,51.4391409583438,4.07808419840524));
#41919=CARTESIAN_POINT('Ctrl Pts',(-39.2591415164243,51.4392982345284,4.08055774959127));
#41920=CARTESIAN_POINT('Ctrl Pts',(-39.260497242635,51.439446129712,4.08303140018469));
#41921=CARTESIAN_POINT('Ctrl Pts',(-39.2711302077067,51.4406060721175,4.10243224981992));
#41922=CARTESIAN_POINT('Ctrl Pts',(-39.2817131423343,51.4411909085124,4.1218386024189));
#41923=CARTESIAN_POINT('Ctrl Pts',(-39.2922518059041,51.4412652877384,4.14125077550199));
#41924=CARTESIAN_POINT('Ctrl Pts',(-39.2950635958798,51.4412851326419,4.14643008057427));
#41925=CARTESIAN_POINT('Ctrl Pts',(-39.2978722688055,51.4412685850813,4.15160990753937));
#41926=CARTESIAN_POINT('Ctrl Pts',(-39.3006778532916,51.4412167771412,4.15679013282812));
#41927=CARTESIAN_POINT('Ctrl Pts',(-39.3142541806936,51.4409660765973,4.18185743516235));
#41928=CARTESIAN_POINT('Ctrl Pts',(-39.3277581609359,51.4398899778444,4.20693402949082));
#41929=CARTESIAN_POINT('Ctrl Pts',(-39.3411957010275,51.4380798014802,4.23201782515537));
#41930=CARTESIAN_POINT('Ctrl Pts',(-39.3484511372291,51.4371024187871,4.24556151528739));
#41931=CARTESIAN_POINT('Ctrl Pts',(-39.3556872284612,51.4359106986094,4.25910740126514));
#41932=CARTESIAN_POINT('Ctrl Pts',(-39.3629052291215,51.4345145275482,4.272656587124));
#41933=CARTESIAN_POINT('Ctrl Pts',(-39.3692939295653,51.4332787672458,4.28464906174185));
#41934=CARTESIAN_POINT('Ctrl Pts',(-39.3756681854211,51.4318828504596,4.296643680088));
#41935=CARTESIAN_POINT('Ctrl Pts',(-39.3820282651167,51.4303333574907,4.30864017603793));
#41936=CARTESIAN_POINT('Ctrl Pts',(-39.3872902770699,51.4290513844788,4.31856547699404));
#41937=CARTESIAN_POINT('Ctrl Pts',(-39.3925425978744,51.42766410719,4.32849212439794));
#41938=CARTESIAN_POINT('Ctrl Pts',(-39.3977854414924,51.4261743730365,4.33842025616291));
#41939=CARTESIAN_POINT('Ctrl Pts',(-39.3993770212168,51.4257221316869,4.3414341574672));
#41940=CARTESIAN_POINT('Ctrl Pts',(-39.4009677741981,51.4252604370354,4.3444482776708));
#41941=CARTESIAN_POINT('Ctrl Pts',(-39.4025579934351,51.4247892753985,4.34746316990157));
#41942=CARTESIAN_POINT('Ctrl Pts',(-39.4067527024737,51.4235464367187,4.35541590710714));
#41943=CARTESIAN_POINT('Ctrl Pts',(-39.4109385157346,51.4222391034398,4.36336422205488));
#41944=CARTESIAN_POINT('Ctrl Pts',(-39.4151134316595,51.4208697596477,4.37130418161823));
#41945=CARTESIAN_POINT('Ctrl Pts',(-39.4177756300927,51.4199965768188,4.37636721720734));
#41946=CARTESIAN_POINT('Ctrl Pts',(-39.420434351826,51.4190978481754,4.38142864884858));
#41947=CARTESIAN_POINT('Ctrl Pts',(-39.4230874920304,51.4181746011217,4.38648444527947));
#41948=CARTESIAN_POINT('Ctrl Pts',(-39.4261723928398,51.4171011088206,4.39236300023734));
#41949=CARTESIAN_POINT('Ctrl Pts',(-39.4292518432436,51.4159941061449,4.39823785994851));
#41950=CARTESIAN_POINT('Ctrl Pts',(-39.4323256432954,51.4148540747936,4.40410862153796));
#41951=CARTESIAN_POINT('Ctrl Pts',(-39.4551952159076,51.4063720560127,4.44778804316367));
#41952=CARTESIAN_POINT('Ctrl Pts',(-39.4777471479169,51.3960634027247,4.49123179831034));
#41953=CARTESIAN_POINT('Ctrl Pts',(-39.500000018719,51.3840965499153,4.53446621502614));
#41954=CARTESIAN_POINT('Origin',(-39.8162486064498,50.8770797377211,4.27697468104505));
#41955=CARTESIAN_POINT('Origin',(-36.5,48.5946168001447,0.960726074544506));
#41956=CARTESIAN_POINT('',(-36.5,49.0946168001447,0.960726074544506));
#41957=CARTESIAN_POINT('',(-36.5,49.0946168001447,0.960726074544506));
#41958=CARTESIAN_POINT('',(-36.5,48.5946168001447,0.960726074544506));
#41959=CARTESIAN_POINT('Origin',(-29.,48.5946168001447,-3.5392739254555));
#41960=CARTESIAN_POINT('',(-36.7071067811865,48.5946168001447,0.460726074544506));
#41961=CARTESIAN_POINT('',(-30.8535533905933,48.5946168001447,-5.39282731604877));
#41962=CARTESIAN_POINT('',(-39.,48.5946168001447,-3.5392739254555));
#41963=CARTESIAN_POINT('',(-33.5,48.5946168001447,-3.5392739254555));
#41964=CARTESIAN_POINT('',(-29.,48.5946168001447,-3.5392739254555));
#41965=CARTESIAN_POINT('',(-33.5,48.5946168001447,0.960726074544506));
#41966=CARTESIAN_POINT('',(-29.,48.5946168001447,0.460726074544506));
#41967=CARTESIAN_POINT('Origin',(-34.5,21.2255401693197,-2.54750793782168));
#41968=CARTESIAN_POINT('',(-38.5,21.2255401693197,4.45249206217833));
#41969=CARTESIAN_POINT('Origin',(-38.5,39.9592920728172,13.6255430020507));
#41970=CARTESIAN_POINT('',(-39.,42.2751240270462,11.7184713306729));
#41971=CARTESIAN_POINT('Ctrl Pts',(-38.5,42.0900494371385,12.3179218587563));
#41972=CARTESIAN_POINT('Ctrl Pts',(-38.5068454246389,42.0900494371385,12.3179218587563));
#41973=CARTESIAN_POINT('Ctrl Pts',(-38.5137049378611,42.0901092205902,12.3177505069324));
#41974=CARTESIAN_POINT('Ctrl Pts',(-38.574487053383,42.0911734302424,12.3146992394163));
#41975=CARTESIAN_POINT('Ctrl Pts',(-38.6266179130002,42.0958133615388,12.3014448852174));
#41976=CARTESIAN_POINT('Ctrl Pts',(-38.7343668418878,42.1126444683801,12.2523913323773));
#41977=CARTESIAN_POINT('Ctrl Pts',(-38.7864380337499,42.1258891023781,12.2133094615048));
#41978=CARTESIAN_POINT('Ctrl Pts',(-38.885076407075,42.1601839674529,12.1084861762414));
#41979=CARTESIAN_POINT('Ctrl Pts',(-38.9288507671719,42.1829880422529,12.0365453528697));
#41980=CARTESIAN_POINT('Ctrl Pts',(-38.9855092027927,42.2295139139639,11.8814589266464));
#41981=CARTESIAN_POINT('Ctrl Pts',(-38.9995659056513,42.2523337408292,11.8018633471128));
#41982=CARTESIAN_POINT('Ctrl Pts',(-38.9999967004912,42.2744474855277,11.7209494981299));
#41983=CARTESIAN_POINT('Ctrl Pts',(-39.,42.2747858712613,11.719710445334));
#41984=CARTESIAN_POINT('Ctrl Pts',(-39.,42.2751240270462,11.7184713306729));
#41985=CARTESIAN_POINT('',(-39.,37.0086337430747,14.1674059193286));
#41986=CARTESIAN_POINT('Ctrl Pts',(-39.,37.0086337430746,14.1674059193286));
#41987=CARTESIAN_POINT('Ctrl Pts',(-39.,37.0677771080364,14.1458794949282));
#41988=CARTESIAN_POINT('Ctrl Pts',(-38.9854014653638,37.1374107416916,14.1205349249739));
#41989=CARTESIAN_POINT('Ctrl Pts',(-38.9377610024774,37.2465671473057,14.0808052424509));
#41990=CARTESIAN_POINT('Ctrl Pts',(-38.8963920732344,37.3055052224255,14.0593535374423));
#41991=CARTESIAN_POINT('Ctrl Pts',(-38.8087985454361,37.3887709311951,14.0290472979151));
#41992=CARTESIAN_POINT('Ctrl Pts',(-38.747240880002,37.428004125326,14.0147675830563));
#41993=CARTESIAN_POINT('Ctrl Pts',(-38.6335018474161,37.4728113710041,13.99845907935));
#41994=CARTESIAN_POINT('Ctrl Pts',(-38.5613457566216,37.4865145651702,13.9934715245592));
#41995=CARTESIAN_POINT('Ctrl Pts',(-38.5,37.4865145651702,13.9934715245592));
#41996=CARTESIAN_POINT('Origin',(-39.,39.9592920728172,13.6255430020507));
#41997=CARTESIAN_POINT('Origin',(-29.,38.5965482096145,9.88143500940095));
#41998=CARTESIAN_POINT('',(-29.,39.4462618578287,12.2160040708718));
#41999=CARTESIAN_POINT('Origin',(-30.,39.4462618578287,12.2160040708718));
#42000=CARTESIAN_POINT('',(-29.,40.4723222878057,15.0350819332295));
#42001=CARTESIAN_POINT('',(-29.,38.5965482096145,9.88143500940095));
#42002=CARTESIAN_POINT('Origin',(-30.,40.4723222878057,15.0350819332295));
#42003=CARTESIAN_POINT('',(-34.,38.5965482096145,9.88143500940095));
#42004=CARTESIAN_POINT('Origin',(-42.5,40.13030214448,14.0953893124436));
#42005=CARTESIAN_POINT('',(-38.5,42.4320695804642,13.2576144795422));
#42006=CARTESIAN_POINT('Origin',(-42.5,39.7882820011544,13.1556966916577));
#42007=CARTESIAN_POINT('',(-38.5,39.7882820011544,13.1556966916577));
#42008=CARTESIAN_POINT('Origin',(-42.5,40.13030214448,14.0953893124436));
#42009=CARTESIAN_POINT('',(-38.5,36.192066340255,15.5287899207029));
#42010=CARTESIAN_POINT('',(-38.5,35.4318390405505,15.805490029072));
#42011=CARTESIAN_POINT('',(-34.22360679775,38.2013139081217,14.7974836127277));
#42012=CARTESIAN_POINT('Origin',(-38.5,39.9592920728172,13.6255430020507));
#42013=CARTESIAN_POINT('',(-39.,38.3487778137292,16.1565988728829));
#42014=CARTESIAN_POINT('Origin',(-38.5,38.3487778137292,16.1565988728829));
#42015=CARTESIAN_POINT('',(-39.,37.6434601185882,15.5326146734285));
#42016=CARTESIAN_POINT('Origin',(-39.,39.9592920728172,13.6255430020507));
#42017=CARTESIAN_POINT('Ctrl Pts',(-38.5,37.8285347084959,14.9331641453451));
#42018=CARTESIAN_POINT('Ctrl Pts',(-38.5068454246389,37.8285347084959,14.9331641453451));
#42019=CARTESIAN_POINT('Ctrl Pts',(-38.5137049378611,37.8284749250441,14.933335497169));
#42020=CARTESIAN_POINT('Ctrl Pts',(-38.574487053383,37.827410715392,14.9363867646851));
#42021=CARTESIAN_POINT('Ctrl Pts',(-38.6266179130002,37.8227707840955,14.949641118884));
#42022=CARTESIAN_POINT('Ctrl Pts',(-38.7343668418877,37.8059396772543,14.9986946717241));
#42023=CARTESIAN_POINT('Ctrl Pts',(-38.7864380337499,37.7926950432563,15.0377765425966));
#42024=CARTESIAN_POINT('Ctrl Pts',(-38.885076407075,37.7584001781814,15.1425998278601));
#42025=CARTESIAN_POINT('Ctrl Pts',(-38.9288507671719,37.7355961033814,15.2145406512318));
#42026=CARTESIAN_POINT('Ctrl Pts',(-38.9855092027929,37.6890702316704,15.3696270774554));
#42027=CARTESIAN_POINT('Ctrl Pts',(-38.9995659056513,37.6662504048046,15.4492226569908));
#42028=CARTESIAN_POINT('Ctrl Pts',(-38.9999967004912,37.6441366601067,15.5301365059714));
#42029=CARTESIAN_POINT('Ctrl Pts',(-39.,37.643798274373,15.5313755587675));
#42030=CARTESIAN_POINT('Ctrl Pts',(-39.,37.6434601185882,15.5326146734285));
#42031=CARTESIAN_POINT('Origin',(-38.5,40.3013122161429,14.5652356228366));
#42032=CARTESIAN_POINT('',(-39.,36.3630764119178,15.9986362310959));
#42033=CARTESIAN_POINT('',(-39.,37.9995447801587,15.4030104557381));
#42034=CARTESIAN_POINT('Origin',(-38.5,36.3630764119178,15.9986362310959));
#42035=CARTESIAN_POINT('Ctrl Pts',(-38.499976268987,36.1920824132574,15.528784071));
#42036=CARTESIAN_POINT('Ctrl Pts',(-39.0000141579952,36.1920742957822,15.5287617695291));
#42037=CARTESIAN_POINT('Ctrl Pts',(-38.9999999997996,36.3631080422587,15.9986397839424));
#42038=CARTESIAN_POINT('Ctrl Pts',(-38.5097935987872,36.1644071656834,15.5388572571144));
#42039=CARTESIAN_POINT('Ctrl Pts',(-39.0000137450654,36.1679944730221,15.5478735083829));
#42040=CARTESIAN_POINT('Ctrl Pts',(-38.9999999998035,36.3169823289421,16.0154292157321));
#42041=CARTESIAN_POINT('Ctrl Pts',(-38.5196108634531,36.1362370290697,15.5475699381323));
#42042=CARTESIAN_POINT('Ctrl Pts',(-39.0000133419967,36.1419138371004,15.5656989246035));
#42043=CARTESIAN_POINT('Ctrl Pts',(-38.9999999998075,36.2698666781457,16.0294976363005));
#42044=CARTESIAN_POINT('Ctrl Pts',(-38.5390736407832,36.0793995346958,15.5621222878223));
#42045=CARTESIAN_POINT('Ctrl Pts',(-39.0000125682431,36.0869060952579,15.5975660971732));
#42046=CARTESIAN_POINT('Ctrl Pts',(-38.9999999998153,36.1744793668348,16.0519471037778));
#42047=CARTESIAN_POINT('Ctrl Pts',(-38.5487190733747,36.0507326010709,15.5679624197071));
#42048=CARTESIAN_POINT('Ctrl Pts',(-39.0000121966607,36.0580101419523,15.6116879967721));
#42049=CARTESIAN_POINT('Ctrl Pts',(-38.9999999998191,36.1262084792976,16.0603291053491));
#42050=CARTESIAN_POINT('Ctrl Pts',(-38.5676730659644,35.9933927191952,15.5766710046091));
#42051=CARTESIAN_POINT('Ctrl Pts',(-39.0000114876801,35.9982390714978,15.6356400264069));
#42052=CARTESIAN_POINT('Ctrl Pts',(-38.9999999998267,36.0293379704017,16.0712648402057));
#42053=CARTESIAN_POINT('Ctrl Pts',(-38.5769815381232,35.9647200359621,15.5795394154795));
#42054=CARTESIAN_POINT('Ctrl Pts',(-39.0000111493512,35.967367881521,15.6455528228801));
#42055=CARTESIAN_POINT('Ctrl Pts',(-38.9999999998304,35.9807387962325,16.0738185200393));
#42056=CARTESIAN_POINT('Ctrl Pts',(-38.5951004176242,35.9078651416925,15.5822548730069));
#42057=CARTESIAN_POINT('Ctrl Pts',(-39.0000105080838,35.9045586256948,15.6607504618682));
#42058=CARTESIAN_POINT('Ctrl Pts',(-38.9999999998377,35.8840532497444,16.0730533413708));
#42059=CARTESIAN_POINT('Ctrl Pts',(-38.6039107409546,35.8796831935688,15.5821019053127));
#42060=CARTESIAN_POINT('Ctrl Pts',(-39.0000102042262,35.8726008933071,15.6661139213138));
#42061=CARTESIAN_POINT('Ctrl Pts',(-38.9999999998412,35.8359673238182,16.0697344836139));
#42062=CARTESIAN_POINT('Ctrl Pts',(-38.6208807544625,35.8242977617097,15.5787772351315));
#42063=CARTESIAN_POINT('Ctrl Pts',(-39.0000096326357,35.8085383701626,15.672043607951));
#42064=CARTESIAN_POINT('Ctrl Pts',(-38.999999999848,35.7411409298723,16.0572816469404));
#42065=CARTESIAN_POINT('Ctrl Pts',(-38.6290403659709,35.7970945340313,15.5756055463191));
#42066=CARTESIAN_POINT('Ctrl Pts',(-39.0000093640297,35.7763944628456,15.6726787655436));
#42067=CARTESIAN_POINT('Ctrl Pts',(-38.9999999998513,35.6944008994066,16.0481477228676));
#42068=CARTESIAN_POINT('Ctrl Pts',(-38.6445676535155,35.7441375911989,15.5662983324471));
#42069=CARTESIAN_POINT('Ctrl Pts',(-39.0000088633528,35.7128591951203,15.6691379903098));
#42070=CARTESIAN_POINT('Ctrl Pts',(-38.9999999998575,35.6030756547977,16.0242228639181));
#42071=CARTESIAN_POINT('Ctrl Pts',(-38.6519352576302,35.7183841206501,15.5601628487775));
#42072=CARTESIAN_POINT('Ctrl Pts',(-39.0000086304804,35.6814143002466,15.6650171583177));
#42073=CARTESIAN_POINT('Ctrl Pts',(-38.9999999998605,35.5584908615417,16.0094320368528));
#42074=CARTESIAN_POINT('Ctrl Pts',(-38.6657509411343,35.6687726400952,15.5450342622458));
#42075=CARTESIAN_POINT('Ctrl Pts',(-39.0000082014641,35.6201335587595,15.6520932108391));
#42076=CARTESIAN_POINT('Ctrl Pts',(-38.999999999866,35.4722481374437,15.9744494378102));
#42077=CARTESIAN_POINT('Ctrl Pts',(-38.6721989566158,35.6449148589008,15.5360412276563));
#42078=CARTESIAN_POINT('Ctrl Pts',(-39.000008004609,35.5902352214897,15.6433287035253));
#42079=CARTESIAN_POINT('Ctrl Pts',(-38.9999999998686,35.4305906033754,15.9542578244946));
#42080=CARTESIAN_POINT('Ctrl Pts',(-38.6840637962516,35.5995078834839,15.5153532356979));
#42081=CARTESIAN_POINT('Ctrl Pts',(-39.0000076476799,35.5328419212708,15.6213754182932));
#42082=CARTESIAN_POINT('Ctrl Pts',(-38.9999999998734,35.3509237627701,15.9088232405161));
#42083=CARTESIAN_POINT('Ctrl Pts',(-38.6894805656146,35.5779588982795,15.5036583721644));
#42084=CARTESIAN_POINT('Ctrl Pts',(-39.0000074869986,35.5052810328468,15.6082074902829));
#42085=CARTESIAN_POINT('Ctrl Pts',(-38.9999999998755,35.3129148219788,15.8835804763394));
#42086=CARTESIAN_POINT('Ctrl Pts',(-38.6991891029095,35.5375426665068,15.4777692022388));
#42087=CARTESIAN_POINT('Ctrl Pts',(-39.0000072023815,35.453278780813,15.5778206579272));
#42088=CARTESIAN_POINT('Ctrl Pts',(-38.9999999998794,35.2412033609684,15.8284806465574));
#42089=CARTESIAN_POINT('Ctrl Pts',(-38.7034808260903,35.5186756055761,15.4635750134849));
#42090=CARTESIAN_POINT('Ctrl Pts',(-39.000007077952,35.4287733420543,15.5606048558306));
#42091=CARTESIAN_POINT('Ctrl Pts',(-38.9999999998812,35.2075011692091,15.7986238314282));
#42092=CARTESIAN_POINT('Ctrl Pts',(-38.7108649420266,35.4839499382353,15.4329329506642));
#42093=CARTESIAN_POINT('Ctrl Pts',(-39.0000068657516,35.3835065226858,15.5225965334714));
#42094=CARTESIAN_POINT('Ctrl Pts',(-38.9999999998841,35.1449868299947,15.734812856048));
#42095=CARTESIAN_POINT('Ctrl Pts',(-38.7139573008052,35.4680914909596,15.4164852158956));
#42096=CARTESIAN_POINT('Ctrl Pts',(-39.0000067776074,35.3626877297703,15.5017905115115));
#42097=CARTESIAN_POINT('Ctrl Pts',(-38.9999999998854,35.1161749682031,15.7008589857377));
#42098=CARTESIAN_POINT('Ctrl Pts',(-38.7188891272861,35.4396576740633,15.3816208410028));
#42099=CARTESIAN_POINT('Ctrl Pts',(-39.000006637863,35.3253159030815,15.4571622621386));
#42100=CARTESIAN_POINT('Ctrl Pts',(-38.9999999998873,35.0639402373661,15.629441805129));
#42101=CARTESIAN_POINT('Ctrl Pts',(-38.7207285723286,35.4270824344453,15.3632043593695));
#42102=CARTESIAN_POINT('Ctrl Pts',(-39.0000065860148,35.3087162707208,15.4333120500278));
#42103=CARTESIAN_POINT('Ctrl Pts',(-38.9999999998881,35.0405176064801,15.5919788191372));
#42104=CARTESIAN_POINT('Ctrl Pts',(-38.7231227065882,35.405432808278,15.3247213622512));
#42105=CARTESIAN_POINT('Ctrl Pts',(-39.0000065187358,35.2801924397798,15.3832270666568));
#42106=CARTESIAN_POINT('Ctrl Pts',(-38.999999999889,34.9994669708968,15.5141920809946));
#42107=CARTESIAN_POINT('Ctrl Pts',(-38.7236773848157,35.3963585204766,15.3046550217128));
#42108=CARTESIAN_POINT('Ctrl Pts',(-39.0000065031849,35.2682357947743,15.3569527614816));
#42109=CARTESIAN_POINT('Ctrl Pts',(-38.9999999998892,34.9818391529727,15.47386868195));
#42110=CARTESIAN_POINT('Ctrl Pts',(-38.7234923684179,35.3818679549979,15.2632197487042));
#42111=CARTESIAN_POINT('Ctrl Pts',(-39.0000065083713,35.2492882925041,15.302706822063));
#42112=CARTESIAN_POINT('Ctrl Pts',(-38.9999999998892,34.9526834379338,15.3910593278306));
#42113=CARTESIAN_POINT('Ctrl Pts',(-38.7227526746417,35.376451743197,15.2418510046719));
#42114=CARTESIAN_POINT('Ctrl Pts',(-39.0000065291178,35.2422815479729,15.2746876798518));
#42115=CARTESIAN_POINT('Ctrl Pts',(-38.9999999998889,34.9411556731551,15.3485737487106));
#42116=CARTESIAN_POINT('Ctrl Pts',(-38.7199917114554,35.3693711473898,15.1981809212197));
#42117=CARTESIAN_POINT('Ctrl Pts',(-39.0000066067696,35.2333994155145,15.2176788928919));
#42118=CARTESIAN_POINT('Ctrl Pts',(-38.9999999998878,34.9243997338898,15.2621756907445));
#42119=CARTESIAN_POINT('Ctrl Pts',(-38.71797045472,35.3677067952793,15.1758797805686));
#42120=CARTESIAN_POINT('Ctrl Pts',(-39.0000066638135,35.2315260836188,15.1886378039953));
#42121=CARTESIAN_POINT('Ctrl Pts',(-38.999999999887,34.9191716350856,15.2182636044247));
#42122=CARTESIAN_POINT('Ctrl Pts',(-38.7126813554341,35.3681587728171,15.1307310487624));
#42123=CARTESIAN_POINT('Ctrl Pts',(-39.0000068139304,35.2329478863815,15.1303351175404));
#42124=CARTESIAN_POINT('Ctrl Pts',(-38.9999999998848,34.9151056148188,15.1297728960607));
#42125=CARTESIAN_POINT('Ctrl Pts',(-38.7094135371893,35.3702750997888,15.1078836633738));
#42126=CARTESIAN_POINT('Ctrl Pts',(-39.0000069072694,35.236263315592,15.1010224532041));
#42127=CARTESIAN_POINT('Ctrl Pts',(-38.9999999998835,34.9162677110207,15.0851946765572));
#42128=CARTESIAN_POINT('Ctrl Pts',(-38.7016878913306,35.3782518262364,15.0620380494563));
#42129=CARTESIAN_POINT('Ctrl Pts',(-39.0000071298392,35.2479693887033,15.0429328957708));
#42130=CARTESIAN_POINT('Ctrl Pts',(-38.9999999998804,34.9249620169377,14.9961436072836));
#42131=CARTESIAN_POINT('Ctrl Pts',(-38.6972300992734,35.3841121884087,15.0390400302111));
#42132=CARTESIAN_POINT('Ctrl Pts',(-39.0000072594605,35.2563977307434,15.014109705271));
#42133=CARTESIAN_POINT('Ctrl Pts',(-38.9999999998786,34.9324941858258,14.9516711632801));
#42134=CARTESIAN_POINT('Ctrl Pts',(-38.6872016890651,35.3994755467077,14.9932913687407));
#42135=CARTESIAN_POINT('Ctrl Pts',(-39.000007554437,35.2781058833073,14.9577442969424));
#42136=CARTESIAN_POINT('Ctrl Pts',(-38.9999999998746,34.9537982699429,14.8636017258914));
#42137=CARTESIAN_POINT('Ctrl Pts',(-38.6816311171518,35.4089784714142,14.9705409357234));
#42138=CARTESIAN_POINT('Ctrl Pts',(-39.0000077203025,35.2914388153182,14.930164811733));
#42139=CARTESIAN_POINT('Ctrl Pts',(-38.9999999998724,34.9675700863202,14.8200051345488));
#42140=CARTESIAN_POINT('Ctrl Pts',(-38.6694736006842,35.4314624433087,14.9256813847395));
#42141=CARTESIAN_POINT('Ctrl Pts',(-39.0000080875677,35.322603574829,14.8770030217846));
#42142=CARTESIAN_POINT('Ctrl Pts',(-38.9999999998675,35.0011150523726,14.734442324397));
#42143=CARTESIAN_POINT('Ctrl Pts',(-38.6628867122873,35.4444433860599,14.9035724722508));
#42144=CARTESIAN_POINT('Ctrl Pts',(-39.0000082895903,35.3405008359967,14.8513963837194));
#42145=CARTESIAN_POINT('Ctrl Pts',(-38.9999999998649,35.0208880466275,14.6924764968968));
#42146=CARTESIAN_POINT('Ctrl Pts',(-38.6488106161275,35.4736586580552,14.8603787974157));
#42147=CARTESIAN_POINT('Ctrl Pts',(-39.0000087288964,35.3803164068158,14.802848917274));
#42148=CARTESIAN_POINT('Ctrl Pts',(-38.9999999998592,35.0660930378355,14.6109019054829));
#42149=CARTESIAN_POINT('Ctrl Pts',(-38.6413214734913,35.489892851549,14.8392942331689));
#42150=CARTESIAN_POINT('Ctrl Pts',(-39.0000089669049,35.402308270487,14.7798999933156));
#42151=CARTESIAN_POINT('Ctrl Pts',(-38.9999999998562,35.0915248252762,14.5712935152036));
#42152=CARTESIAN_POINT('Ctrl Pts',(-38.6255705468163,35.5253335556531,14.7985143583617));
#42153=CARTESIAN_POINT('Ctrl Pts',(-39.0000094777876,35.4497155470534,14.7372695705394));
#42154=CARTESIAN_POINT('Ctrl Pts',(-38.9999999998499,35.1476070823755,14.4951196753651));
#42155=CARTESIAN_POINT('Ctrl Pts',(-38.6173088357458,35.5445399014998,14.778819234957));
#42156=CARTESIAN_POINT('Ctrl Pts',(-39.0000097514748,35.4752074583967,14.7175986525734));
#42157=CARTESIAN_POINT('Ctrl Pts',(-38.9999999998466,35.1782572919257,14.4585545750434));
#42158=CARTESIAN_POINT('Ctrl Pts',(-38.6001558291468,35.5855923740298,14.7411592921823));
#42159=CARTESIAN_POINT('Ctrl Pts',(-39.0000103331288,35.5289057182098,14.6820383202293));
#42160=CARTESIAN_POINT('Ctrl Pts',(-38.9999999998397,35.2442457072874,14.3891005019824));
#42161=CARTESIAN_POINT('Ctrl Pts',(-38.591264613141,35.607438309806,14.7231946456245));
#42162=CARTESIAN_POINT('Ctrl Pts',(-39.0000106419771,35.5571855083951,14.6661794507694));
#42163=CARTESIAN_POINT('Ctrl Pts',(-38.9999999998362,35.2795836068755,14.3562118477394));
#42164=CARTESIAN_POINT('Ctrl Pts',(-38.5730065552073,35.653391716595,14.6893067484556));
#42165=CARTESIAN_POINT('Ctrl Pts',(-39.000011293078,35.6156498660526,14.6386478824867));
#42166=CARTESIAN_POINT('Ctrl Pts',(-38.9999999998289,35.354335539997,14.2946801994281));
#42167=CARTESIAN_POINT('Ctrl Pts',(-38.5636397979342,35.6774989739494,14.6733836531619));
#42168=CARTESIAN_POINT('Ctrl Pts',(-39.0000116362538,35.6458982364807,14.6270255264977));
#42169=CARTESIAN_POINT('Ctrl Pts',(-38.9999999998251,35.3937492265869,14.2660374873015));
#42170=CARTESIAN_POINT('Ctrl Pts',(-38.544592851426,35.7275576179694,14.6438546054077));
#42171=CARTESIAN_POINT('Ctrl Pts',(-39.0000123547097,35.7074046291006,14.608238812539));
#42172=CARTESIAN_POINT('Ctrl Pts',(-38.9999999998175,35.4759702897537,14.2134937397502));
#42173=CARTESIAN_POINT('Ctrl Pts',(-38.5349127504493,35.7535087720731,14.630248787943));
#42174=CARTESIAN_POINT('Ctrl Pts',(-39.0000127309186,35.7387100140626,14.6011426709817));
#42175=CARTESIAN_POINT('Ctrl Pts',(-38.9999999998136,35.5187772848732,14.1895929445726));
#42176=CARTESIAN_POINT('Ctrl Pts',(-38.5154067371474,35.8068058703489,14.6055899230286));
#42177=CARTESIAN_POINT('Ctrl Pts',(-39.0000135135293,35.8013704615112,14.5915224275482));
#42178=CARTESIAN_POINT('Ctrl Pts',(-38.9999999998058,35.607043756353,14.1469469425535));
#42179=CARTESIAN_POINT('Ctrl Pts',(-38.5055809150832,35.8341515672782,14.594536987818));
#42180=CARTESIAN_POINT('Ctrl Pts',(-39.0000139208182,35.8327499432145,14.5890804612011));
#42181=CARTESIAN_POINT('Ctrl Pts',(-38.9999999998018,35.6525028236316,14.1282019299212));
#42182=CARTESIAN_POINT('Ctrl Pts',(-38.4859536041471,35.8897642585238,14.5751753147767));
#42183=CARTESIAN_POINT('Ctrl Pts',(-39.0000147628207,35.8945620836492,14.5886989627516));
#42184=CARTESIAN_POINT('Ctrl Pts',(-38.999999999794,35.7452863002563,14.0961921325892));
#42185=CARTESIAN_POINT('Ctrl Pts',(-38.4761522059002,35.9180309954215,14.5668666644427));
#42186=CARTESIAN_POINT('Ctrl Pts',(-39.0000151983183,35.9249907258467,14.5908493270198));
#42187=CARTESIAN_POINT('Ctrl Pts',(-38.99999999979,35.792610280322,14.0829274926165));
#42188=CARTESIAN_POINT('Ctrl Pts',(-38.4567434646595,35.974996318516,14.5531374737745));
#42189=CARTESIAN_POINT('Ctrl Pts',(-39.0000160927976,35.9839070296273,14.5993741709333));
#42190=CARTESIAN_POINT('Ctrl Pts',(-38.9999999997822,35.8883041425332,14.0621081867874));
#42191=CARTESIAN_POINT('Ctrl Pts',(-38.4471362110153,36.0036946418055,14.5477169947031));
#42192=CARTESIAN_POINT('Ctrl Pts',(-39.0000165523838,36.0123586893398,14.6058379828008));
#42193=CARTESIAN_POINT('Ctrl Pts',(-38.9999999997784,35.9366735829977,14.0545536137068));
#42194=CARTESIAN_POINT('Ctrl Pts',(-38.4282821195088,36.0610262084247,14.5398580520424));
#42195=CARTESIAN_POINT('Ctrl Pts',(-39.0000174895439,36.0663818685961,14.6224820332273));
#42196=CARTESIAN_POINT('Ctrl Pts',(-38.9999999997708,36.033620814048,14.0452853161319));
#42197=CARTESIAN_POINT('Ctrl Pts',(-38.4190353681169,36.089659188121,14.5374196225146));
#42198=CARTESIAN_POINT('Ctrl Pts',(-39.0000179674514,36.0918849124185,14.6327409659728));
#42199=CARTESIAN_POINT('Ctrl Pts',(-38.9999999997671,36.0821981585482,14.0435716310186));
#42200=CARTESIAN_POINT('Ctrl Pts',(-38.4010623993245,36.146364260849,14.5355670505141));
#42201=CARTESIAN_POINT('Ctrl Pts',(-39.0000189337675,36.1391959072527,14.6562284569052));
#42202=CARTESIAN_POINT('Ctrl Pts',(-38.9999999997599,36.1787200361203,14.0460148457356));
#42203=CARTESIAN_POINT('Ctrl Pts',(-38.392336263983,36.1744360942504,14.5361529144741));
#42204=CARTESIAN_POINT('Ctrl Pts',(-39.0000194221385,36.1609066386604,14.6695142627742));
#42205=CARTESIAN_POINT('Ctrl Pts',(-38.9999999997564,36.2266641267153,14.050171731156));
#42206=CARTESIAN_POINT('Ctrl Pts',(-38.3755556305667,36.2295327745401,14.5403388340369));
#42207=CARTESIAN_POINT('Ctrl Pts',(-39.0000203994702,36.2000284416751,14.6980809799109));
#42208=CARTESIAN_POINT('Ctrl Pts',(-38.9999999997497,36.3210892901581,14.0642841698589));
#42209=CARTESIAN_POINT('Ctrl Pts',(-38.367501208712,36.2565573703884,14.5439388685547));
#42210=CARTESIAN_POINT('Ctrl Pts',(-39.0000208879253,36.2173223481235,14.713387954275));
#42211=CARTESIAN_POINT('Ctrl Pts',(-38.9999999997465,36.3675699319872,14.0742396555811));
#42212=CARTESIAN_POINT('Ctrl Pts',(-38.3522034742026,36.3090915989522,14.5540908400596));
#42213=CARTESIAN_POINT('Ctrl Pts',(-39.0000218527547,36.2473143300469,14.7448410689014));
#42214=CARTESIAN_POINT('Ctrl Pts',(-38.9999999997403,36.4582633219484,14.0997769689501));
#42215=CARTESIAN_POINT('Ctrl Pts',(-38.3449602306372,36.3346009935599,14.5606427290728));
#42216=CARTESIAN_POINT('Ctrl Pts',(-39.0000223280847,36.2598891039266,14.7609760213118));
#42217=CARTESIAN_POINT('Ctrl Pts',(-38.9999999997374,36.5024756580302,14.1153586775199));
#42218=CARTESIAN_POINT('Ctrl Pts',(-38.3314102784294,36.3836630691935,14.5765850031111));
#42219=CARTESIAN_POINT('Ctrl Pts',(-39.0000232511576,36.2805499895026,14.7928435792589));
#42220=CARTESIAN_POINT('Ctrl Pts',(-38.999999999732,36.5878668276054,14.1518786846698));
#42221=CARTESIAN_POINT('Ctrl Pts',(-38.3251036306141,36.4072155290489,14.5859753143807));
#42222=CARTESIAN_POINT('Ctrl Pts',(-39.0000236973072,36.2885237503305,14.8085282882104));
#42223=CARTESIAN_POINT('Ctrl Pts',(-38.9999999997295,36.6290452750275,14.1728168152053));
#42224=CARTESIAN_POINT('Ctrl Pts',(-38.3135360779263,36.4519558604292,14.607431870355));
#42225=CARTESIAN_POINT('Ctrl Pts',(-39.0000245440666,36.3005570344607,14.8383222788334));
#42226=CARTESIAN_POINT('Ctrl Pts',(-38.9999999997248,36.7076555825882,14.2196871579371));
#42227=CARTESIAN_POINT('Ctrl Pts',(-38.3082751784691,36.4731437264623,14.6194981478164));
#42228=CARTESIAN_POINT('Ctrl Pts',(-39.0000249426352,36.3045330498124,14.852363427476));
#42229=CARTESIAN_POINT('Ctrl Pts',(-38.9999999997227,36.745087131247,14.2456191901704));
#42230=CARTESIAN_POINT('Ctrl Pts',(-38.3035827917596,36.4929654448321,14.6327976801015));
#42231=CARTESIAN_POINT('Ctrl Pts',(-39.0000253059108,36.3070470821327,14.865052826966));
#42232=CARTESIAN_POINT('Ctrl Pts',(-38.9999999997209,36.7803212016997,14.2738237060164));
#42233=CARTESIAN_POINT('',(-38.9808995532817,35.0987932250002,14.8625310449412));
#42234=CARTESIAN_POINT('',(-39.,36.7598993715046,14.257937916702));
#42235=CARTESIAN_POINT('Ctrl Pts',(-38.9808995442742,35.0987933242929,14.8625310222129));
#42236=CARTESIAN_POINT('Ctrl Pts',(-38.9767647379296,35.116349019978,14.8561412678243));
#42237=CARTESIAN_POINT('Ctrl Pts',(-38.9719271471844,35.1341609379785,14.8496306127704));
#42238=CARTESIAN_POINT('Ctrl Pts',(-38.9663672797599,35.1521966963304,14.8430315129897));
#42239=CARTESIAN_POINT('Ctrl Pts',(-38.9589054668452,35.176402211376,14.8341749622469));
#42240=CARTESIAN_POINT('Ctrl Pts',(-38.9501421609617,35.2010095699642,14.8251608525414));
#42241=CARTESIAN_POINT('Ctrl Pts',(-38.9400483440121,35.2259561953471,14.8160432642181));
#42242=CARTESIAN_POINT('Ctrl Pts',(-38.9308756360675,35.2486263220181,14.8077576993751));
#42243=CARTESIAN_POINT('Ctrl Pts',(-38.9206045220855,35.2715762307629,14.7993865402743));
#42244=CARTESIAN_POINT('Ctrl Pts',(-38.9092251669917,35.2947851487066,14.7909462729069));
#42245=CARTESIAN_POINT('Ctrl Pts',(-38.8978601608867,35.3179648009758,14.7825166484363));
#42246=CARTESIAN_POINT('Ctrl Pts',(-38.8853895090675,35.3414022162457,14.7740185519616));
#42247=CARTESIAN_POINT('Ctrl Pts',(-38.8718153038447,35.3651025799904,14.7654350181464));
#42248=CARTESIAN_POINT('Ctrl Pts',(-38.8629383335795,35.380601640214,14.7598217411112));
#42249=CARTESIAN_POINT('Ctrl Pts',(-38.8535896256093,35.3962138014434,14.7541712904865));
#42250=CARTESIAN_POINT('Ctrl Pts',(-38.8437734577105,35.411950727854,14.7484733033058));
#42251=CARTESIAN_POINT('Ctrl Pts',(-38.8299407627953,35.4341268055438,14.7404438442426));
#42252=CARTESIAN_POINT('Ctrl Pts',(-38.8151786393598,35.4565484470982,14.7323203526436));
#42253=CARTESIAN_POINT('Ctrl Pts',(-38.7995152955661,35.4792736089631,14.7240525449706));
#42254=CARTESIAN_POINT('Ctrl Pts',(-38.7936375981427,35.4878012660903,14.7209500355386));
#42255=CARTESIAN_POINT('Ctrl Pts',(-38.7876332216565,35.4963721011908,14.7178271266627));
#42256=CARTESIAN_POINT('Ctrl Pts',(-38.7815045885274,35.5049909053511,14.7146810901815));
#42257=CARTESIAN_POINT('Ctrl Pts',(-38.7795162123981,35.5077871935437,14.7136603888752));
#42258=CARTESIAN_POINT('Ctrl Pts',(-38.7771942222782,35.5110389942361,14.7124711412873));
#42259=CARTESIAN_POINT('Ctrl Pts',(-38.7751079474046,35.5139398250466,14.711413790367));
#42260=CARTESIAN_POINT('Ctrl Pts',(-38.7736879354939,35.5159142601288,14.7106941100797));
#42261=CARTESIAN_POINT('Ctrl Pts',(-38.7723780994354,35.517726392354,14.7100348526341));
#42262=CARTESIAN_POINT('Ctrl Pts',(-38.7713664599503,35.5191246936257,14.7095250845846));
#42263=CARTESIAN_POINT('Ctrl Pts',(-38.7591460919159,35.5360158454794,14.7033672059448));
#42264=CARTESIAN_POINT('Ctrl Pts',(-38.7459652690169,35.5537552475421,14.6968911730339));
#42265=CARTESIAN_POINT('Ctrl Pts',(-38.7317687459757,35.5723139069922,14.6901294727658));
#42266=CARTESIAN_POINT('Ctrl Pts',(-38.7232003627024,35.5835150797543,14.6860484143751));
#42267=CARTESIAN_POINT('Ctrl Pts',(-38.7142624901345,35.5950148086917,14.6818626484207));
#42268=CARTESIAN_POINT('Ctrl Pts',(-38.7049499967065,35.6068100037668,14.6775738863478));
#42269=CARTESIAN_POINT('Ctrl Pts',(-38.6914598459875,35.6238966154841,14.6713611521097));
#42270=CARTESIAN_POINT('Ctrl Pts',(-38.6771815904704,35.6416017827983,14.6649326897865));
#42271=CARTESIAN_POINT('Ctrl Pts',(-38.6621289822079,35.6599303559949,14.6582736496514));
#42272=CARTESIAN_POINT('Ctrl Pts',(-38.6529092037587,35.6711566751295,14.6541949628445));
#42273=CARTESIAN_POINT('Ctrl Pts',(-38.6433996162985,35.6826172647426,14.6500294703126));
#42274=CARTESIAN_POINT('Ctrl Pts',(-38.6336114709703,35.6943188541858,14.6457727995193));
#42275=CARTESIAN_POINT('Ctrl Pts',(-38.6307797553414,35.6977041302108,14.6445413424038));
#42276=CARTESIAN_POINT('Ctrl Pts',(-38.6279247708707,35.7011096036338,14.6433022574605));
#42277=CARTESIAN_POINT('Ctrl Pts',(-38.6250469058212,35.7045355081267,14.642055390223));
#42278=CARTESIAN_POINT('Ctrl Pts',(-38.6231484010499,35.7067955501765,14.6412328417856));
#42279=CARTESIAN_POINT('Ctrl Pts',(-38.6219577178143,35.70821201593,14.6407173324049));
#42280=CARTESIAN_POINT('Ctrl Pts',(-38.6193199827135,35.7113415310103,14.639578540854));
#42281=CARTESIAN_POINT('Ctrl Pts',(-38.6093963463712,35.7231153325473,14.6352942011503));
#42282=CARTESIAN_POINT('Ctrl Pts',(-38.600451520594,35.733924467879,14.6312927832749));
#42283=CARTESIAN_POINT('Ctrl Pts',(-38.5925313692603,35.7438150067674,14.6275978327402));
#42284=CARTESIAN_POINT('Ctrl Pts',(-38.5839175250442,35.7545718165312,14.6235792569642));
#42285=CARTESIAN_POINT('Ctrl Pts',(-38.5765151121156,35.7642419688015,14.6199244835375));
#42286=CARTESIAN_POINT('Ctrl Pts',(-38.5703367971687,35.7728453441612,14.6166607138016));
#42287=CARTESIAN_POINT('Ctrl Pts',(-38.5689416731234,35.7747880706065,14.6159237226194));
#42288=CARTESIAN_POINT('Ctrl Pts',(-38.5676088151344,35.7766762616162,14.6152066150956));
#42289=CARTESIAN_POINT('Ctrl Pts',(-38.5663381283992,35.7785099169919,14.6145095958068));
#42290=CARTESIAN_POINT('Ctrl Pts',(-38.5600210194182,35.7876257757806,14.6110444248188));
#42291=CARTESIAN_POINT('Ctrl Pts',(-38.5552431665246,35.7953964841108,14.6080782285374));
#42292=CARTESIAN_POINT('Ctrl Pts',(-38.5519704510026,35.8017991138177,14.6056167712994));
#42293=CARTESIAN_POINT('Ctrl Pts',(-38.5508098883644,35.8040695992216,14.6047438951552));
#42294=CARTESIAN_POINT('Ctrl Pts',(-38.5498383139863,35.8061677486475,14.603934201354));
#42295=CARTESIAN_POINT('Ctrl Pts',(-38.5490533846631,35.808091706157,14.603187009408));
#42296=CARTESIAN_POINT('Ctrl Pts',(-38.5486074101368,35.8091848441171,14.6027624761865));
#42297=CARTESIAN_POINT('Ctrl Pts',(-38.5485269918336,35.8092779875322,14.602729607332));
#42298=CARTESIAN_POINT('Ctrl Pts',(-38.5479678306013,35.8109932342015,14.602055342206));
#42299=CARTESIAN_POINT('Ctrl Pts',(-38.5479228048346,35.8111313523181,14.6020010478406));
#42300=CARTESIAN_POINT('Ctrl Pts',(-38.5478746740126,35.8112799988974,14.6019426209443));
#42301=CARTESIAN_POINT('Ctrl Pts',(-38.5478229968322,35.8114405509189,14.6018795418018));
#42302=CARTESIAN_POINT('Ctrl Pts',(-38.5449835603478,35.8202621867631,14.5984136170561));
#42303=CARTESIAN_POINT('Ctrl Pts',(-38.5433058289746,35.8292618452946,14.5949231012738));
#42304=CARTESIAN_POINT('Ctrl Pts',(-38.5427752974539,35.8384513754963,14.5914640211649));
#42305=CARTESIAN_POINT('Ctrl Pts',(-38.5423420551633,35.8459557234158,14.5886392695128));
#42306=CARTESIAN_POINT('Ctrl Pts',(-38.5426741373589,35.8535859788554,14.5858347064009));
#42307=CARTESIAN_POINT('Ctrl Pts',(-38.5437703713166,35.8613377512468,14.5830585045683));
#42308=CARTESIAN_POINT('Ctrl Pts',(-38.5451107571661,35.8708159889432,14.579663990445));
#42309=CARTESIAN_POINT('Ctrl Pts',(-38.5475935941593,35.8804757210054,14.5763134226948));
#42310=CARTESIAN_POINT('Ctrl Pts',(-38.5512260819329,35.890297003835,14.5729770455601));
#42311=CARTESIAN_POINT('Ctrl Pts',(-38.5547558391688,35.8998405305566,14.569735024646));
#42312=CARTESIAN_POINT('Ctrl Pts',(-38.5593717925242,35.909535959512,14.5665064366129));
#42313=CARTESIAN_POINT('Ctrl Pts',(-38.5650829120781,35.9193616198279,14.5632169645182));
#42314=CARTESIAN_POINT('Ctrl Pts',(-38.5658016677034,35.9205981984981,14.5628029779872));
#42315=CARTESIAN_POINT('Ctrl Pts',(-38.5671656761932,35.922871397621,14.5620409226064));
#42316=CARTESIAN_POINT('Ctrl Pts',(-38.567290740915,35.9230774137073,14.5619718110317));
#42317=CARTESIAN_POINT('Ctrl Pts',(-38.5682304871265,35.924625434875,14.561452501193));
#42318=CARTESIAN_POINT('Ctrl Pts',(-38.570461396946,35.9276549380703,14.5603840529096));
#42319=CARTESIAN_POINT('Ctrl Pts',(-38.5739282260106,35.9321429471728,14.5587879606264));
#42320=CARTESIAN_POINT('Ctrl Pts',(-38.5766210025586,35.9356289008882,14.5575482341246));
#42321=CARTESIAN_POINT('Ctrl Pts',(-38.58006088657,35.9399948247985,14.5559900602808));
#42322=CARTESIAN_POINT('Ctrl Pts',(-38.5842425702584,35.9452337123745,14.5541188046349));
#42323=CARTESIAN_POINT('Ctrl Pts',(-38.5902071488439,35.9527062423353,14.5514497239044));
#42324=CARTESIAN_POINT('Ctrl Pts',(-38.5976806527857,35.9619529111913,14.5481458695105));
#42325=CARTESIAN_POINT('Ctrl Pts',(-38.6066862825953,35.9729747446293,14.5441966642552));
#42326=CARTESIAN_POINT('Ctrl Pts',(-38.6144225315189,35.9824430049148,14.5408041158659));
#42327=CARTESIAN_POINT('Ctrl Pts',(-38.6232918494035,35.9932206612145,14.5369352592365));
#42328=CARTESIAN_POINT('Ctrl Pts',(-38.6333101538699,36.0053367931859,14.5325548376229));
#42329=CARTESIAN_POINT('Ctrl Pts',(-38.634953979492,36.0073248349989,14.5318360883267));
#42330=CARTESIAN_POINT('Ctrl Pts',(-38.6366286984273,36.009348995464,14.5311034993255));
#42331=CARTESIAN_POINT('Ctrl Pts',(-38.6383343167614,36.0114095103981,14.5303568361756));
#42332=CARTESIAN_POINT('Ctrl Pts',(-38.6403446495301,36.0138381432345,14.5294767791504));
#42333=CARTESIAN_POINT('Ctrl Pts',(-38.6430226780081,36.0170741020974,14.5283029774242));
#42334=CARTESIAN_POINT('Ctrl Pts',(-38.6450720281982,36.0195454051338,14.5274039547414));
#42335=CARTESIAN_POINT('Ctrl Pts',(-38.6459862124317,36.0206478161728,14.5270029142719));
#42336=CARTESIAN_POINT('Ctrl Pts',(-38.6467744829065,36.0215977660742,14.5266569179816));
#42337=CARTESIAN_POINT('Ctrl Pts',(-38.6473190777943,36.022254636695,14.5264177462369));
#42338=CARTESIAN_POINT('Ctrl Pts',(-38.6495834782687,36.0249858744988,14.5254232811321));
#42339=CARTESIAN_POINT('Ctrl Pts',(-38.6518336507024,36.0277062660658,14.5244327799928));
#42340=CARTESIAN_POINT('Ctrl Pts',(-38.6540694260694,36.0304158360253,14.5234462803024));
#42341=CARTESIAN_POINT('Ctrl Pts',(-38.667469166842,36.0466551843962,14.5175338615874));
#42342=CARTESIAN_POINT('Ctrl Pts',(-38.6803477610403,36.0625071583347,14.5117657668271));
#42343=CARTESIAN_POINT('Ctrl Pts',(-38.6926983696478,36.0779736920762,14.5061390254219));
#42344=CARTESIAN_POINT('Ctrl Pts',(-38.6975666324403,36.0840701649816,14.5039211221026));
#42345=CARTESIAN_POINT('Ctrl Pts',(-38.7023533966268,36.0901065401151,14.5017250552718));
#42346=CARTESIAN_POINT('Ctrl Pts',(-38.7070601793549,36.0960821953089,14.4995499061324));
#42347=CARTESIAN_POINT('Ctrl Pts',(-38.7110458741123,36.1011423688826,14.4977079939341));
#42348=CARTESIAN_POINT('Ctrl Pts',(-38.7146256566631,36.1057104847595,14.4960433701251));
#42349=CARTESIAN_POINT('Ctrl Pts',(-38.7184672819383,36.1106486014496,14.4942458820026));
#42350=CARTESIAN_POINT('Ctrl Pts',(-38.7205521762747,36.1133285743211,14.4932703644708));
#42351=CARTESIAN_POINT('Ctrl Pts',(-38.7227146244336,36.1161180496071,14.4922552996327));
#42352=CARTESIAN_POINT('Ctrl Pts',(-38.7250639334399,36.1191596590394,14.4911476720038));
#42353=CARTESIAN_POINT('Ctrl Pts',(-38.725134081171,36.1192504780845,14.4911145994855));
#42354=CARTESIAN_POINT('Ctrl Pts',(-38.7252043956138,36.1193415222387,14.4910814442195));
#42355=CARTESIAN_POINT('Ctrl Pts',(-38.7252748796988,36.1194327953631,14.4910482047526));
#42356=CARTESIAN_POINT('Ctrl Pts',(-38.7391992330306,36.1374640890149,14.4844816431961));
#42357=CARTESIAN_POINT('Ctrl Pts',(-38.7525852683106,36.1552020757998,14.4780033780421));
#42358=CARTESIAN_POINT('Ctrl Pts',(-38.7653792735979,36.1726723554198,14.4716284835979));
#42359=CARTESIAN_POINT('Ctrl Pts',(-38.7756440047546,36.1866888982854,14.4665138556019));
#42360=CARTESIAN_POINT('Ctrl Pts',(-38.785528790763,36.2005323432467,14.4614663378914));
#42361=CARTESIAN_POINT('Ctrl Pts',(-38.7950264447249,36.214203378581,14.45649124442));
#42362=CARTESIAN_POINT('Ctrl Pts',(-38.8079002855734,36.2327341372116,14.4497476252259));
#42363=CARTESIAN_POINT('Ctrl Pts',(-38.8200619297502,36.2509486437685,14.4431385491419));
#42364=CARTESIAN_POINT('Ctrl Pts',(-38.8315338136742,36.268839344416,14.4366484694331));
#42365=CARTESIAN_POINT('Ctrl Pts',(-38.8395762860386,36.2813817887514,14.4320985378747));
#42366=CARTESIAN_POINT('Ctrl Pts',(-38.8472807935542,36.2937644106038,14.4276064034222));
#42367=CARTESIAN_POINT('Ctrl Pts',(-38.8546637596816,36.3059802738794,14.4231551143583));
#42368=CARTESIAN_POINT('Ctrl Pts',(-38.8563276050559,36.3087332741307,14.4221519597196));
#42369=CARTESIAN_POINT('Ctrl Pts',(-38.857677559501,36.3109841441762,14.4213330235564));
#42370=CARTESIAN_POINT('Ctrl Pts',(-38.8593427195925,36.3137774238209,14.4203146899841));
#42371=CARTESIAN_POINT('Ctrl Pts',(-38.8600372362967,36.3149424645772,14.4198899562424));
#42372=CARTESIAN_POINT('Ctrl Pts',(-38.8607863197798,36.3162022978644,14.4194305167246));
#42373=CARTESIAN_POINT('Ctrl Pts',(-38.8616341123971,36.3176350562414,14.4189085099844));
#42374=CARTESIAN_POINT('Ctrl Pts',(-38.8620353308256,36.3183131101108,14.4186614699421));
#42375=CARTESIAN_POINT('Ctrl Pts',(-38.8624357283147,36.318990958965,14.4184144479097));
#42376=CARTESIAN_POINT('Ctrl Pts',(-38.8628353023743,36.3196686044897,14.4181674451164));
#42377=CARTESIAN_POINT('Ctrl Pts',(-38.8747207051118,36.339825293296,14.4108203023155));
#42378=CARTESIAN_POINT('Ctrl Pts',(-38.8858742499577,36.3598051766581,14.4034902073188));
#42379=CARTESIAN_POINT('Ctrl Pts',(-38.8962515739831,36.3796455861763,14.3962075160251));
#42380=CARTESIAN_POINT('Ctrl Pts',(-38.9073388406698,36.4008433353228,14.3884265948192));
#42381=CARTESIAN_POINT('Ctrl Pts',(-38.9175408702454,36.4218807760399,14.3807005684331));
#42382=CARTESIAN_POINT('Ctrl Pts',(-38.9268423622115,36.4427703158319,14.3730516163559));
#42383=CARTESIAN_POINT('Ctrl Pts',(-38.9383225424702,36.4685528121461,14.3636110503739));
#42384=CARTESIAN_POINT('Ctrl Pts',(-38.9484320971274,36.494109926635,14.354288799014));
#42385=CARTESIAN_POINT('Ctrl Pts',(-38.9571837010109,36.5194437401331,14.345086390156));
#42386=CARTESIAN_POINT('Ctrl Pts',(-38.9661019465223,36.5452599415428,14.3357087557723));
#42387=CARTESIAN_POINT('Ctrl Pts',(-38.9736123558276,36.5708426756316,14.3264533231054));
#42388=CARTESIAN_POINT('Ctrl Pts',(-38.9797348916918,36.5961815584403,14.3172922402715));
#42389=CARTESIAN_POINT('Ctrl Pts',(-38.9864757782507,36.6240795631782,14.3072059261181));
#42390=CARTESIAN_POINT('Ctrl Pts',(-38.9915356867791,36.6516828688677,14.2972307775915));
#42391=CARTESIAN_POINT('Ctrl Pts',(-38.9949170488217,36.6789767320434,14.287338916061));
#42392=CARTESIAN_POINT('Ctrl Pts',(-38.9978813548361,36.7029041795484,14.27866711332));
#42393=CARTESIAN_POINT('Ctrl Pts',(-38.9995545419852,36.7265941813416,14.2700581931021));
#42394=CARTESIAN_POINT('Ctrl Pts',(-38.9999223536161,36.7500252217522,14.261531615527));
#42395=CARTESIAN_POINT('Ctrl Pts',(-38.9999741020041,36.7533217966002,14.2603319888489));
#42396=CARTESIAN_POINT('Ctrl Pts',(-38.9999999996542,36.7566132194275,14.2591340723458));
#42397=CARTESIAN_POINT('Ctrl Pts',(-39.,36.7598994028097,14.2579380027121));
#42398=CARTESIAN_POINT('',(-38.7236068457623,35.3906903574536,15.2883751610654));
#42399=CARTESIAN_POINT('Ctrl Pts',(-38.7236068979077,35.3906894271638,15.2883726211906));
#42400=CARTESIAN_POINT('Ctrl Pts',(-38.7246641593601,35.3897885482407,15.2874430895349));
#42401=CARTESIAN_POINT('Ctrl Pts',(-38.7250262636518,35.389481991673,15.2871302835944));
#42402=CARTESIAN_POINT('Ctrl Pts',(-38.7514788663481,35.3668699550198,15.2636753415614));
#42403=CARTESIAN_POINT('Ctrl Pts',(-38.8224426853319,35.3062619186145,15.2008982931996));
#42404=CARTESIAN_POINT('Ctrl Pts',(-38.9289695382785,35.1867017408949,15.0281412453392));
#42405=CARTESIAN_POINT('Ctrl Pts',(-38.9617634006977,35.140307300847,14.9486149885387));
#42406=CARTESIAN_POINT('Ctrl Pts',(-38.9808995805048,35.0987931708383,14.8625310771125));
#42407=CARTESIAN_POINT('Origin',(-38.5,36.0210562685922,15.0589436103097));
#42408=CARTESIAN_POINT('Origin',(-38.9999999999999,36.0210586628155,15.058945287974));
#42409=CARTESIAN_POINT('Origin',(-40.02360679775,35.3051952361797,15.3194957179792));
#42410=CARTESIAN_POINT('',(-39.,35.2608289688876,15.335643718679));
#42411=CARTESIAN_POINT('Origin',(-38.5,40.3013122161429,14.5652356228366));
#42412=CARTESIAN_POINT('',(-39.,44.2395480203679,13.1318350145773));
#42413=CARTESIAN_POINT('Origin',(-38.5,44.2395480203679,13.1318350145773));
#42414=CARTESIAN_POINT('',(-39.,44.9997753200724,12.8551349062082));
#42415=CARTESIAN_POINT('Ctrl Pts',(-38.4957681230772,43.7146667366125,11.7267038890717));
#42416=CARTESIAN_POINT('Ctrl Pts',(-39.,43.716193831966,11.7306891746095));
#42417=CARTESIAN_POINT('Ctrl Pts',(-39.,43.5357661657807,11.2598241647595));
#42418=CARTESIAN_POINT('Ctrl Pts',(-38.5104887561845,43.755952609823,11.7110172571947));
#42419=CARTESIAN_POINT('Ctrl Pts',(-39.0000000000001,43.7513673016004,11.7015437407619));
#42420=CARTESIAN_POINT('Ctrl Pts',(-39.,43.6045049054216,11.2334846192326));
#42421=CARTESIAN_POINT('Ctrl Pts',(-38.5252362294721,43.7984294432773,11.6983678551985));
#42422=CARTESIAN_POINT('Ctrl Pts',(-39.,43.7911361284587,11.675132616616));
#42423=CARTESIAN_POINT('Ctrl Pts',(-39.,43.675600497817,11.2132286937603));
#42424=CARTESIAN_POINT('Ctrl Pts',(-38.5542137101166,43.8841199255624,11.6796331382235));
#42425=CARTESIAN_POINT('Ctrl Pts',(-39.,43.8764894776903,11.6313912291823));
#42426=CARTESIAN_POINT('Ctrl Pts',(-39.,43.819752056524,11.1856680867503));
#42427=CARTESIAN_POINT('Ctrl Pts',(-38.5684428387846,43.9273310021072,11.6735484618443));
#42428=CARTESIAN_POINT('Ctrl Pts',(-39.,43.9219957425488,11.6137920684096));
#42429=CARTESIAN_POINT('Ctrl Pts',(-39.,43.8928036600594,11.1783643871917));
#42430=CARTESIAN_POINT('Ctrl Pts',(-38.5958298929736,44.0128086259304,11.668180454929));
#42431=CARTESIAN_POINT('Ctrl Pts',(-39.,44.0157276825881,11.5890560462835));
#42432=CARTESIAN_POINT('Ctrl Pts',(-39.,44.0380247156817,11.1769935191695));
#42433=CARTESIAN_POINT('Ctrl Pts',(-38.6089871338095,44.0550730387334,11.6688972641344));
#42434=CARTESIAN_POINT('Ctrl Pts',(-39.,44.0640020110278,11.5816534952057));
#42435=CARTESIAN_POINT('Ctrl Pts',(-39.,44.1101905494472,11.1829263849608));
#42436=CARTESIAN_POINT('Ctrl Pts',(-38.6337186415401,44.1370136007802,11.6771046639679));
#42437=CARTESIAN_POINT('Ctrl Pts',(-39.,44.1601223386003,11.5778169161264));
#42438=CARTESIAN_POINT('Ctrl Pts',(-39.,44.2508333864788,11.2077985694355));
#42439=CARTESIAN_POINT('Ctrl Pts',(-38.6452922898437,44.1766877029697,11.6845950548096));
#42440=CARTESIAN_POINT('Ctrl Pts',(-39.,44.2081128144266,11.5811665269809));
#42441=CARTESIAN_POINT('Ctrl Pts',(-39.,44.3193068873798,11.2267372688822));
#42442=CARTESIAN_POINT('Ctrl Pts',(-38.6664064032844,44.251904572198,11.7060586330073));
#42443=CARTESIAN_POINT('Ctrl Pts',(-39.,44.3006750969489,11.598562111161));
#42444=CARTESIAN_POINT('Ctrl Pts',(-39.,44.4499018395266,11.2768852145754));
#42445=CARTESIAN_POINT('Ctrl Pts',(-38.6759463402347,44.2874454600443,11.7200312889306));
#42446=CARTESIAN_POINT('Ctrl Pts',(-39.,44.3454481642641,11.6124687294269));
#42447=CARTESIAN_POINT('Ctrl Pts',(-39.,44.5120200408709,11.3080932130564));
#42448=CARTESIAN_POINT('Ctrl Pts',(-38.6926218940153,44.3530134983602,11.753916307973));
#42449=CARTESIAN_POINT('Ctrl Pts',(-39.,44.428901013663,11.6500339784918));
#42450=CARTESIAN_POINT('Ctrl Pts',(-39.,44.6274882090049,11.3815666424003));
#42451=CARTESIAN_POINT('Ctrl Pts',(-38.6997570937363,44.3830390111172,11.7738278290408));
#42452=CARTESIAN_POINT('Ctrl Pts',(-39.,44.4677973706649,11.6736416532639));
#42453=CARTESIAN_POINT('Ctrl Pts',(-39.,44.6808353045031,11.4238302464452));
#42454=CARTESIAN_POINT('Ctrl Pts',(-38.7113455437151,44.4364083250159,11.8188165042088));
#42455=CARTESIAN_POINT('Ctrl Pts',(-39.,44.5372576216464,11.7291039591263));
#42456=CARTESIAN_POINT('Ctrl Pts',(-39.,44.7766860774448,11.5177717429142));
#42457=CARTESIAN_POINT('Ctrl Pts',(-38.7157985041745,44.4597507937971,11.8438925388205));
#42458=CARTESIAN_POINT('Ctrl Pts',(-39.,44.5680147948136,11.760993098812));
#42459=CARTESIAN_POINT('Ctrl Pts',(-39.,44.8191873730925,11.5694473011972));
#42460=CARTESIAN_POINT('Ctrl Pts',(-38.7218491523116,44.4988458933973,11.8982352839493));
#42461=CARTESIAN_POINT('Ctrl Pts',(-39.,44.619483259022,11.8310677445932));
#42462=CARTESIAN_POINT('Ctrl Pts',(-39.,44.8916930695162,11.6802034356976));
#42463=CARTESIAN_POINT('Ctrl Pts',(-38.7234466887105,44.514597548933,11.9275006414011));
#42464=CARTESIAN_POINT('Ctrl Pts',(-39.,44.6403325524953,11.869358484827));
#42465=CARTESIAN_POINT('Ctrl Pts',(-39.,44.9216956695369,11.7392812613325));
#42466=CARTESIAN_POINT('Ctrl Pts',(-38.7237242128408,44.5378980584001,11.9890841057603));
#42467=CARTESIAN_POINT('Ctrl Pts',(-39.,44.6708633890369,11.9499591289122));
#42468=CARTESIAN_POINT('Ctrl Pts',(-39.,44.9680365091014,11.8625446758251));
#42469=CARTESIAN_POINT('Ctrl Pts',(-38.7224041936341,44.5454463318916,12.0214006787586));
#42470=CARTESIAN_POINT('Ctrl Pts',(-39.,44.6806049880233,11.9924212363057));
#42471=CARTESIAN_POINT('Ctrl Pts',(-39.,44.9843735979966,11.9267272040495));
#42472=CARTESIAN_POINT('Ctrl Pts',(-38.7168978002672,44.5520461127452,12.0878299294229));
#42473=CARTESIAN_POINT('Ctrl Pts',(-39.,44.6884337596283,12.0788836807004));
#42474=CARTESIAN_POINT('Ctrl Pts',(-39.,45.0027473637736,12.0577041266596));
#42475=CARTESIAN_POINT('Ctrl Pts',(-38.7127115637761,44.5510974570559,12.1219409519436));
#42476=CARTESIAN_POINT('Ctrl Pts',(-39.,44.6864915499809,12.1230533895049));
#42477=CARTESIAN_POINT('Ctrl Pts',(-39.,45.0047835844392,12.1244952683306));
#42478=CARTESIAN_POINT('Ctrl Pts',(-38.7016354079073,44.5407398453553,12.1906326060098));
#42479=CARTESIAN_POINT('Ctrl Pts',(-39.,44.6711238494387,12.210373277459));
#42480=CARTESIAN_POINT('Ctrl Pts',(-39.,44.9944757119117,12.2580919452284));
#42481=CARTESIAN_POINT('Ctrl Pts',(-38.6947457655101,44.5313311502024,12.2252115255115));
#42482=CARTESIAN_POINT('Ctrl Pts',(-39.,44.6575804147925,12.2536773253778));
#42483=CARTESIAN_POINT('Ctrl Pts',(-39.,44.982131874978,12.3248941610696));
#42484=CARTESIAN_POINT('Ctrl Pts',(-38.6785306211109,44.5044189374293,12.2934942107537));
#42485=CARTESIAN_POINT('Ctrl Pts',(-39.,44.6198413622739,12.3367624214714));
#42486=CARTESIAN_POINT('Ctrl Pts',(-39.,44.9435432418528,12.4559149547927));
#42487=CARTESIAN_POINT('Ctrl Pts',(-38.6692055246944,44.486916094711,12.3271962742984));
#42488=CARTESIAN_POINT('Ctrl Pts',(-39.,44.5954530285034,12.3766497399001));
#42489=CARTESIAN_POINT('Ctrl Pts',(-39.,44.9172994052938,12.5201302750391));
#42490=CARTESIAN_POINT('Ctrl Pts',(-38.6484820298786,44.4444958642473,12.3924145118707));
#42491=CARTESIAN_POINT('Ctrl Pts',(-39.,44.537496750665,12.4505883516032));
#42492=CARTESIAN_POINT('Ctrl Pts',(-39.,44.851930741321,12.6434797252075));
#42493=CARTESIAN_POINT('Ctrl Pts',(-38.6370841498941,44.4195795393625,12.4239290601754));
#42494=CARTESIAN_POINT('Ctrl Pts',(-39.,44.5036878365839,12.4846706149496));
#42495=CARTESIAN_POINT('Ctrl Pts',(-39.,44.8128075406341,12.7026107858961));
#42496=CARTESIAN_POINT('Ctrl Pts',(-38.612658278484,44.36330096768,12.4835465298239));
#42497=CARTESIAN_POINT('Ctrl Pts',(-39.,44.4289638773543,12.5450197756454));
#42498=CARTESIAN_POINT('Ctrl Pts',(-39.,44.7232010636579,12.8134917740948));
#42499=CARTESIAN_POINT('Ctrl Pts',(-38.5996308980214,44.3319401302231,12.511647965753));
#42500=CARTESIAN_POINT('Ctrl Pts',(-39.,44.3877977020642,12.5712233390459));
#42501=CARTESIAN_POINT('Ctrl Pts',(-39.,44.6727200187587,12.8652389406661));
#42502=CARTESIAN_POINT('Ctrl Pts',(-38.5724526116315,44.2639918355033,12.5633461379396));
#42503=CARTESIAN_POINT('Ctrl Pts',(-39.,44.3009663522788,12.6143232592351));
#42504=CARTESIAN_POINT('Ctrl Pts',(-39.,44.5623605667487,12.9593392527306));
#42505=CARTESIAN_POINT('Ctrl Pts',(-38.5583023852123,44.2274060787236,12.5869415874867));
#42506=CARTESIAN_POINT('Ctrl Pts',(-39.,44.2550869417833,12.6310565225753));
#42507=CARTESIAN_POINT('Ctrl Pts',(-39.,44.5024849092967,13.0016900538045));
#42508=CARTESIAN_POINT('Ctrl Pts',(-38.5294286852375,44.1504305117409,12.6287098869748));
#42509=CARTESIAN_POINT('Ctrl Pts',(-39.,44.1618651290856,12.6543799114258));
#42510=CARTESIAN_POINT('Ctrl Pts',(-39.,44.3756644133745,13.0753500839617));
#42511=CARTESIAN_POINT('Ctrl Pts',(-38.5147061045232,44.1100431097314,12.6468815233693));
#42512=CARTESIAN_POINT('Ctrl Pts',(-39.,44.1143989355615,12.660720422544));
#42513=CARTESIAN_POINT('Ctrl Pts',(-39.,44.3087235418349,13.1066571838109));
#42514=CARTESIAN_POINT('Ctrl Pts',(-38.4999828339055,44.0685379488058,12.6619887044612));
#42515=CARTESIAN_POINT('Ctrl Pts',(-39.,44.0685320774541,12.661972573055));
#42516=CARTESIAN_POINT('Ctrl Pts',(-39.,44.2395480203679,13.1318350145773));
#42517=CARTESIAN_POINT('',(-39.,43.5555078199205,11.2524499908864));
#42518=CARTESIAN_POINT('Ctrl Pts',(-38.5439382020836,43.7465865791704,11.7129332004299));
#42519=CARTESIAN_POINT('Ctrl Pts',(-38.5627108024178,43.7454905093906,11.7115697786477));
#42520=CARTESIAN_POINT('Ctrl Pts',(-38.5818394836764,43.7440439920326,11.7091586579251));
#42521=CARTESIAN_POINT('Ctrl Pts',(-38.6011103776041,43.7422011778166,11.7055948274057));
#42522=CARTESIAN_POINT('Ctrl Pts',(-38.6202864790502,43.7403674283036,11.7020485271752));
#42523=CARTESIAN_POINT('Ctrl Pts',(-38.639602741903,43.7381411164017,11.6973604045454));
#42524=CARTESIAN_POINT('Ctrl Pts',(-38.6588261733529,43.7354930847464,11.6914710015509));
#42525=CARTESIAN_POINT('Ctrl Pts',(-38.6780496048027,43.7328450530911,11.6855815985564));
#42526=CARTESIAN_POINT('Ctrl Pts',(-38.6971794210865,43.729775197568,11.6784906291453));
#42527=CARTESIAN_POINT('Ctrl Pts',(-38.7159711064253,43.7262723900725,11.6701881703371));
#42528=CARTESIAN_POINT('Ctrl Pts',(-38.7336425594366,43.7229783961093,11.6623806475916));
#42529=CARTESIAN_POINT('Ctrl Pts',(-38.7510179611022,43.7192998641312,11.6535001143584));
#42530=CARTESIAN_POINT('Ctrl Pts',(-38.7678799008077,43.7152435234236,11.6435908256301));
#42531=CARTESIAN_POINT('Ctrl Pts',(-38.7846868277303,43.7112004166971,11.6337138663705));
#42532=CARTESIAN_POINT('Ctrl Pts',(-38.8009828486583,43.7067820402673,11.6228150671742));
#42533=CARTESIAN_POINT('Ctrl Pts',(-38.8165686297444,43.702011877337,11.6109844626736));
#42534=CARTESIAN_POINT('Ctrl Pts',(-38.8321255085374,43.6972505602032,11.5991757968617));
#42535=CARTESIAN_POINT('Ctrl Pts',(-38.8469740663892,43.6921389056185,11.5864391783255));
#42536=CARTESIAN_POINT('Ctrl Pts',(-38.860943297614,43.6867153771627,11.5729056582632));
#42537=CARTESIAN_POINT('Ctrl Pts',(-38.8638049456601,43.6856043475463,11.5701332672403));
#42538=CARTESIAN_POINT('Ctrl Pts',(-38.8666298041761,43.6844802762301,11.5673275608693));
#42539=CARTESIAN_POINT('Ctrl Pts',(-38.8694165842623,43.6833435624567,11.5644898541878));
#42540=CARTESIAN_POINT('Ctrl Pts',(-38.8830703511397,43.6777742586767,11.5505865735923));
#42541=CARTESIAN_POINT('Ctrl Pts',(-38.8958018953305,43.6719012781054,11.5359181594009));
#42542=CARTESIAN_POINT('Ctrl Pts',(-38.907487219436,43.6657813607992,11.5206573183788));
#42543=CARTESIAN_POINT('Ctrl Pts',(-38.919187229744,43.6596537519353,11.5053772974177));
#42544=CARTESIAN_POINT('Ctrl Pts',(-38.9298380208449,43.6532788417078,11.4895040641895));
#42545=CARTESIAN_POINT('Ctrl Pts',(-38.9393615495029,43.646721800628,11.4732335514217));
#42546=CARTESIAN_POINT('Ctrl Pts',(-38.9489282990728,43.6401350015348,11.4568891977047));
#42547=CARTESIAN_POINT('Ctrl Pts',(-38.957357351642,43.6333646919751,11.440144712106));
#42548=CARTESIAN_POINT('Ctrl Pts',(-38.964620598952,43.6264811843718,11.4232103854808));
#42549=CARTESIAN_POINT('Ctrl Pts',(-38.9660145216253,43.6251601392647,11.4199604421934));
#42550=CARTESIAN_POINT('Ctrl Pts',(-38.967365659868,43.6238349302522,11.4167035214325));
#42551=CARTESIAN_POINT('Ctrl Pts',(-38.9686740335233,43.6225060587887,11.413441121867));
#42552=CARTESIAN_POINT('Ctrl Pts',(-38.9760247879083,43.6150401428423,11.3951121851654));
#42553=CARTESIAN_POINT('Ctrl Pts',(-38.9820201538307,43.6074604423925,11.3766151341195));
#42554=CARTESIAN_POINT('Ctrl Pts',(-38.9867094178029,43.5998495614506,11.3581761811704));
#42555=CARTESIAN_POINT('Ctrl Pts',(-38.9914661093554,43.5921292425905,11.3394720919461));
#42556=CARTESIAN_POINT('Ctrl Pts',(-38.9948792009387,43.5843770901683,11.3208284707058));
#42557=CARTESIAN_POINT('Ctrl Pts',(-38.9970499532579,43.5766720279274,11.3024613860455));
#42558=CARTESIAN_POINT('Ctrl Pts',(-38.9990538941774,43.5695590609736,11.2855057194795));
#42559=CARTESIAN_POINT('Ctrl Pts',(-38.9999999917031,43.5624862507436,11.2687857923547));
#42560=CARTESIAN_POINT('Ctrl Pts',(-39.,43.5555078257317,11.2524499884039));
#42561=CARTESIAN_POINT('Origin',(-39.,43.8975113829057,12.1921486462674));
#42562=CARTESIAN_POINT('Origin',(-38.5,39.6172719294915,12.6858503812648));
#42563=CARTESIAN_POINT('',(-39.,39.6172719294915,12.6858503812648));
#42564=CARTESIAN_POINT('Ctrl Pts',(-38.5,42.3431727827618,14.3786118971418));
#42565=CARTESIAN_POINT('Ctrl Pts',(-39.,42.3431727827618,14.3786118971418));
#42566=CARTESIAN_POINT('Ctrl Pts',(-39.,42.8199489247508,14.5292256761601));
#42567=CARTESIAN_POINT('Ctrl Pts',(-38.5000000151735,42.3235389145373,14.4407639791455));
#42568=CARTESIAN_POINT('Ctrl Pts',(-38.9808235694178,42.3295231330866,14.4218206445454));
#42569=CARTESIAN_POINT('Ctrl Pts',(-39.,42.7834708241676,14.5798104778281));
#42570=CARTESIAN_POINT('Ctrl Pts',(-38.5044132464344,42.3017127589935,14.5014168958436));
#42571=CARTESIAN_POINT('Ctrl Pts',(-38.9652824568155,42.3135424787352,14.4689442264536));
#42572=CARTESIAN_POINT('Ctrl Pts',(-39.0022066208479,42.7452111602329,14.6295830574807));
#42573=CARTESIAN_POINT('Ctrl Pts',(-38.5201182104299,42.2538679845483,14.6200333912239));
#42574=CARTESIAN_POINT('Ctrl Pts',(-38.9423369615246,42.2764879943097,14.5669878025861));
#42575=CARTESIAN_POINT('Ctrl Pts',(-39.0100591075842,42.6651957614355,14.7276861607036));
#42576=CARTESIAN_POINT('Ctrl Pts',(-38.5314246665614,42.227847908903,14.6779967191923));
#42577=CARTESIAN_POINT('Ctrl Pts',(-38.9346328775752,42.2555724552384,14.6178337748267));
#42578=CARTESIAN_POINT('Ctrl Pts',(-39.0157123318515,42.6234394464224,14.7760157468895));
#42579=CARTESIAN_POINT('Ctrl Pts',(-38.552651089205,42.1857348662789,14.7630638104245));
#42580=CARTESIAN_POINT('Ctrl Pts',(-38.9285245106868,42.2199024964374,14.6960761304899));
#42581=CARTESIAN_POINT('Ctrl Pts',(-39.0263255453171,42.5581752806135,14.8475077052381));
#42582=CARTESIAN_POINT('Ctrl Pts',(-38.5604419961988,42.1711826366542,14.7911056783425));
#42583=CARTESIAN_POINT('Ctrl Pts',(-38.9273730528816,42.2074674656466,14.7221761912045));
#42584=CARTESIAN_POINT('Ctrl Pts',(-39.0302209975595,42.5359817233398,14.8711708137875));
#42585=CARTESIAN_POINT('Ctrl Pts',(-38.5731186427038,42.1485842461019,14.832708622288));
#42586=CARTESIAN_POINT('Ctrl Pts',(-38.926916498768,42.1877378091319,14.7616810012592));
#42587=CARTESIAN_POINT('Ctrl Pts',(-39.0365593216219,42.5020273470754,14.9064206387115));
#42588=CARTESIAN_POINT('Ctrl Pts',(-38.5775094223885,42.1409230674214,14.846499586987));
#42589=CARTESIAN_POINT('Ctrl Pts',(-38.9269719591409,42.1810223729242,14.7748341780693));
#42590=CARTESIAN_POINT('Ctrl Pts',(-39.0387547109623,42.4905985146427,14.9181297528723));
#42591=CARTESIAN_POINT('Ctrl Pts',(-38.5866095911227,42.1253437576203,14.8739295117817));
#42592=CARTESIAN_POINT('Ctrl Pts',(-38.9274916449468,42.1672574095469,14.8011897647693));
#42593=CARTESIAN_POINT('Ctrl Pts',(-39.0433047957933,42.4675180576399,14.9414671669666));
#42594=CARTESIAN_POINT('Ctrl Pts',(-38.5913209172013,42.1174228143287,14.8875723296809));
#42595=CARTESIAN_POINT('Ctrl Pts',(-38.9279536908748,42.1602065716068,14.8143979542777));
#42596=CARTESIAN_POINT('Ctrl Pts',(-39.0456604581885,42.4558625514204,14.9530988371724));
#42597=CARTESIAN_POINT('Ctrl Pts',(-38.6155177819721,42.0773849632758,14.9550630836894));
#42598=CARTESIAN_POINT('Ctrl Pts',(-38.9311989887487,42.1246877033306,14.8794706017327));
#42599=CARTESIAN_POINT('Ctrl Pts',(-39.0577588926346,42.3973293691335,15.0107605238563));
#42600=CARTESIAN_POINT('Ctrl Pts',(-38.6370023785226,42.0438120311917,15.0070352766296));
#42601=CARTESIAN_POINT('Ctrl Pts',(-38.9368284508843,42.0937684062961,14.9316236792503));
#42602=CARTESIAN_POINT('Ctrl Pts',(-39.0685011882335,42.3494478230898,15.0555491513583));
#42603=CARTESIAN_POINT('Ctrl Pts',(-38.6834063423229,41.9737282317394,15.1073632756364));
#42604=CARTESIAN_POINT('Ctrl Pts',(-38.9532556851885,42.0277155354844,15.0338788517455));
#42605=CARTESIAN_POINT('Ctrl Pts',(-39.0917031721878,42.2515616380507,15.1427428606496));
#42606=CARTESIAN_POINT('Ctrl Pts',(-38.7083300695819,41.9372167755023,15.1557169775274));
#42607=CARTESIAN_POINT('Ctrl Pts',(-38.963949218556,41.9925965667856,15.0841722205039));
#42608=CARTESIAN_POINT('Ctrl Pts',(-39.1041650341826,42.2015570290535,15.1851464699237));
#42609=CARTESIAN_POINT('Ctrl Pts',(-38.7610633626364,41.8613333331087,15.2490754374726));
#42610=CARTESIAN_POINT('Ctrl Pts',(-38.9895991647772,41.9183569021626,15.1822592900656));
#42611=CARTESIAN_POINT('Ctrl Pts',(-39.1305316819265,42.0993810792371,15.2677629211416));
#42612=CARTESIAN_POINT('Ctrl Pts',(-38.7888752933149,41.8219610687487,15.2940790871008));
#42613=CARTESIAN_POINT('Ctrl Pts',(-39.0044992158228,41.8792245556372,15.2302347536082));
#42614=CARTESIAN_POINT('Ctrl Pts',(-39.1444376463372,42.0472098181495,15.3079749806063));
#42615=CARTESIAN_POINT('Ctrl Pts',(-38.8324659250877,41.7607737749083,15.3591954444135));
#42616=CARTESIAN_POINT('Ctrl Pts',(-39.0296343641317,41.8173594933725,15.3004082221224));
#42617=CARTESIAN_POINT('Ctrl Pts',(-39.166232962704,41.967271130407,15.3667436422317));
#42618=CARTESIAN_POINT('Ctrl Pts',(-38.8473093173328,41.7400227844779,15.3805019886511));
#42619=CARTESIAN_POINT('Ctrl Pts',(-39.0384151694295,41.7963453190696,15.3233737884774));
#42620=CARTESIAN_POINT('Ctrl Pts',(-39.1736546585605,41.940344345471,15.3860744919038));
#42621=CARTESIAN_POINT('Ctrl Pts',(-38.870015379526,41.7083619831663,15.4118730882152));
#42622=CARTESIAN_POINT('Ctrl Pts',(-39.0522271030963,41.7640415062336,15.357359413503));
#42623=CARTESIAN_POINT('Ctrl Pts',(-39.1850076898159,41.8995237784172,15.4146908074332));
#42624=CARTESIAN_POINT('Ctrl Pts',(-38.8776576124367,41.6977193058703,15.4222319640262));
#42625=CARTESIAN_POINT('Ctrl Pts',(-39.0569232021872,41.7531759506236,15.3685790901832));
#42626=CARTESIAN_POINT('Ctrl Pts',(-39.1888288061772,41.8858451739218,15.4241662290078));
#42627=CARTESIAN_POINT('Ctrl Pts',(-38.8930849110735,41.6762552578125,15.4427545725828));
#42628=CARTESIAN_POINT('Ctrl Pts',(-39.066511133906,41.7312068662022,15.3908393217828));
#42629=CARTESIAN_POINT('Ctrl Pts',(-39.1965424555779,41.8583426536247,15.4429914483156));
#42630=CARTESIAN_POINT('Ctrl Pts',(-38.9008746912715,41.66542735373,15.4529240043621));
#42631=CARTESIAN_POINT('Ctrl Pts',(-39.0714060895731,41.7200956440113,15.4018887144115));
#42632=CARTESIAN_POINT('Ctrl Pts',(-39.2004373455104,41.8445104908778,15.4523465539704));
#42633=CARTESIAN_POINT('Ctrl Pts',(-38.9400159979964,41.611054246107,15.5030904749622));
#42634=CARTESIAN_POINT('Ctrl Pts',(-39.0961105529348,41.664486384419,15.4561555034708));
#42635=CARTESIAN_POINT('Ctrl Pts',(-39.2200079994996,41.7752545712226,15.4986298218549));
#42636=CARTESIAN_POINT('Ctrl Pts',(-38.9720506860609,41.566657227979,15.5411994956368));
#42637=CARTESIAN_POINT('Ctrl Pts',(-39.1172505217694,41.6183487327083,15.4979423053299));
#42638=CARTESIAN_POINT('Ctrl Pts',(-39.2360252362306,41.7193499540182,15.5342207819066));
#42639=CARTESIAN_POINT('Ctrl Pts',(-39.004664367461,41.5213832040514,15.5774321632787));
#42640=CARTESIAN_POINT('Ctrl Pts',(-39.139478538059,41.5707159497276,15.537951312608));
#42641=CARTESIAN_POINT('Ctrl Pts',(-39.2523321837305,41.6629039474018,15.5684921983703));
#42642=CARTESIAN_POINT('',(-39.0936699647309,42.2443432359162,15.1482528495184));
#42643=CARTESIAN_POINT('Ctrl Pts',(-39.,41.5278577779161,15.5722329179818));
#42644=CARTESIAN_POINT('Ctrl Pts',(-39.,41.555365582337,15.5500682176439));
#42645=CARTESIAN_POINT('Ctrl Pts',(-39.0025061283031,41.6103743139319,15.5062349506866));
#42646=CARTESIAN_POINT('Ctrl Pts',(-39.011910467653,41.6938875962409,15.4431191586721));
#42647=CARTESIAN_POINT('Ctrl Pts',(-39.0251886793738,41.7791789788017,15.383441099477));
#42648=CARTESIAN_POINT('Ctrl Pts',(-39.0355006548008,41.8375977236174,15.3462767602701));
#42649=CARTESIAN_POINT('Ctrl Pts',(-39.0460180996933,41.8969209424409,15.3105044475851));
#42650=CARTESIAN_POINT('Ctrl Pts',(-39.0513795683656,41.9270342259527,15.2933134663306));
#42651=CARTESIAN_POINT('Ctrl Pts',(-39.0592129369566,41.9729415209881,15.2685857940176));
#42652=CARTESIAN_POINT('Ctrl Pts',(-39.0617895723962,41.9883665401829,15.2605193084358));
#42653=CARTESIAN_POINT('Ctrl Pts',(-39.0668167987977,42.0194688332009,15.2447375200145));
#42654=CARTESIAN_POINT('Ctrl Pts',(-39.0692638673594,42.0351249489564,15.2370331001163));
#42655=CARTESIAN_POINT('Ctrl Pts',(-39.0763170763895,42.0823578826811,15.2144966152885));
#42656=CARTESIAN_POINT('Ctrl Pts',(-39.0806383134429,42.1142224339666,15.2002291333683));
#42657=CARTESIAN_POINT('Ctrl Pts',(-39.086250870079,42.1626004871079,15.1799187978017));
#42658=CARTESIAN_POINT('Ctrl Pts',(-39.0888401552868,42.1869348076306,15.1700364166254));
#42659=CARTESIAN_POINT('Ctrl Pts',(-39.0914175141258,42.2155837611224,15.1589770191016));
#42660=CARTESIAN_POINT('Ctrl Pts',(-39.0924201592736,42.227917997062,15.15433750161));
#42661=CARTESIAN_POINT('Ctrl Pts',(-39.0929039086555,42.2340945254209,15.1520344157921));
#42662=CARTESIAN_POINT('Ctrl Pts',(-39.0930625659985,42.236159807516,15.1512676840144));
#42663=CARTESIAN_POINT('Ctrl Pts',(-39.0933714042916,42.2402499173753,15.1497569469128));
#42664=CARTESIAN_POINT('Ctrl Pts',(-39.0935224084833,42.2422960384328,15.1490037844944));
#42665=CARTESIAN_POINT('Ctrl Pts',(-39.0936699647319,42.2443432359167,15.1482528495195));
#42666=CARTESIAN_POINT('Ctrl Pts',(-39.0936699647319,42.2443432359167,15.1482528495195));
#42667=CARTESIAN_POINT('Ctrl Pts',(-39.0805958020047,42.2975092731202,15.1026169640987));
#42668=CARTESIAN_POINT('Ctrl Pts',(-39.0684075521881,42.3495683432789,15.0555700511839));
#42669=CARTESIAN_POINT('Ctrl Pts',(-39.0545825391346,42.413189511403,14.994849343675));
#42670=CARTESIAN_POINT('Ctrl Pts',(-39.0518885060209,42.4258409923919,14.9826093594223));
#42671=CARTESIAN_POINT('Ctrl Pts',(-39.0466519979229,42.4509962153533,14.9579329492598));
#42672=CARTESIAN_POINT('Ctrl Pts',(-39.0441085920868,42.4635046891825,14.945491722837));
#42673=CARTESIAN_POINT('Ctrl Pts',(-39.0367291513417,42.5007669083855,14.9079038797878));
#42674=CARTESIAN_POINT('Ctrl Pts',(-39.0321447527579,42.5252490627375,14.8825025364275));
#42675=CARTESIAN_POINT('Ctrl Pts',(-39.0195339780508,42.5975848409282,14.805227756089));
#42676=CARTESIAN_POINT('Ctrl Pts',(-39.0126341194485,42.6443310367265,14.752288032587));
#42677=CARTESIAN_POINT('Ctrl Pts',(-39.0053154013728,42.7120528329345,14.6705075551378));
#42678=CARTESIAN_POINT('Ctrl Pts',(-39.0033844025761,42.7342264354137,14.6428512503343));
#42679=CARTESIAN_POINT('Ctrl Pts',(-39.0007271289037,42.7777317502299,14.586691290421));
#42680=CARTESIAN_POINT('Ctrl Pts',(-38.9999999999987,42.799063541628,14.5581877930259));
#42681=CARTESIAN_POINT('Ctrl Pts',(-39.,42.8199489247508,14.5292256761601));
#42682=CARTESIAN_POINT('Origin',(-29.,20.7255401693197,-2.54750793782168));
#42683=CARTESIAN_POINT('Origin',(-29.,39.9592920728172,13.6255430020507));
#42684=CARTESIAN_POINT('Origin',(-29.,39.9592920728172,13.6255430020507));
#42685=CARTESIAN_POINT('Ctrl Pts',(-39.,38.3487778137292,16.1565988728829));
#42686=CARTESIAN_POINT('Ctrl Pts',(-39.,38.6171968569105,15.7347562277442));
#42687=CARTESIAN_POINT('Ctrl Pts',(-38.5,38.6171968569105,15.7347562277442));
#42688=CARTESIAN_POINT('Ctrl Pts',(-39.,38.4092369437272,16.1719014080264));
#42689=CARTESIAN_POINT('Ctrl Pts',(-38.980823569418,38.6554271426563,15.7590822228985));
#42690=CARTESIAN_POINT('Ctrl Pts',(-38.5000000151735,38.6721878607891,15.7697470775665));
#42691=CARTESIAN_POINT('Ctrl Pts',(-39.0022066208479,38.4705387441827,16.1854365781618));
#42692=CARTESIAN_POINT('Ctrl Pts',(-38.9652824568155,38.6979594886938,15.7849088143478));
#42693=CARTESIAN_POINT('Ctrl Pts',(-38.5044132464344,38.7278946093028,15.8021803250113));
#42694=CARTESIAN_POINT('Ctrl Pts',(-39.0100591075842,38.5948935550188,16.2091550083072));
#42695=CARTESIAN_POINT('Ctrl Pts',(-38.9423369615246,38.7893660665278,15.8361963875558));
#42696=CARTESIAN_POINT('Ctrl Pts',(-38.5201182104299,38.8407910464338,15.862291803958));
#42697=CARTESIAN_POINT('Ctrl Pts',(-39.0157123318516,38.6579464072813,16.2193371773267));
#42698=CARTESIAN_POINT('Ctrl Pts',(-38.9346328775752,38.8380714599669,15.8617024126807));
#42699=CARTESIAN_POINT('Ctrl Pts',(-38.5314246665614,38.8979816898257,15.889968907025));
#42700=CARTESIAN_POINT('Ctrl Pts',(-39.0263255453171,38.7538958038527,16.2321521976088));
#42701=CARTESIAN_POINT('Ctrl Pts',(-38.9285245106867,38.9156894504658,15.8987113268976));
#42702=CARTESIAN_POINT('Ctrl Pts',(-38.552651089205,38.9849222243469,15.9280643375507));
#42703=CARTESIAN_POINT('Ctrl Pts',(-39.0302209975595,38.7861074080575,16.2360134467896));
#42704=CARTESIAN_POINT('Ctrl Pts',(-38.9273730528816,38.9419920323425,15.9107120496548));
#42705=CARTESIAN_POINT('Ctrl Pts',(-38.5604419961988,39.014094844236,15.9401916617479));
#42706=CARTESIAN_POINT('Ctrl Pts',(-39.0365593216218,38.8347761200192,16.2411909269361));
#42707=CARTESIAN_POINT('Ctrl Pts',(-38.926916498768,38.9824990285064,15.9282925111225));
#42708=CARTESIAN_POINT('Ctrl Pts',(-38.5731186427039,39.0581480726366,15.9575354003289));
#42709=CARTESIAN_POINT('Ctrl Pts',(-39.0387547109622,38.8510575870985,16.2428143168919));
#42710=CARTESIAN_POINT('Ctrl Pts',(-38.9269719591409,38.996098050178,15.9340518299393));
#42711=CARTESIAN_POINT('Ctrl Pts',(-38.5775094223885,39.0728815372267,15.9631753814703));
#42712=CARTESIAN_POINT('Ctrl Pts',(-39.0433047957933,38.8837392435521,16.2458559814884));
#42713=CARTESIAN_POINT('Ctrl Pts',(-38.9274916449469,39.0235836684596,15.9453934327693));
#42714=CARTESIAN_POINT('Ctrl Pts',(-38.5866095911227,39.1024475967202,15.974173735627));
#42715=CARTESIAN_POINT('Ctrl Pts',(-39.0456604581885,38.9001445728115,16.2472743428312));
#42716=CARTESIAN_POINT('Ctrl Pts',(-38.9279536908748,39.0374749842454,15.9509793016801));
#42717=CARTESIAN_POINT('Ctrl Pts',(-38.5913209172013,39.1172848256198,15.9795332562622));
#42718=CARTESIAN_POINT('Ctrl Pts',(-39.0577588926345,38.9820478095945,16.2538213531667));
#42719=CARTESIAN_POINT('Ctrl Pts',(-38.9311989887487,39.1065119074279,15.9779967532242));
#42720=CARTESIAN_POINT('Ctrl Pts',(-38.6155177819721,39.1913378193784,16.0054983387571));
#42721=CARTESIAN_POINT('Ctrl Pts',(-39.0685011882335,39.0475167766825,16.2573537678501));
#42722=CARTESIAN_POINT('Ctrl Pts',(-38.9368284508843,39.1637208151416,15.9980737874138));
#42723=CARTESIAN_POINT('Ctrl Pts',(-38.6370023785226,39.2504632591108,16.023731083591));
#42724=CARTESIAN_POINT('Ctrl Pts',(-39.0917031721878,39.1785489807647,16.2612279974249));
#42725=CARTESIAN_POINT('Ctrl Pts',(-38.9532556851884,39.2800486076852,16.0339478271421));
#42726=CARTESIAN_POINT('Ctrl Pts',(-38.6834063423228,39.3686401589,16.0555377917917));
#42727=CARTESIAN_POINT('Ctrl Pts',(-39.1041650341826,39.2441112482649,16.2615687035868));
#42728=CARTESIAN_POINT('Ctrl Pts',(-38.9639492185558,39.3392792527924,16.0499007448607));
#42729=CARTESIAN_POINT('Ctrl Pts',(-38.7083300695817,39.4276907175188,16.0691097647488));
#42730=CARTESIAN_POINT('Ctrl Pts',(-39.1305316819266,39.3754873980411,16.2591791424027));
#42731=CARTESIAN_POINT('Ctrl Pts',(-38.9895991647774,39.4591992883204,16.077319462873));
#42732=CARTESIAN_POINT('Ctrl Pts',(-38.7610633626365,39.5458304682011,16.091849557657));
#42733=CARTESIAN_POINT('Ctrl Pts',(-39.1444376463372,39.4413007162717,16.2564483268932));
#42734=CARTESIAN_POINT('Ctrl Pts',(-39.0044992158227,39.5200144384565,16.0889170126415));
#42735=CARTESIAN_POINT('Ctrl Pts',(-38.788875293315,39.6049191608988,16.1010163496788));
#42736=CARTESIAN_POINT('Ctrl Pts',(-39.1662329627039,39.5403130713378,16.2500841355454));
#42737=CARTESIAN_POINT('Ctrl Pts',(-39.0296343641317,39.6125124617173,16.1029069127551));
#42738=CARTESIAN_POINT('Ctrl Pts',(-38.8324659250876,39.6936473350033,16.1115679390035));
#42739=CARTESIAN_POINT('Ctrl Pts',(-39.1736546585605,39.573365815963,16.2475842217919));
#42740=CARTESIAN_POINT('Ctrl Pts',(-39.0384151694294,39.6433722346712,16.1069919063746));
#42741=CARTESIAN_POINT('Ctrl Pts',(-38.8473093173327,39.7232390985529,16.1145512192814));
#42742=CARTESIAN_POINT('Ctrl Pts',(-39.1850076898159,39.6230303975766,16.2432666365631));
#42743=CARTESIAN_POINT('Ctrl Pts',(-39.0522271030963,39.6899639296596,16.1122619149349));
#42744=CARTESIAN_POINT('Ctrl Pts',(-38.870015379526,39.7676576335643,16.1182317049812));
#42745=CARTESIAN_POINT('Ctrl Pts',(-39.1888288061771,39.6395995001247,16.2417327931191));
#42746=CARTESIAN_POINT('Ctrl Pts',(-39.0569232021872,39.7054992973109,16.1138724413908));
#42747=CARTESIAN_POINT('Ctrl Pts',(-38.8776576124367,39.7824689543885,16.1193260831334));
#42748=CARTESIAN_POINT('Ctrl Pts',(-39.1965424555779,39.6727682706908,16.2384754684783));
#42749=CARTESIAN_POINT('Ctrl Pts',(-39.0665111339059,39.7366371934134,16.1168033128481));
#42750=CARTESIAN_POINT('Ctrl Pts',(-38.8930849110734,39.8121030476287,16.1212504892313));
#42751=CARTESIAN_POINT('Ctrl Pts',(-39.2004373455104,39.6893776681015,16.236750752351));
#42752=CARTESIAN_POINT('Ctrl Pts',(-39.0714060895731,39.7522512961052,16.1181254827183));
#42753=CARTESIAN_POINT('Ctrl Pts',(-38.9008746912715,39.8269344881269,16.1220806833524));
#42754=CARTESIAN_POINT('Ctrl Pts',(-39.2200079994996,39.7721810916385,16.2276889454715));
#42755=CARTESIAN_POINT('Ctrl Pts',(-39.0961105529348,39.8297324800265,16.1239513118732));
#42756=CARTESIAN_POINT('Ctrl Pts',(-38.9400159979962,39.9008330908001,16.1255600695062));
#42757=CARTESIAN_POINT('Ctrl Pts',(-39.2360252362298,39.8378839411281,16.2190184073814));
#42758=CARTESIAN_POINT('Ctrl Pts',(-39.1172505217682,39.8919360102205,16.1263051483739));
#42759=CARTESIAN_POINT('Ctrl Pts',(-38.9720506860607,39.9593391861364,16.126215419867));
#42760=CARTESIAN_POINT('Ctrl Pts',(-39.2523321837305,39.9031533327047,16.2089890418516));
#42761=CARTESIAN_POINT('Ctrl Pts',(-39.1394785380589,39.9541421330884,16.1263360633587));
#42762=CARTESIAN_POINT('Ctrl Pts',(-39.0046643674609,40.0173110104085,16.1248696719522));
#42763=CARTESIAN_POINT('',(-39.0936699647309,39.1876203501825,16.2608089943257));
#42764=CARTESIAN_POINT('Ctrl Pts',(-39.0936699647318,39.187620350183,16.2608089943268));
#42765=CARTESIAN_POINT('Ctrl Pts',(-39.0935222711613,39.1896732804381,16.2600676057615));
#42766=CARTESIAN_POINT('Ctrl Pts',(-39.0933711189158,39.1917268197941,16.2593286228811));
#42767=CARTESIAN_POINT('Ctrl Pts',(-39.0932165432533,39.1937809620199,16.2585920211916));
#42768=CARTESIAN_POINT('Ctrl Pts',(-39.0930619675907,39.1958351042458,16.2578554195021));
#42769=CARTESIAN_POINT('Ctrl Pts',(-39.092903426222,39.1979084188697,16.2571158289587));
#42770=CARTESIAN_POINT('Ctrl Pts',(-39.0927422452511,39.1999780775388,16.2563808711829));
#42771=CARTESIAN_POINT('Ctrl Pts',(-39.0924198833093,39.2041173948769,16.2549109556315));
#42772=CARTESIAN_POINT('Ctrl Pts',(-39.0920858400397,39.2082587537971,16.2534536804623));
#42773=CARTESIAN_POINT('Ctrl Pts',(-39.0917405120476,39.2124021988525,16.2520090278225));
#42774=CARTESIAN_POINT('Ctrl Pts',(-39.0913590487798,39.2169792158534,16.2504132060838));
#42775=CARTESIAN_POINT('Ctrl Pts',(-39.0909638345645,39.2215588916347,16.2488327920271));
#42776=CARTESIAN_POINT('Ctrl Pts',(-39.0905552639041,39.2261405355601,16.2472677592867));
#42777=CARTESIAN_POINT('Ctrl Pts',(-39.0902240994565,39.2298541589952,16.24599923158));
#42778=CARTESIAN_POINT('Ctrl Pts',(-39.0898844110932,39.2335707729552,16.2447408596389));
#42779=CARTESIAN_POINT('Ctrl Pts',(-39.0895361673382,39.2372882900436,16.2434925788529));
#42780=CARTESIAN_POINT('Ctrl Pts',(-39.0886541452664,39.2467039136605,16.240330968087));
#42781=CARTESIAN_POINT('Ctrl Pts',(-39.0877185869797,39.2561331757771,16.2372343338719));
#42782=CARTESIAN_POINT('Ctrl Pts',(-39.086733089636,39.2655732066824,16.2342025468132));
#42783=CARTESIAN_POINT('Ctrl Pts',(-39.0859802984598,39.2727841565797,16.2318866577235));
#42784=CARTESIAN_POINT('Ctrl Pts',(-39.0851976546674,39.2799960143386,16.2296084227804));
#42785=CARTESIAN_POINT('Ctrl Pts',(-39.0843887635932,39.2872199202528,16.227368365464));
#42786=CARTESIAN_POINT('Ctrl Pts',(-39.0821852989432,39.3068982450882,16.2212663237091));
#42787=CARTESIAN_POINT('Ctrl Pts',(-39.0797811657753,39.3266296736303,16.2154445797335));
#42788=CARTESIAN_POINT('Ctrl Pts',(-39.0772180387328,39.3464197777051,16.2099084657454));
#42789=CARTESIAN_POINT('Ctrl Pts',(-39.0754357491048,39.3601809751188,16.2060588873295));
#42790=CARTESIAN_POINT('Ctrl Pts',(-39.0735764432121,39.3739705906881,16.2023472616272));
#42791=CARTESIAN_POINT('Ctrl Pts',(-39.0716534468229,39.3877906531785,16.1987731088965));
#42792=CARTESIAN_POINT('Ctrl Pts',(-39.0697077670658,39.4017737349879,16.1951567960131));
#42793=CARTESIAN_POINT('Ctrl Pts',(-39.0676967956697,39.4157878636927,16.1916811593399));
#42794=CARTESIAN_POINT('Ctrl Pts',(-39.0656363274421,39.4298353024344,16.1883485708264));
#42795=CARTESIAN_POINT('Ctrl Pts',(-39.0627317165124,39.4496377645914,16.1836506711497));
#42796=CARTESIAN_POINT('Ctrl Pts',(-39.0597289039457,39.4695066940188,16.1792373046652));
#42797=CARTESIAN_POINT('Ctrl Pts',(-39.0566705585344,39.4894474076504,16.1751065688499));
#42798=CARTESIAN_POINT('Ctrl Pts',(-39.0553071680152,39.4983368482646,16.1732651136541));
#42799=CARTESIAN_POINT('Ctrl Pts',(-39.0539328325859,39.5072405288181,16.1714799449962));
#42800=CARTESIAN_POINT('Ctrl Pts',(-39.0525528681501,39.5161521790931,16.1697524675246));
#42801=CARTESIAN_POINT('Ctrl Pts',(-39.0512871217776,39.5243262223628,16.1681679713691));
#42802=CARTESIAN_POINT('Ctrl Pts',(-39.0500165629401,39.5325070881124,16.1666320070914));
#42803=CARTESIAN_POINT('Ctrl Pts',(-39.0487453928414,39.540689545901,16.165145081683));
#42804=CARTESIAN_POINT('Ctrl Pts',(-39.0460883451561,39.5577928277904,16.1620370541116));
#42805=CARTESIAN_POINT('Ctrl Pts',(-39.0434267036561,39.574915257398,16.1591411118856));
#42806=CARTESIAN_POINT('Ctrl Pts',(-39.0407917137069,39.5920596775563,16.1564516597163));
#42807=CARTESIAN_POINT('Ctrl Pts',(-39.0365649129289,39.6195611291217,16.1521374958141));
#42808=CARTESIAN_POINT('Ctrl Pts',(-39.0324051221603,39.6471188125438,16.1483543509625));
#42809=CARTESIAN_POINT('Ctrl Pts',(-39.0284495518797,39.6747449792293,16.1450705587353));
#42810=CARTESIAN_POINT('Ctrl Pts',(-39.0274733127469,39.6815631478105,16.1442601151711));
#42811=CARTESIAN_POINT('Ctrl Pts',(-39.0265094328012,39.6883854420688,16.143479855215));
#42812=CARTESIAN_POINT('Ctrl Pts',(-39.0255598220946,39.6952119531012,16.1427288579772));
#42813=CARTESIAN_POINT('Ctrl Pts',(-39.0253702851041,39.6965744865557,16.1425789631253));
#42814=CARTESIAN_POINT('Ctrl Pts',(-39.025181313738,39.6979371831495,16.1424302302673));
#42815=CARTESIAN_POINT('Ctrl Pts',(-39.024992926915,39.6993000467681,16.1422826560201));
#42816=CARTESIAN_POINT('Ctrl Pts',(-39.0214262186056,39.7251030032366,16.1394886480019));
#42817=CARTESIAN_POINT('Ctrl Pts',(-39.0180708061177,39.7509672726913,16.1371132295503));
#42818=CARTESIAN_POINT('Ctrl Pts',(-39.0150463870856,39.7769022070589,16.135109441488));
#42819=CARTESIAN_POINT('Ctrl Pts',(-39.0141873375696,39.7842687103705,16.1345402898107));
#42820=CARTESIAN_POINT('Ctrl Pts',(-39.0133548629673,39.7916408279094,16.1340008353982));
#42821=CARTESIAN_POINT('Ctrl Pts',(-39.0125513944238,39.7990185563883,16.1334893473139));
#42822=CARTESIAN_POINT('Ctrl Pts',(-39.0099373559885,39.8230215692805,16.1318252504152));
#42823=CARTESIAN_POINT('Ctrl Pts',(-39.0076304951035,39.8470819631763,16.1304589284462));
#42824=CARTESIAN_POINT('Ctrl Pts',(-39.005733443495,39.871213035224,16.1293377024353));
#42825=CARTESIAN_POINT('Ctrl Pts',(-39.004959266345,39.8810608034669,16.1288801357809));
#42826=CARTESIAN_POINT('Ctrl Pts',(-39.0042530766643,39.8909201437646,16.128462873272));
#42827=CARTESIAN_POINT('Ctrl Pts',(-39.0036206852641,39.9007910684579,16.1280803373666));
#42828=CARTESIAN_POINT('Ctrl Pts',(-39.0035609301979,39.9017237784193,16.1280441913052));
#42829=CARTESIAN_POINT('Ctrl Pts',(-39.0035018335811,39.9026565289322,16.1280083528885));
#42830=CARTESIAN_POINT('Ctrl Pts',(-39.0034433999712,39.9035893197067,16.1279728172578));
#42831=CARTESIAN_POINT('Ctrl Pts',(-39.0023473053679,39.9210865603477,16.1273062417523));
#42832=CARTESIAN_POINT('Ctrl Pts',(-39.0014873834615,39.9386193782255,16.1267495520393));
#42833=CARTESIAN_POINT('Ctrl Pts',(-39.0009007469202,39.9561889486819,16.1262726075685));
#42834=CARTESIAN_POINT('Ctrl Pts',(-39.0006074286495,39.9649737339102,16.1260341353331));
#42835=CARTESIAN_POINT('Ctrl Pts',(-39.0003824779079,39.9737677102205,16.1258155565433));
#42836=CARTESIAN_POINT('Ctrl Pts',(-39.0002308110869,39.9825710305249,16.1256127882412));
#42837=CARTESIAN_POINT('Ctrl Pts',(-39.0001549776764,39.9869726906771,16.1255114040901));
#42838=CARTESIAN_POINT('Ctrl Pts',(-39.0000974681329,39.9913766867925,16.1254139687993));
#42839=CARTESIAN_POINT('Ctrl Pts',(-39.0000589140448,39.995783037166,16.1253199473816));
#42840=CARTESIAN_POINT('Ctrl Pts',(-39.0000396370008,39.9979862123527,16.1252729366727));
#42841=CARTESIAN_POINT('Ctrl Pts',(-39.0000250989958,40.0001899760904,16.1252267791589));
#42842=CARTESIAN_POINT('Ctrl Pts',(-39.000015380015,40.0023943305614,16.1251814062609));
#42843=CARTESIAN_POINT('Ctrl Pts',(-39.0000105205245,40.0034965077969,16.1251587198119));
#42844=CARTESIAN_POINT('Ctrl Pts',(-39.0000068658008,40.0045988327145,16.1251362294985));
#42845=CARTESIAN_POINT('Ctrl Pts',(-39.0000044259056,40.0057013055785,16.1251139266363));
#42846=CARTESIAN_POINT('Ctrl Pts',(-39.0000019860103,40.0068037784424,16.125091623774));
#42847=CARTESIAN_POINT('Ctrl Pts',(-39.0000007609435,40.0079063992528,16.125069508363));
#42848=CARTESIAN_POINT('Ctrl Pts',(-39.0000007608086,40.0090091682675,16.125047571642));
#42849=CARTESIAN_POINT('Ctrl Pts',(-39.,38.3487778137292,16.1565988728829));
#42850=CARTESIAN_POINT('Ctrl Pts',(-39.,38.3833934352842,16.1653602760744));
#42851=CARTESIAN_POINT('Ctrl Pts',(-39.0007271289037,38.418056230505,16.1734834106599));
#42852=CARTESIAN_POINT('Ctrl Pts',(-39.0033844025761,38.4874821615589,16.1885397585578));
#42853=CARTESIAN_POINT('Ctrl Pts',(-39.0053154013728,38.5222452565794,16.1954728002341));
#42854=CARTESIAN_POINT('Ctrl Pts',(-39.0126341194485,38.6266906398611,16.2145895490314));
#42855=CARTESIAN_POINT('Ctrl Pts',(-39.0195339780508,38.6965293017166,16.2250958545813));
#42856=CARTESIAN_POINT('Ctrl Pts',(-39.0321447527579,38.8016129939812,16.2377952286948));
#42857=CARTESIAN_POINT('Ctrl Pts',(-39.0367291513417,38.8366950810595,16.2415169611478));
#42858=CARTESIAN_POINT('Ctrl Pts',(-39.0441085920868,38.8894005968051,16.2463592266313));
#42859=CARTESIAN_POINT('Ctrl Pts',(-39.0466519979229,38.9069797098678,16.2478494670046));
#42860=CARTESIAN_POINT('Ctrl Pts',(-39.0518885060209,38.9421114193367,16.2505832282473));
#42861=CARTESIAN_POINT('Ctrl Pts',(-39.065360489734,39.029907703484,16.2568029716959));
#42862=CARTESIAN_POINT('Ctrl Pts',(-39.0805958020047,39.1175586211149,16.260024347864));
#42863=CARTESIAN_POINT('Ctrl Pts',(-39.0936699647319,39.1876203501829,16.2608089943269));
#42864=CARTESIAN_POINT('Origin',(-39.5,34.999999994595,6.54998265276524E-10));
#42865=CARTESIAN_POINT('Origin',(-39.,34.999999994595,6.54998265276524E-10));
#42866=CARTESIAN_POINT('Origin',(-39.5,42.1186371575735,14.8853956938121));
#42867=CARTESIAN_POINT('Origin',(-39.5,34.999999994595,6.54998265276524E-10));
#42868=CARTESIAN_POINT('',(-39.,18.5084035288379,-0.52654155575758));
#42869=CARTESIAN_POINT('Ctrl Pts',(-39.5,18.2644264063412,-2.98673344445558));
#42870=CARTESIAN_POINT('Ctrl Pts',(-39.4982565645427,18.2632940298282,-2.98038839532042));
#42871=CARTESIAN_POINT('Ctrl Pts',(-39.4965117602025,18.2621733491251,-2.97403614595641));
#42872=CARTESIAN_POINT('Ctrl Pts',(-39.4947636361374,18.2610631637812,-2.96766936765203));
#42873=CARTESIAN_POINT('Ctrl Pts',(-39.4930155120723,18.2599529784372,-2.96130258934765));
#42874=CARTESIAN_POINT('Ctrl Pts',(-39.4912678321557,18.2588557079406,-2.95493499688772));
#42875=CARTESIAN_POINT('Ctrl Pts',(-39.4895206393129,18.2577713218828,-2.94856658238146));
#42876=CARTESIAN_POINT('Ctrl Pts',(-39.4860262536273,18.2556025497672,-2.93582975336894));
#42877=CARTESIAN_POINT('Ctrl Pts',(-39.4825338167734,18.2534853302707,-2.92308963332142));
#42878=CARTESIAN_POINT('Ctrl Pts',(-39.4790436750457,18.2514195389397,-2.91034613927784));
#42879=CARTESIAN_POINT('Ctrl Pts',(-39.4720633915901,18.2472879562777,-2.88485915119069));
#42880=CARTESIAN_POINT('Ctrl Pts',(-39.4650922877873,18.2433620564643,-2.85935867096065));
#42881=CARTESIAN_POINT('Ctrl Pts',(-39.4581331343936,18.2396411072223,-2.83384400738141));
#42882=CARTESIAN_POINT('Ctrl Pts',(-39.4442148276061,18.2321992087383,-2.78281468022295));
#42883=CARTESIAN_POINT('Ctrl Pts',(-39.4303442716327,18.2255766539551,-2.73172870279065));
#42884=CARTESIAN_POINT('Ctrl Pts',(-39.4165440806474,18.2197717559618,-2.68058028152748));
#42885=CARTESIAN_POINT('Ctrl Pts',(-39.3889436986768,18.2081619599752,-2.57828343900114));
#42886=CARTESIAN_POINT('Ctrl Pts',(-39.3616221749354,18.1998153193335,-2.47573793659964));
#42887=CARTESIAN_POINT('Ctrl Pts',(-39.3347784476018,18.1947856738467,-2.37288927501648));
#42888=CARTESIAN_POINT('Ctrl Pts',(-39.3335875496944,18.1945625381319,-2.368326486312));
#42889=CARTESIAN_POINT('Ctrl Pts',(-39.3323975904841,18.1943459235456,-2.36376309599717));
#42890=CARTESIAN_POINT('Ctrl Pts',(-39.331208587611,18.1941358327567,-2.35919910078715));
#42891=CARTESIAN_POINT('Ctrl Pts',(-39.3055965786381,18.1896103204193,-2.26088723887917));
#42892=CARTESIAN_POINT('Ctrl Pts',(-39.2804265332853,18.1881140973325,-2.16229734459659));
#42893=CARTESIAN_POINT('Ctrl Pts',(-39.2559179426822,18.1897840045728,-2.06336481042167));
#42894=CARTESIAN_POINT('Ctrl Pts',(-39.2543480339218,18.1898909712298,-2.05702764258509));
#42895=CARTESIAN_POINT('Ctrl Pts',(-39.2527808346664,18.1900109130978,-2.05068906626546));
#42896=CARTESIAN_POINT('Ctrl Pts',(-39.2512164033361,18.1901438593256,-2.04434907378134));
#42897=CARTESIAN_POINT('Ctrl Pts',(-39.2400023905221,18.1910968322516,-1.99890332261146));
#42898=CARTESIAN_POINT('Ctrl Pts',(-39.2289314687727,18.1927201844435,-1.95338409824031));
#42899=CARTESIAN_POINT('Ctrl Pts',(-39.2180308629908,18.1950353121287,-1.9077834153972));
#42900=CARTESIAN_POINT('Ctrl Pts',(-39.2162879759569,18.1954054755953,-1.90049236749997));
#42901=CARTESIAN_POINT('Ctrl Pts',(-39.2145494600503,18.1957933142013,-1.89319931660478));
#42902=CARTESIAN_POINT('Ctrl Pts',(-39.2128154190889,18.1961989089874,-1.8859042096267));
#42903=CARTESIAN_POINT('Ctrl Pts',(-39.2096666341135,18.1969354145239,-1.8726572773113));
#42904=CARTESIAN_POINT('Ctrl Pts',(-39.2065326463223,18.1977305429674,-1.85940352639851));
#42905=CARTESIAN_POINT('Ctrl Pts',(-39.2034141624684,18.1985849209553,-1.84614255750622));
#42906=CARTESIAN_POINT('Ctrl Pts',(-39.2021303279584,18.1989366559641,-1.84068320921452));
#42907=CARTESIAN_POINT('Ctrl Pts',(-39.2008487219748,18.1992985676539,-1.83522091067537));
#42908=CARTESIAN_POINT('Ctrl Pts',(-39.1995701568081,18.1996704526564,-1.82975891490213));
#42909=CARTESIAN_POINT('Ctrl Pts',(-39.1977421510071,18.2002021486229,-1.82194972361643));
#42910=CARTESIAN_POINT('Ctrl Pts',(-39.1959192655843,18.2007545485336,-1.81413647416283));
#42911=CARTESIAN_POINT('Ctrl Pts',(-39.1941037111139,18.2013271931799,-1.80632787186134));
#42912=CARTESIAN_POINT('Ctrl Pts',(-39.1898662232147,18.2026637406637,-1.78810266391492));
#42913=CARTESIAN_POINT('Ctrl Pts',(-39.1856666064574,18.2041108748653,-1.76989434449253));
#42914=CARTESIAN_POINT('Ctrl Pts',(-39.1815045041788,18.2056702971502,-1.75169250579292));
#42915=CARTESIAN_POINT('Ctrl Pts',(-39.1796210579155,18.2063759713213,-1.74345575840182));
#42916=CARTESIAN_POINT('Ctrl Pts',(-39.1777454922288,18.2071045751166,-1.7352212012678));
#42917=CARTESIAN_POINT('Ctrl Pts',(-39.1758779937713,18.2078561914943,-1.72698881253716));
#42918=CARTESIAN_POINT('Ctrl Pts',(-39.1541654270963,18.2165948978911,-1.63127452238991));
#42919=CARTESIAN_POINT('Ctrl Pts',(-39.133529694962,18.2284326450439,-1.53585516105736));
#42920=CARTESIAN_POINT('Ctrl Pts',(-39.1143518851541,18.2435811130114,-1.44068967460049));
#42921=CARTESIAN_POINT('Ctrl Pts',(-39.1125541406822,18.2450011434956,-1.43176877962281));
#42922=CARTESIAN_POINT('Ctrl Pts',(-39.1107692087929,18.2464502566782,-1.42285010476126));
#42923=CARTESIAN_POINT('Ctrl Pts',(-39.1089974104922,18.2479286136716,-1.41393362056419));
#42924=CARTESIAN_POINT('Ctrl Pts',(-39.1005058581712,18.2550138139192,-1.37120031844464));
#42925=CARTESIAN_POINT('Ctrl Pts',(-39.0923179063329,18.2627729609616,-1.32851751678849));
#42926=CARTESIAN_POINT('Ctrl Pts',(-39.0844832261953,18.271236307921,-1.28588020640277));
#42927=CARTESIAN_POINT('Ctrl Pts',(-39.0828756161155,18.2729729151138,-1.27713139103993));
#42928=CARTESIAN_POINT('Ctrl Pts',(-39.0812828770768,18.2747391740245,-1.26838447431847));
#42929=CARTESIAN_POINT('Ctrl Pts',(-39.0797054438143,18.276535337416,-1.25963942990192));
#42930=CARTESIAN_POINT('Ctrl Pts',(-39.0719912104367,18.2853192422034,-1.2168729210884));
#42931=CARTESIAN_POINT('Ctrl Pts',(-39.064642510105,18.2948181395909,-1.17415144094987));
#42932=CARTESIAN_POINT('Ctrl Pts',(-39.0577257707355,18.3050731128552,-1.1314683987587));
#42933=CARTESIAN_POINT('Ctrl Pts',(-39.0563799319872,18.30706849531,-1.1231632582857));
#42934=CARTESIAN_POINT('Ctrl Pts',(-39.0550503898463,18.3090925886837,-1.11485922024422));
#42935=CARTESIAN_POINT('Ctrl Pts',(-39.053737708826,18.3111455823682,-1.10655668676609));
#42936=CARTESIAN_POINT('Ctrl Pts',(-39.0517286769875,18.3142876478149,-1.09384982665325));
#42937=CARTESIAN_POINT('Ctrl Pts',(-39.0497593032948,18.3174975330194,-1.08114645633668));
#42938=CARTESIAN_POINT('Ctrl Pts',(-39.0478319313426,18.3207761133243,-1.06844792063594));
#42939=CARTESIAN_POINT('Ctrl Pts',(-39.0471208500752,18.3219857070594,-1.0637629448841));
#42940=CARTESIAN_POINT('Ctrl Pts',(-39.0464152375459,18.323205119103,-1.05907690212186));
#42941=CARTESIAN_POINT('Ctrl Pts',(-39.0457155529325,18.3244337666235,-1.05439218017061));
#42942=CARTESIAN_POINT('Ctrl Pts',(-39.044520955394,18.3265314821878,-1.04639378031453));
#42943=CARTESIAN_POINT('Ctrl Pts',(-39.0433430534469,18.3286571222814,-1.03839536818302));
#42944=CARTESIAN_POINT('Ctrl Pts',(-39.0421834943012,18.330809197905,-1.03040397925429));
#42945=CARTESIAN_POINT('Ctrl Pts',(-39.0414816456199,18.3321117890182,-1.02556701530778));
#42946=CARTESIAN_POINT('Ctrl Pts',(-39.040786633438,18.333423792319,-1.0207335461338));
#42947=CARTESIAN_POINT('Ctrl Pts',(-39.0400984395507,18.3347455178494,-1.01590260391144));
#42948=CARTESIAN_POINT('Ctrl Pts',(-39.0382732462829,18.3382509319266,-1.00309022155061));
#42949=CARTESIAN_POINT('Ctrl Pts',(-39.0364962908506,18.3418242089596,-0.990297549473336));
#42950=CARTESIAN_POINT('Ctrl Pts',(-39.0347699154051,18.3454662563153,-0.977524706607762));
#42951=CARTESIAN_POINT('Ctrl Pts',(-39.0337567600377,18.3476036591823,-0.970028727480062));
#42952=CARTESIAN_POINT('Ctrl Pts',(-39.0327610270135,18.3497647464099,-0.962539592535702));
#42953=CARTESIAN_POINT('Ctrl Pts',(-39.0317831970767,18.3519497059365,-0.955057313744942));
#42954=CARTESIAN_POINT('Ctrl Pts',(-39.0260962976061,18.3646570742702,-0.911541600336059));
#42955=CARTESIAN_POINT('Ctrl Pts',(-39.0210121201334,18.3781709589092,-0.868257443629536));
#42956=CARTESIAN_POINT('Ctrl Pts',(-39.0166488781946,18.3925369729867,-0.825211111031793));
#42957=CARTESIAN_POINT('Ctrl Pts',(-39.0160595867312,18.3944772205315,-0.819397352206009));
#42958=CARTESIAN_POINT('Ctrl Pts',(-39.0154834597696,18.3964330177636,-0.813587937240513));
#42959=CARTESIAN_POINT('Ctrl Pts',(-39.0149208018372,18.3984044833367,-0.807782873087525));
#42960=CARTESIAN_POINT('Ctrl Pts',(-39.010601091197,18.4135400751802,-0.763215479751383));
#42961=CARTESIAN_POINT('Ctrl Pts',(-39.0070725985321,18.4295985556218,-0.718904554302151));
#42962=CARTESIAN_POINT('Ctrl Pts',(-39.004522940544,18.446649756052,-0.674858878290108));
#42963=CARTESIAN_POINT('Ctrl Pts',(-39.0043320691178,18.4479262358618,-0.671561549379601));
#42964=CARTESIAN_POINT('Ctrl Pts',(-39.0041466913404,18.4492082820768,-0.668265708929566));
#42965=CARTESIAN_POINT('Ctrl Pts',(-39.0039668898115,18.4504959258862,-0.66497135916845));
#42966=CARTESIAN_POINT('Ctrl Pts',(-39.001432063524,18.4686490161198,-0.618527903270653));
#42967=CARTESIAN_POINT('Ctrl Pts',(-39.,18.4879134182867,-0.572380484667404));
#42968=CARTESIAN_POINT('Ctrl Pts',(-39.,18.5084035288379,-0.52654155575758));
#42969=CARTESIAN_POINT('Origin',(-39.,34.999999994595,6.54998265276524E-10));
#42970=CARTESIAN_POINT('Origin',(-39.5,39.1149554701578,15.978646421242));
#42971=CARTESIAN_POINT('Origin',(-38.5,20.7255401693197,-2.54750793782168));
#42972=CARTESIAN_POINT('',(-39.,19.7255401693197,0.28091918692451));
#42973=CARTESIAN_POINT('Ctrl Pts',(-38.5,20.2255401693197,-0.0980181950385015));
#42974=CARTESIAN_POINT('Ctrl Pts',(-38.5068454246389,20.2255401693197,-0.0980181950385014));
#42975=CARTESIAN_POINT('Ctrl Pts',(-38.5137049378611,20.2253995984199,-0.0979034111946665));
#42976=CARTESIAN_POINT('Ctrl Pts',(-38.574487053383,20.2228963259888,-0.0958597862843734));
#42977=CARTESIAN_POINT('Ctrl Pts',(-38.6266179130002,20.2120282571218,-0.0869664209613772));
#42978=CARTESIAN_POINT('Ctrl Pts',(-38.7343668418878,20.1716895730688,-0.0543730508899982));
#42979=CARTESIAN_POINT('Ctrl Pts',(-38.7864380337499,20.1394945590217,-0.0285603789798399));
#42980=CARTESIAN_POINT('Ctrl Pts',(-38.8850764070749,20.0527224260415,0.0395179277114487));
#42981=CARTESIAN_POINT('Ctrl Pts',(-38.9288507671718,19.9929196181174,0.0855519592453916));
#42982=CARTESIAN_POINT('Ctrl Pts',(-38.9855092027928,19.863098833122,0.182314659292735));
#42983=CARTESIAN_POINT('Ctrl Pts',(-38.9995659056513,19.7961082948418,0.230981573726129));
#42984=CARTESIAN_POINT('Ctrl Pts',(-38.9999967004912,19.7276374941665,0.279435862662001));
#42985=CARTESIAN_POINT('Ctrl Pts',(-39.,19.7265889001319,0.280177622255819));
#42986=CARTESIAN_POINT('Ctrl Pts',(-39.,19.7255401693201,0.28091918692451));
#42987=CARTESIAN_POINT('Origin',(-39.,20.7255401693197,-2.54750793782168));
#42988=CARTESIAN_POINT('Origin',(-38.5,18.5084035288379,-0.52654155575758));
#42989=CARTESIAN_POINT('Ctrl Pts',(-38.5,18.8779263022516,-0.863369286101596));
#42990=CARTESIAN_POINT('Ctrl Pts',(-39.,18.8779263022516,-0.863369286101596));
#42991=CARTESIAN_POINT('Ctrl Pts',(-39.,18.5084035288379,-0.526541555757579));
#42992=CARTESIAN_POINT('Ctrl Pts',(-38.5000000121044,18.8428991572258,-0.901796430331833));
#42993=CARTESIAN_POINT('Ctrl Pts',(-38.9846448633454,18.8534834999705,-0.890184678462895));
#42994=CARTESIAN_POINT('Ctrl Pts',(-39.,18.4881009996417,-0.571960841817054));
#42995=CARTESIAN_POINT('Ctrl Pts',(-38.5028175697433,18.8093997703974,-0.940951127436968));
#42996=CARTESIAN_POINT('Ctrl Pts',(-38.9716161398923,18.8276179047806,-0.919547640497487));
#42997=CARTESIAN_POINT('Ctrl Pts',(-39.001408782789,18.4688157281884,-0.61810138075627));
#42998=CARTESIAN_POINT('Ctrl Pts',(-38.5130500106387,18.7452608184442,-1.02070981564836));
#42999=CARTESIAN_POINT('Ctrl Pts',(-38.9507774942834,18.7751212471768,-0.982362104350359));
#43000=CARTESIAN_POINT('Ctrl Pts',(-39.006525007402,18.4321760372884,-0.711841267055085));
#43001=CARTESIAN_POINT('Ctrl Pts',(-38.5204704459176,18.7146215389275,-1.06131431190728));
#43002=CARTESIAN_POINT('Ctrl Pts',(-38.9428107063041,18.7484926791068,-1.01571890599804));
#43003=CARTESIAN_POINT('Ctrl Pts',(-39.0102352215507,18.4148220173941,-0.759440668067828));
#43004=CARTESIAN_POINT('Ctrl Pts',(-38.5392127937583,18.6560779514862,-1.14397975473208));
#43005=CARTESIAN_POINT('Ctrl Pts',(-38.9317121494331,18.6955196203185,-1.08611448020077));
#43006=CARTESIAN_POINT('Ctrl Pts',(-39.0196063982873,18.3819868820653,-0.8561250274524));
#43007=CARTESIAN_POINT('Ctrl Pts',(-38.5505376800415,18.6281740998822,-1.18604062346602));
#43008=CARTESIAN_POINT('Ctrl Pts',(-38.9284460459492,18.6691391641143,-1.12309259491601));
#43009=CARTESIAN_POINT('Ctrl Pts',(-39.0252688391042,18.3665060238294,-0.905209872964393));
#43010=CARTESIAN_POINT('Ctrl Pts',(-38.5700807581267,18.5883170213382,-1.25023709676593));
#43011=CARTESIAN_POINT('Ctrl Pts',(-38.9268518414429,18.6301154171898,-1.18142532324));
#43012=CARTESIAN_POINT('Ctrl Pts',(-39.0350403795217,18.3446715373495,-0.979981027272348));
#43013=CARTESIAN_POINT('Ctrl Pts',(-38.5770224165533,18.5753648269077,-1.27182020968494));
#43014=CARTESIAN_POINT('Ctrl Pts',(-38.9268547426899,18.6173082485063,-1.20115921207614));
#43015=CARTESIAN_POINT('Ctrl Pts',(-39.0385112079161,18.3376247517694,-1.00509550606235));
#43016=CARTESIAN_POINT('Ctrl Pts',(-38.5880392751736,18.556433320345,-1.30447383795162));
#43017=CARTESIAN_POINT('Ctrl Pts',(-38.9276416963271,18.5982881776557,-1.23144666676493));
#43018=CARTESIAN_POINT('Ctrl Pts',(-39.0440196377671,18.3274014203209,-1.0430582153955));
#43019=CARTESIAN_POINT('Ctrl Pts',(-38.5918107280427,18.5502090235416,-1.31539948656175));
#43020=CARTESIAN_POINT('Ctrl Pts',(-38.9280311463852,18.5920097611487,-1.24160683011756));
#43021=CARTESIAN_POINT('Ctrl Pts',(-39.0459053636913,18.3240533247711,-1.05575467508082));
#43022=CARTESIAN_POINT('Ctrl Pts',(-38.5995170068257,18.537974590515,-1.33725438261636));
#43023=CARTESIAN_POINT('Ctrl Pts',(-38.9290567915728,18.5795930841744,-1.26203671753181));
#43024=CARTESIAN_POINT('Ctrl Pts',(-39.0497585037429,18.3174988913271,-1.08114115888948));
#43025=CARTESIAN_POINT('Ctrl Pts',(-38.6034554755142,18.5319580960745,-1.34819451677163));
#43026=CARTESIAN_POINT('Ctrl Pts',(-38.9296918352213,18.5734470765348,-1.2723168318538));
#43027=CARTESIAN_POINT('Ctrl Pts',(-39.0517277374561,18.3142891141038,-1.09384384268011));
#43028=CARTESIAN_POINT('Ctrl Pts',(-38.6235552691089,18.5023687406762,-1.4029605589706));
#43029=CARTESIAN_POINT('Ctrl Pts',(-38.9334287389161,18.5433014861436,-1.32359797225254));
#43030=CARTESIAN_POINT('Ctrl Pts',(-39.0617776357584,18.2985713692847,-1.15740800389106));
#43031=CARTESIAN_POINT('Ctrl Pts',(-38.6409338208112,18.4802721042523,-1.44698296900576));
#43032=CARTESIAN_POINT('Ctrl Pts',(-38.9382939320124,18.5199892666906,-1.36598545379934));
#43033=CARTESIAN_POINT('Ctrl Pts',(-39.0704669095817,18.2870548910152,-1.20842227191335));
#43034=CARTESIAN_POINT('Ctrl Pts',(-38.6778880423194,18.4390140339829,-1.53548910231471));
#43035=CARTESIAN_POINT('Ctrl Pts',(-38.9513053448041,18.4758073593947,-1.45244063995325));
#43036=CARTESIAN_POINT('Ctrl Pts',(-39.0889440219837,18.2660157117594,-1.31085653901257));
#43037=CARTESIAN_POINT('Ctrl Pts',(-38.6974651244877,18.4198532838473,-1.57997264774622));
#43038=CARTESIAN_POINT('Ctrl Pts',(-38.9593984641188,18.4548505882054,-1.4965504346942));
#43039=CARTESIAN_POINT('Ctrl Pts',(-39.0987325617014,18.2564934169457,-1.3622762904579));
#43040=CARTESIAN_POINT('Ctrl Pts',(-38.7590544808404,18.3665552095797,-1.71416757203857));
#43041=CARTESIAN_POINT('Ctrl Pts',(-38.9876508556077,18.3963878957642,-1.62990979111957));
#43042=CARTESIAN_POINT('Ctrl Pts',(-39.1295272415051,18.2307988288308,-1.51724815893203));
#43043=CARTESIAN_POINT('Ctrl Pts',(-38.8039018553468,18.3365825126792,-1.80462281697605));
#43044=CARTESIAN_POINT('Ctrl Pts',(-39.012095726413,18.3618241711421,-1.72283960130348));
#43045=CARTESIAN_POINT('Ctrl Pts',(-39.1519509272974,18.2174861530546,-1.62151228107335));
#43046=CARTESIAN_POINT('Ctrl Pts',(-38.863719532733,18.3056934244436,-1.91909402720029));
#43047=CARTESIAN_POINT('Ctrl Pts',(-39.0483420183347,18.3254434461637,-1.84301300206946));
#43048=CARTESIAN_POINT('Ctrl Pts',(-39.1818597664605,18.2054486954808,-1.7533579412421));
#43049=CARTESIAN_POINT('Ctrl Pts',(-38.8758729301451,18.2998460440467,-1.94205839310398));
#43050=CARTESIAN_POINT('Ctrl Pts',(-39.0557807395094,18.3185797826281,-1.86696003063784));
#43051=CARTESIAN_POINT('Ctrl Pts',(-39.187936465009,18.2032724058732,-1.779802873125));
#43052=CARTESIAN_POINT('Ctrl Pts',(-38.8943746691618,18.2915681837471,-1.97661332531131));
#43053=CARTESIAN_POINT('Ctrl Pts',(-39.0673289982722,18.3087953136981,-1.90315643956538));
#43054=CARTESIAN_POINT('Ctrl Pts',(-39.1971873346127,18.2003545864548,-1.81959037093966));
#43055=CARTESIAN_POINT('Ctrl Pts',(-38.9005893670775,18.2888903886097,-1.98815358276858));
#43056=CARTESIAN_POINT('Ctrl Pts',(-39.0712357141135,18.305624513315,-1.91524480475088));
#43057=CARTESIAN_POINT('Ctrl Pts',(-39.2002946834377,18.1994395715941,-1.83287735674673));
#43058=CARTESIAN_POINT('Ctrl Pts',(-38.9130672827963,18.2837149816403,-2.01119720590798));
#43059=CARTESIAN_POINT('Ctrl Pts',(-39.0791435396456,18.2994780043902,-1.93941653842486));
#43060=CARTESIAN_POINT('Ctrl Pts',(-39.2065336414992,18.1977302703166,-1.85940775826571));
#43061=CARTESIAN_POINT('Ctrl Pts',(-38.9193352153427,18.281215176572,-2.02270942842269));
#43062=CARTESIAN_POINT('Ctrl Pts',(-39.0831476831193,18.2964988066967,-1.95151041911247));
#43063=CARTESIAN_POINT('Ctrl Pts',(-39.2096676075802,18.1969351868286,-1.87266137268417));
#43064=CARTESIAN_POINT('Ctrl Pts',(-38.9508133295184,18.2691491038573,-2.08022508586583));
#43065=CARTESIAN_POINT('Ctrl Pts',(-39.1033178931505,18.2821373957891,-2.01174614075846));
#43066=CARTESIAN_POINT('Ctrl Pts',(-39.2254066651236,18.1932537976226,-1.9388755573968));
#43067=CARTESIAN_POINT('Ctrl Pts',(-38.9764375556006,18.2608798321247,-2.12609264637355));
#43068=CARTESIAN_POINT('Ctrl Pts',(-39.1202929972975,18.2720741420306,-2.06029596271023));
#43069=CARTESIAN_POINT('Ctrl Pts',(-39.2382187775668,18.1912484049181,-1.99167508271378));
#43070=CARTESIAN_POINT('Ctrl Pts',(-39.0544233622651,18.240018901072,-2.26334297249591));
#43071=CARTESIAN_POINT('Ctrl Pts',(-39.1728036049692,18.2464825605143,-2.20533681448651));
#43072=CARTESIAN_POINT('Ctrl Pts',(-39.2772116815981,18.1879347508401,-2.14969704063337));
#43073=CARTESIAN_POINT('Ctrl Pts',(-39.1078893586506,18.2313577128234,-2.35437654643091));
#43074=CARTESIAN_POINT('Ctrl Pts',(-39.2105403633043,18.2350636347238,-2.30311269780209));
#43075=CARTESIAN_POINT('Ctrl Pts',(-39.3039446791879,18.1893184331436,-2.25454639009119));
#43076=CARTESIAN_POINT('Ctrl Pts',(-39.2169451138417,18.2239187624629,-2.53583757407667));
#43077=CARTESIAN_POINT('Ctrl Pts',(-39.2890733295988,18.2238760787528,-2.49823411040255));
#43078=CARTESIAN_POINT('Ctrl Pts',(-39.3584725570583,18.1989532058266,-2.46385177983269));
#43079=CARTESIAN_POINT('Ctrl Pts',(-39.2725402949566,18.225144403491,-2.62626286641505));
#43080=CARTESIAN_POINT('Ctrl Pts',(-39.3300826313235,18.2239232442552,-2.59620144360494));
#43081=CARTESIAN_POINT('Ctrl Pts',(-39.3862701474838,18.2072061381291,-2.56830453161861));
#43082=CARTESIAN_POINT('Ctrl Pts',(-39.357082512524,18.234316031401,-2.76162852484942));
#43083=CARTESIAN_POINT('Ctrl Pts',(-39.392982196192,18.2326394199283,-2.74287394441288));
#43084=CARTESIAN_POINT('Ctrl Pts',(-39.4285412562593,18.2247429067445,-2.72507720804866));
#43085=CARTESIAN_POINT('Ctrl Pts',(-39.3854560789677,18.2385989626561,-2.806704608599));
#43086=CARTESIAN_POINT('Ctrl Pts',(-39.4141769794873,18.2369681932566,-2.79171803684677));
#43087=CARTESIAN_POINT('Ctrl Pts',(-39.4427280394942,18.2314503925561,-2.77735004009521));
#43088=CARTESIAN_POINT('Ctrl Pts',(-39.4282569904425,18.2468831045004,-2.87427088692559));
#43089=CARTESIAN_POINT('Ctrl Pts',(-39.4462140714394,18.2456335650916,-2.86492145390258));
#43090=CARTESIAN_POINT('Ctrl Pts',(-39.4641284952161,18.2428263134802,-2.85583107289212));
#43091=CARTESIAN_POINT('Ctrl Pts',(-39.4425640907085,18.2499546634831,-2.89678499625148));
#43092=CARTESIAN_POINT('Ctrl Pts',(-39.4569337160795,18.2488829564956,-2.88931200575023));
#43093=CARTESIAN_POINT('Ctrl Pts',(-39.471282045358,18.2468375527533,-2.88200339188145));
#43094=CARTESIAN_POINT('Ctrl Pts',(-39.4640790716987,18.2550319670924,-2.9305467580359));
#43095=CARTESIAN_POINT('Ctrl Pts',(-39.4730619699745,18.2543045238099,-2.92588285247038));
#43096=CARTESIAN_POINT('Ctrl Pts',(-39.4820395358475,18.2531874490028,-2.92128612729157));
#43097=CARTESIAN_POINT('Ctrl Pts',(-39.471259788484,18.2568027437311,-2.9417991113903));
#43098=CARTESIAN_POINT('Ctrl Pts',(-39.4784461726879,18.2562028894815,-2.9380706271792));
#43099=CARTESIAN_POINT('Ctrl Pts',(-39.4856298942431,18.2553595973052,-2.93438441656583));
#43100=CARTESIAN_POINT('Ctrl Pts',(-39.48204372096,18.2595771436823,-2.95867561371929));
#43101=CARTESIAN_POINT('Ctrl Pts',(-39.4865331229068,18.2591880585981,-2.9563486344656));
#43102=CARTESIAN_POINT('Ctrl Pts',(-39.4910218604795,18.2587017046828,-2.95403872240394));
#43103=CARTESIAN_POINT('Ctrl Pts',(-39.4856405081953,18.2605216504332,-2.96430077645969));
#43104=CARTESIAN_POINT('Ctrl Pts',(-39.4892305469675,18.2602060471952,-2.96244069404455));
#43105=CARTESIAN_POINT('Ctrl Pts',(-39.4928202540979,18.2598297219177,-2.96059130293824));
#43106=CARTESIAN_POINT('Ctrl Pts',(-39.4928382474395,18.2624502093871,-2.97555048018476));
#43107=CARTESIAN_POINT('Ctrl Pts',(-39.4946286518323,18.2622880271486,-2.97462353554838));
#43108=CARTESIAN_POINT('Ctrl Pts',(-39.4964191237195,18.2621138291545,-2.97369889104282));
#43109=CARTESIAN_POINT('Ctrl Pts',(-39.4964375477875,18.2634339488499,-2.98117240404692));
#43110=CARTESIAN_POINT('Ctrl Pts',(-39.4973281609331,18.2633517166985,-2.98071163235519));
#43111=CARTESIAN_POINT('Ctrl Pts',(-39.4982187739313,18.263269484497,-2.9802508603831));
#43112=CARTESIAN_POINT('Ctrl Pts',(-39.5,18.2644264063412,-2.98673344445558));
#43113=CARTESIAN_POINT('Ctrl Pts',(-39.5,18.2644264063412,-2.98673344445558));
#43114=CARTESIAN_POINT('Ctrl Pts',(-39.5,18.2644264063412,-2.98673344445558));
#43115=CARTESIAN_POINT('Origin',(-38.5,21.7255401693197,6.54991633351602E-10));
#43116=CARTESIAN_POINT('',(-39.,21.7255401693197,4.24538528099178));
#43117=CARTESIAN_POINT('',(-39.,21.7255401693197,-0.0980181950384951));
#43118=CARTESIAN_POINT('Origin',(-38.4999999999995,21.7255401693202,3.24538528099092));
#43119=CARTESIAN_POINT('Origin',(-44.,34.999999994595,6.55E-10));
#43120=CARTESIAN_POINT('',(-45.,20.5124191061237,-0.599999999345));
#43121=CARTESIAN_POINT('Origin',(-45.,34.999999994595,6.55E-10));
#43122=CARTESIAN_POINT('',(-44.,21.5133399188016,-0.599999999345));
#43123=CARTESIAN_POINT('Ctrl Pts',(-45.,20.5124191061237,-0.599999999344999));
#43124=CARTESIAN_POINT('Ctrl Pts',(-45.,20.6359758165694,-0.599999999344999));
#43125=CARTESIAN_POINT('Ctrl Pts',(-44.9710914795861,20.7813983486954,-0.599999999344999));
#43126=CARTESIAN_POINT('Ctrl Pts',(-44.8765874788021,21.009674170601,-0.599999999344999));
#43127=CARTESIAN_POINT('Ctrl Pts',(-44.7942865874973,21.1329323008594,-0.599999999345));
#43128=CARTESIAN_POINT('Ctrl Pts',(-44.6197204613676,21.3076006884133,-0.599999999345));
#43129=CARTESIAN_POINT('Ctrl Pts',(-44.4965862673463,21.3899370868742,-0.599999999345));
#43130=CARTESIAN_POINT('Ctrl Pts',(-44.2685787628921,21.4844357492405,-0.599999999345));
#43131=CARTESIAN_POINT('Ctrl Pts',(-44.123376209915,21.5133399188016,-0.599999999345));
#43132=CARTESIAN_POINT('Ctrl Pts',(-44.,21.5133399188016,-0.599999999345));
#43133=CARTESIAN_POINT('Origin',(-44.,34.999999994595,6.55E-10));
#43134=CARTESIAN_POINT('Origin',(-35.3179607461319,34.999999994595,6.55E-10));
#43135=CARTESIAN_POINT('',(-39.,26.0690696232311,-5.52163768230196));
#43136=CARTESIAN_POINT('',(-35.3179607461319,26.0690696232311,-5.52163768230196));
#43137=CARTESIAN_POINT('',(-41.5,40.1133069970551,-9.17082828792356));
#43138=CARTESIAN_POINT('Origin',(-41.5,34.999999994595,6.55E-10));
#43139=CARTESIAN_POINT('',(-39.,40.1133069970551,-9.17082828792356));
#43140=CARTESIAN_POINT('',(-35.3179607461319,40.1133069970551,-9.17082828792356));
#43141=CARTESIAN_POINT('Origin',(-39.,34.999999994595,6.55E-10));
#43142=CARTESIAN_POINT('Origin',(-35.3179607461319,45.925692710035,-9.04424050588343));
#43143=CARTESIAN_POINT('',(-39.,40.600288616337,-9.04424050588343));
#43144=CARTESIAN_POINT('',(-41.5,40.600288616337,-9.04424050588343));
#43145=CARTESIAN_POINT('',(-42.,40.600288616337,-9.04424050588343));
#43146=CARTESIAN_POINT('',(-41.5000000000004,45.7278783986988,-9.04424052035057));
#43147=CARTESIAN_POINT('',(-41.5,45.925692710035,-9.04424050588343));
#43148=CARTESIAN_POINT('Ctrl Pts',(-41.4999999863947,45.7278783849965,-9.04424050588343));
#43149=CARTESIAN_POINT('Ctrl Pts',(-41.4989575245769,45.7289134916217,-9.04424050588343));
#43150=CARTESIAN_POINT('Ctrl Pts',(-41.4979150491538,45.7299486117559,-9.04424050588343));
#43151=CARTESIAN_POINT('Ctrl Pts',(-41.496611954875,45.7312425119236,-9.04424050588343));
#43152=CARTESIAN_POINT('Ctrl Pts',(-41.4963410586823,45.731507728408,-9.04424050588343));
#43153=CARTESIAN_POINT('Ctrl Pts',(-41.4958079020604,45.7320316239049,-9.04424050588343));
#43154=CARTESIAN_POINT('Ctrl Pts',(-41.4950075021982,45.732816720824,-9.04424050588343));
#43155=CARTESIAN_POINT('Ctrl Pts',(-41.4920653807838,45.7356871913015,-9.04424050588343));
#43156=CARTESIAN_POINT('Ctrl Pts',(-41.485053521909,45.7424071161188,-9.04424050588343));
#43157=CARTESIAN_POINT('Ctrl Pts',(-41.4740518184729,45.7525050091841,-9.04424050588343));
#43158=CARTESIAN_POINT('Ctrl Pts',(-41.4650206065347,45.7603253376589,-9.04424050588343));
#43159=CARTESIAN_POINT('Ctrl Pts',(-41.455874133144,45.7680162950512,-9.04424050588343));
#43160=CARTESIAN_POINT('Ctrl Pts',(-41.4512386468437,45.7718007126244,-9.04424050588343));
#43161=CARTESIAN_POINT('Ctrl Pts',(-41.4278314383774,45.7903528744546,-9.04424050588343));
#43162=CARTESIAN_POINT('Ctrl Pts',(-41.408427535806,45.803971097651,-9.04424050588343));
#43163=CARTESIAN_POINT('Ctrl Pts',(-41.3683622144799,45.8289387080156,-9.04424050588343));
#43164=CARTESIAN_POINT('Ctrl Pts',(-41.3270405528109,45.8516396038261,-9.04424050588343));
#43165=CARTESIAN_POINT('Ctrl Pts',(-41.2833493406892,45.8700653089784,-9.04424050588343));
#43166=CARTESIAN_POINT('Ctrl Pts',(-41.2553247044489,45.8802866146071,-9.04424050588343));
#43167=CARTESIAN_POINT('Ctrl Pts',(-41.2496913297918,45.8822630341662,-9.04424050588343));
#43168=CARTESIAN_POINT('Ctrl Pts',(-41.2384136513533,45.8860676194529,-9.04424050588343));
#43169=CARTESIAN_POINT('Ctrl Pts',(-41.2214609174604,45.8915593252978,-9.04424050588343));
#43170=CARTESIAN_POINT('Ctrl Pts',(-41.2044024102307,45.8964225983601,-9.04424050588343));
#43171=CARTESIAN_POINT('Ctrl Pts',(-41.1701505715342,45.9053481111329,-9.04424050588343));
#43172=CARTESIAN_POINT('Ctrl Pts',(-41.1241226655105,45.9151171234807,-9.04424050588343));
#43173=CARTESIAN_POINT('Ctrl Pts',(-41.0540721293783,45.9237777729692,-9.04424050588343));
#43174=CARTESIAN_POINT('Ctrl Pts',(-41.0067222812585,45.9256927100353,-9.04424050588343));
#43175=CARTESIAN_POINT('Ctrl Pts',(-40.9828862029043,45.925692710035,-9.04424050588343));
#43176=CARTESIAN_POINT('',(-39.,34.999999994595,-9.04424050588343));
#43177=CARTESIAN_POINT('Origin',(-41.5,34.999999994595,6.55E-10));
#43178=CARTESIAN_POINT('',(-42.,39.8698161874141,-8.73412217894363));
#43179=CARTESIAN_POINT('Origin',(-42.,34.999999994595,6.55E-10));
#43180=CARTESIAN_POINT('Origin',(-41.5,39.8698161874141,-8.73412217894363));
#43181=CARTESIAN_POINT('Origin',(-35.3179607461319,40.600288616337,-10.0442405058834));
#43182=CARTESIAN_POINT('Origin',(-41.5,40.600288616337,-10.0442405058834));
#43183=CARTESIAN_POINT('Origin',(-39.,40.600288616337,-10.0442405058834));
#43184=CARTESIAN_POINT('Origin',(-39.,52.6127679742695,-3.71354333343353));
#43185=CARTESIAN_POINT('',(-45.5,51.7756531463269,-4.26057054010477));
#43186=CARTESIAN_POINT('',(-45.,51.7756531463269,-4.26057054010477));
#43187=CARTESIAN_POINT('',(-39.,51.7756531463269,-4.26057054010477));
#43188=CARTESIAN_POINT('Origin',(-45.5,52.6127679742695,-3.71354333343353));
#43189=CARTESIAN_POINT('Origin',(-45.,52.6127679742695,-3.71354333343353));
#43190=CARTESIAN_POINT('Origin',(-35.3179607461319,25.2185048259584,-6.04750793782168));
#43191=CARTESIAN_POINT('',(-39.,25.2185048259584,-5.04750793782168));
#43192=CARTESIAN_POINT('',(-39.,25.2185048259584,-5.04750793782168));
#43193=CARTESIAN_POINT('Origin',(-39.,25.2185048259584,-6.04750793782168));
#43194=CARTESIAN_POINT('Origin',(-45.,50.5871414377259,-8.30646623141651));
#43195=CARTESIAN_POINT('',(-45.,50.8553569437039,-8.43044283154557));
#43196=CARTESIAN_POINT('',(-45.,50.5871414377259,-8.30646623141651));
#43197=CARTESIAN_POINT('',(-45.,50.5871414377259,-8.30646623141651));
#43198=CARTESIAN_POINT('Origin',(-45.,48.5946168001447,-6.3392739254555));
#43199=CARTESIAN_POINT('',(-45.,47.8027400910494,-6.80733765974042));
#43200=CARTESIAN_POINT('Origin',(-29.,57.5946168001448,-3.5392739254555));
#43201=CARTESIAN_POINT('',(-39.,57.5946168001448,-3.5392739254555));
#43202=CARTESIAN_POINT('',(-39.,57.5946168001448,0.460726074544505));
#43203=CARTESIAN_POINT('',(-39.,57.5946168001448,0.960726074544506));
#43204=CARTESIAN_POINT('',(-29.,57.5946168001448,0.460726074544506));
#43205=CARTESIAN_POINT('',(-33.5,57.5946168001448,-3.5392739254555));
#43206=CARTESIAN_POINT('',(-33.5,57.5946168001448,-3.5392739254555));
#43207=CARTESIAN_POINT('',(-29.,57.5946168001448,-3.5392739254555));
#43208=CARTESIAN_POINT('Origin',(-46.,24.5171568688013,-0.599999999345));
#43209=CARTESIAN_POINT('',(-45.5,29.0300753719553,-0.599999999345));
#43210=CARTESIAN_POINT('',(-42.5,29.0300753719553,-0.599999999345));
#43211=CARTESIAN_POINT('',(-42.,29.0300753719553,-0.599999999345));
#43212=CARTESIAN_POINT('',(-42.4999999999993,21.3792341097314,-0.599999999345));
#43213=CARTESIAN_POINT('',(-42.5,20.5124191061237,-0.599999999345));
#43214=CARTESIAN_POINT('',(-43.,21.5133399188016,-0.599999999345));
#43215=CARTESIAN_POINT('Ctrl Pts',(-43.,21.5133399188016,-0.599999999345));
#43216=CARTESIAN_POINT('Ctrl Pts',(-42.876623790085,21.5133399188016,-0.599999999345));
#43217=CARTESIAN_POINT('Ctrl Pts',(-42.7314212371079,21.4844357492405,-0.599999999345));
#43218=CARTESIAN_POINT('Ctrl Pts',(-42.5789143576127,21.4212286361744,-0.599999999345));
#43219=CARTESIAN_POINT('Ctrl Pts',(-42.5390282352261,21.4017889231421,-0.599999999345));
#43220=CARTESIAN_POINT('Ctrl Pts',(-42.4999999999992,21.3792341097314,-0.599999999345));
#43221=CARTESIAN_POINT('',(-35.8316689588642,21.5133399188016,-0.599999999345));
#43222=CARTESIAN_POINT('',(-45.,19.0050007760892,-0.599999999345));
#43223=CARTESIAN_POINT('',(-45.,20.1123922190465,-0.599999999345));
#43224=CARTESIAN_POINT('',(-45.5,19.0050007760892,-0.599999999345));
#43225=CARTESIAN_POINT('',(-46.,19.0050007760892,-0.599999999345));
#43226=CARTESIAN_POINT('',(-45.5,24.5171568688013,-0.599999999345));
#43227=CARTESIAN_POINT('Origin',(-38.5,19.7255401693197,6.5499063415088E-10));
#43228=CARTESIAN_POINT('',(-38.9999999569785,19.7255368100699,4.2453886351283));
#43229=CARTESIAN_POINT('Origin',(-38.4999787117434,19.7255206107479,3.24531886108545));
#43230=CARTESIAN_POINT('',(-39.,19.7255401693197,4.45249206217833));
#43231=CARTESIAN_POINT('Ctrl Pts',(-39.1464465764959,21.7257963191156,4.59893863867423));
#43232=CARTESIAN_POINT('Ctrl Pts',(-38.9999593663855,21.7257212747019,4.45245142856379));
#43233=CARTESIAN_POINT('Ctrl Pts',(-38.9999999931593,21.7256682191115,4.24528722681498));
#43234=CARTESIAN_POINT('Ctrl Pts',(-39.1464634170654,21.6602603482896,4.59895547924376));
#43235=CARTESIAN_POINT('Ctrl Pts',(-38.9999748341363,21.6793856140906,4.45246689631453));
#43236=CARTESIAN_POINT('Ctrl Pts',(-39.0000084101164,21.692906657039,4.24530406763262));
#43237=CARTESIAN_POINT('Ctrl Pts',(-39.1400171767355,21.5947258251822,4.59250923891378));
#43238=CARTESIAN_POINT('Ctrl Pts',(-38.994046097433,21.6329311996428,4.44653815961128));
#43239=CARTESIAN_POINT('Ctrl Pts',(-38.9967865689158,21.6601458581973,4.23885771343968));
#43240=CARTESIAN_POINT('Ctrl Pts',(-39.1144632601427,21.4662576111171,4.56695532232101));
#43241=CARTESIAN_POINT('Ctrl Pts',(-38.9707199974353,21.5430173938286,4.42321205961358));
#43242=CARTESIAN_POINT('Ctrl Pts',(-38.9840145639613,21.5959237595463,4.21330327190672));
#43243=CARTESIAN_POINT('Ctrl Pts',(-39.0953727103553,21.4033245021669,4.54786477253367));
#43244=CARTESIAN_POINT('Ctrl Pts',(-38.9532169021879,21.4993407965975,4.40570896436624));
#43245=CARTESIAN_POINT('Ctrl Pts',(-38.9744729908239,21.5644628247322,4.19421237408121));
#43246=CARTESIAN_POINT('Ctrl Pts',(-39.0452795734807,21.2823889717424,4.49777163565901));
#43247=CARTESIAN_POINT('Ctrl Pts',(-38.9077050083922,21.4174682540841,4.36019707057048));
#43248=CARTESIAN_POINT('Ctrl Pts',(-38.9494357984369,21.5040046541739,4.14411817045999));
#43249=CARTESIAN_POINT('Ctrl Pts',(-39.0142782037993,21.224389488238,4.46677026597765));
#43250=CARTESIAN_POINT('Ctrl Pts',(-38.879467578496,21.379123603316,4.33195964067435));
#43251=CARTESIAN_POINT('Ctrl Pts',(-38.9339408455836,21.4750089453472,4.1131162004694));
#43252=CARTESIAN_POINT('Ctrl Pts',(-38.9415542396192,21.1155503843622,4.39404630179754));
#43253=CARTESIAN_POINT('Ctrl Pts',(-38.8139510374573,21.310227924253,4.26644309963554));
#43254=CARTESIAN_POINT('Ctrl Pts',(-38.8975916626433,21.420595242064,4.04039059104397));
#43255=CARTESIAN_POINT('Ctrl Pts',(-38.8998334160569,21.0647134135968,4.3523254782352));
#43256=CARTESIAN_POINT('Ctrl Pts',(-38.7763600409834,21.279632197814,4.22885210316172));
#43257=CARTESIAN_POINT('Ctrl Pts',(-38.8767383967121,21.3951786071568,3.9986688841259));
#43258=CARTESIAN_POINT('Ctrl Pts',(-38.8072733651297,20.9721533626695,4.259765427308));
#43259=CARTESIAN_POINT('Ctrl Pts',(-38.6940769277129,21.2282175204938,4.14656898989117));
#43260=CARTESIAN_POINT('Ctrl Pts',(-38.8304731995627,21.3488997190596,3.90610655238314));
#43261=CARTESIAN_POINT('Ctrl Pts',(-38.7564363959324,20.930432540155,4.2089284581107));
#43262=CARTESIAN_POINT('Ctrl Pts',(-38.6490267800469,21.207490281533,4.10151884222526));
#43263=CARTESIAN_POINT('Ctrl Pts',(-38.8050624884519,21.3280386002814,3.85526837283333));
#43264=CARTESIAN_POINT('Ctrl Pts',(-38.6475972889203,20.8577085738793,4.10008935109861));
#43265=CARTESIAN_POINT('Ctrl Pts',(-38.5541985142433,21.1773746221138,4.00669057642161));
#43266=CARTESIAN_POINT('Ctrl Pts',(-38.7506581296402,21.2916725623259,3.74642626850048));
#43267=CARTESIAN_POINT('Ctrl Pts',(-38.5895978103376,20.8267072066348,4.04208987251594));
#43268=CARTESIAN_POINT('Ctrl Pts',(-38.504065524732,21.168236619467,3.95655758691019));
#43269=CARTESIAN_POINT('Ctrl Pts',(-38.7216659045744,21.2761685048643,3.68842519451931));
#43270=CARTESIAN_POINT('Ctrl Pts',(-38.468662273206,20.776614066982,3.92115433538435));
#43271=CARTESIAN_POINT('Ctrl Pts',(-38.4018336399262,21.1623409039058,3.85432570210466));
#43272=CARTESIAN_POINT('Ctrl Pts',(-38.6612119130009,21.2511127665618,3.5674858349066));
#43273=CARTESIAN_POINT('Ctrl Pts',(-38.4057291724627,20.7575235195491,3.85822123464104));
#43274=CARTESIAN_POINT('Ctrl Pts',(-38.3494444973764,21.165999727792,3.80193655955489));
#43275=CARTESIAN_POINT('Ctrl Pts',(-38.6297517092871,21.2415616400292,3.50455068049618));
#43276=CARTESIAN_POINT('Ctrl Pts',(-38.2772609486846,20.7319696010243,3.72975301086293));
#43277=CARTESIAN_POINT('Ctrl Pts',(-38.245742257131,21.1861053328133,3.6982343193092));
#43278=CARTESIAN_POINT('Ctrl Pts',(-38.5655282212259,21.22877106589,3.37607766713466));
#43279=CARTESIAN_POINT('Ctrl Pts',(-38.2117264341041,20.7255233616529,3.66421849628246));
#43280=CARTESIAN_POINT('Ctrl Pts',(-38.1942890677528,21.2031338859603,3.64678112993118));
#43281=CARTESIAN_POINT('Ctrl Pts',(-38.5327652990079,21.2255400971374,3.31054054493344));
#43282=CARTESIAN_POINT('Ctrl Pts',(-38.1461904595966,20.7255402022306,3.59868252177487));
#43283=CARTESIAN_POINT('Ctrl Pts',(-38.1462544999649,21.2258119718161,3.59874656214325));
#43284=CARTESIAN_POINT('Ctrl Pts',(-38.5000000005279,21.2255401201565,3.24500105575491));
#43285=CARTESIAN_POINT('',(-39.,21.2045380277352,4.45249206217834));
#43286=CARTESIAN_POINT('Ctrl Pts',(-39.,21.2045380277352,4.45249206217832));
#43287=CARTESIAN_POINT('Ctrl Pts',(-39.,21.3008251669304,4.45249206221659));
#43288=CARTESIAN_POINT('Ctrl Pts',(-39.0000000000062,21.3965734173472,4.43569854959937));
#43289=CARTESIAN_POINT('Ctrl Pts',(-39.0000000000062,21.5319333238365,4.38317740438376));
#43290=CARTESIAN_POINT('Ctrl Pts',(-39.,21.5756326282393,4.36086176771965));
#43291=CARTESIAN_POINT('Ctrl Pts',(-39.,21.6554324370807,4.30861274069145));
#43292=CARTESIAN_POINT('Ctrl Pts',(-39.,21.6909489715919,4.27981443779032));
#43293=CARTESIAN_POINT('Ctrl Pts',(-39.,21.7244769111452,4.24644851929847));
#43294=CARTESIAN_POINT('Ctrl Pts',(-39.,21.7250089648679,4.24591732890776));
#43295=CARTESIAN_POINT('Ctrl Pts',(-39.,21.7255401693197,4.24538528099177));
#43296=CARTESIAN_POINT('Origin',(-38.1470114564408,21.7245991495921,3.59950351982835));
#43297=CARTESIAN_POINT('Ctrl Pts',(-38.1462572731518,20.7255401513379,3.59874933533011));
#43298=CARTESIAN_POINT('Ctrl Pts',(-38.1463046022227,20.2253392826154,3.59879666440107));
#43299=CARTESIAN_POINT('Ctrl Pts',(-38.4999999999868,20.2255401961801,3.24510127662862));
#43300=CARTESIAN_POINT('Ctrl Pts',(-38.2121636970542,20.72555267005,3.66465575923247));
#43301=CARTESIAN_POINT('Ctrl Pts',(-38.1946078611317,20.2481352042117,3.64709992330954));
#43302=CARTESIAN_POINT('Ctrl Pts',(-38.532951213131,20.2255402139663,3.31101031535884));
#43303=CARTESIAN_POINT('Ctrl Pts',(-38.2780681553458,20.7190286310453,3.73056021752408));
#43304=CARTESIAN_POINT('Ctrl Pts',(-38.2463675111531,20.2652184255456,3.69885957333151));
#43305=CARTESIAN_POINT('Ctrl Pts',(-38.565900212778,20.2222723628149,3.37691671021798));
#43306=CARTESIAN_POINT('Ctrl Pts',(-38.407254472938,20.6931736218478,3.85974653511633));
#43307=CARTESIAN_POINT('Ctrl Pts',(-38.3506869574157,20.2852760717712,3.80317901959393));
#43308=CARTESIAN_POINT('Ctrl Pts',(-38.630485454596,20.2093347539537,3.50610658453323));
#43309=CARTESIAN_POINT('Ctrl Pts',(-38.4705347796647,20.6738555693773,3.92302684184305));
#43310=CARTESIAN_POINT('Ctrl Pts',(-38.4033912928499,20.2888369536623,3.85588335502822));
#43311=CARTESIAN_POINT('Ctrl Pts',(-38.6621208762061,20.1996713903363,3.5693884143297));
#43312=CARTESIAN_POINT('Ctrl Pts',(-38.5920768550543,20.6231753537079,4.04456891723265));
#43313=CARTESIAN_POINT('Ctrl Pts',(-38.5061830164427,20.2825955441402,3.95867507862105));
#43314=CARTESIAN_POINT('Ctrl Pts',(-38.7228816482343,20.1743245090983,3.69093332436145));
#43315=CARTESIAN_POINT('Ctrl Pts',(-38.6503355783925,20.5918144601458,4.10282764057083));
#43316=CARTESIAN_POINT('Ctrl Pts',(-38.5565669475031,20.2732153223087,4.00905900968133));
#43317=CARTESIAN_POINT('Ctrl Pts',(-38.7520054127713,20.1586415827856,3.74919322854446));
#43318=CARTESIAN_POINT('Ctrl Pts',(-38.7595684668405,20.518267630651,4.2120605290188));
#43319=CARTESIAN_POINT('Ctrl Pts',(-38.6517811607899,20.2425001122587,4.10427322296828));
#43320=CARTESIAN_POINT('Ctrl Pts',(-38.8066105511857,20.1218652238858,3.85842833570072));
#43321=CARTESIAN_POINT('Ctrl Pts',(-38.8105398978067,20.476083535291,4.26303195998505));
#43322=CARTESIAN_POINT('Ctrl Pts',(-38.696973157022,20.221417076274,4.14946521920037));
#43323=CARTESIAN_POINT('Ctrl Pts',(-38.8320904879864,20.1007726920394,3.90940066031844));
#43324=CARTESIAN_POINT('Ctrl Pts',(-38.9032154807064,20.3825303635642,4.35570754288468));
#43325=CARTESIAN_POINT('Ctrl Pts',(-38.779391773723,20.1692200507405,4.23188383590132));
#43326=CARTESIAN_POINT('Ctrl Pts',(-38.8784172753292,20.0539970424009,4.00207792736665));
#43327=CARTESIAN_POINT('Ctrl Pts',(-38.9449173162986,20.3311636249377,4.39740937847691));
#43328=CARTESIAN_POINT('Ctrl Pts',(-38.8169821824962,20.1381958541655,4.26947424467455));
#43329=CARTESIAN_POINT('Ctrl Pts',(-38.8992628993741,20.028315098226,4.04378041297156));
#43330=CARTESIAN_POINT('Ctrl Pts',(-39.0174313967732,20.221242438767,4.46992345895153));
#43331=CARTESIAN_POINT('Ctrl Pts',(-38.8823308068068,20.0684230182907,4.33482286898507));
#43332=CARTESIAN_POINT('Ctrl Pts',(-38.9355104847273,19.9733589503371,4.1162957034858));
#43333=CARTESIAN_POINT('Ctrl Pts',(-39.0482418325485,20.162690732765,4.50073389472685));
#43334=CARTESIAN_POINT('Ctrl Pts',(-38.9104043915022,20.0296252734399,4.36289645368056));
#43335=CARTESIAN_POINT('Ctrl Pts',(-38.9509114826831,19.9440861441119,4.14710657852245));
#43336=CARTESIAN_POINT('Ctrl Pts',(-39.0977743044738,20.040676419536,4.55026636665211));
#43337=CARTESIAN_POINT('Ctrl Pts',(-38.9554174663834,19.9468798542435,4.40790952856176));
#43338=CARTESIAN_POINT('Ctrl Pts',(-38.9756708542083,19.8830862055383,4.19663982883342));
#43339=CARTESIAN_POINT('Ctrl Pts',(-39.1164951072866,19.9772168492738,4.5689871694649));
#43340=CARTESIAN_POINT('Ctrl Pts',(-38.9725860550694,19.9027778034052,4.42507811724778));
#43341=CARTESIAN_POINT('Ctrl Pts',(-38.9850285683817,19.8513606357535,4.2153608830672));
#43342=CARTESIAN_POINT('Ctrl Pts',(-39.1411196304398,19.8478546030577,4.5936116926181));
#43343=CARTESIAN_POINT('Ctrl Pts',(-38.9950667773803,19.8121580843539,4.44755883955856));
#43344=CARTESIAN_POINT('Ctrl Pts',(-38.9973372985047,19.7866884869349,4.23998577975064));
#43345=CARTESIAN_POINT('Ctrl Pts',(-39.1470227465266,19.7819559842235,4.59951480870491));
#43346=CARTESIAN_POINT('Ctrl Pts',(-39.0004966222791,19.7654220878734,4.45298868445749));
#43347=CARTESIAN_POINT('Ctrl Pts',(-39.0002879913939,19.7537441030219,4.24588897487879));
#43348=CARTESIAN_POINT('Ctrl Pts',(-39.1464021965157,19.7161155308866,4.598894258694));
#43349=CARTESIAN_POINT('Ctrl Pts',(-38.9999293853924,19.7188765600821,4.45242144757075));
#43350=CARTESIAN_POINT('Ctrl Pts',(-38.9999778052401,19.720828532882,4.24526841347127));
#43351=CARTESIAN_POINT('',(-39.,20.2465429544735,4.45249206217834));
#43352=CARTESIAN_POINT('Ctrl Pts',(-38.99999993555,19.7255334503096,4.24539198975394));
#43353=CARTESIAN_POINT('Ctrl Pts',(-38.9999999358904,19.7263281247927,4.24618788058609));
#43354=CARTESIAN_POINT('Ctrl Pts',(-39.,19.7265795127331,4.24646470977148));
#43355=CARTESIAN_POINT('Ctrl Pts',(-39.,19.7599229652764,4.27922044541505));
#43356=CARTESIAN_POINT('Ctrl Pts',(-39.,19.7958071744378,4.30870610834091));
#43357=CARTESIAN_POINT('Ctrl Pts',(-39.,19.8753833962655,4.3608287869574));
#43358=CARTESIAN_POINT('Ctrl Pts',(-39.0000000000057,19.9190457575193,4.38312303219407));
#43359=CARTESIAN_POINT('Ctrl Pts',(-39.0000000000057,20.0543749715938,4.43567530216436));
#43360=CARTESIAN_POINT('Ctrl Pts',(-39.,20.1501887651632,4.45249206221052));
#43361=CARTESIAN_POINT('Ctrl Pts',(-39.,20.2465429544735,4.45249206217833));
#43362=CARTESIAN_POINT('Origin',(-38.1470191121941,19.7264777750522,3.59951117560489));
#43363=CARTESIAN_POINT('Origin',(-42.5,44.0301171154896,-5.44126213566782));
#43364=CARTESIAN_POINT('',(-42.,44.3597593181683,-5.5936318482172));
#43365=CARTESIAN_POINT('Ctrl Pts',(-42.5,44.9368005344368,-5.30952630282034));
#43366=CARTESIAN_POINT('Ctrl Pts',(-42.4693214931018,44.9368005344368,-5.30952630282034));
#43367=CARTESIAN_POINT('Ctrl Pts',(-42.438735398437,44.9334293437634,-5.31107746144859));
#43368=CARTESIAN_POINT('Ctrl Pts',(-42.3572140089482,44.9153607852898,-5.31942199117872));
#43369=CARTESIAN_POINT('Ctrl Pts',(-42.3091583591543,44.8948062033049,-5.32893045402432));
#43370=CARTESIAN_POINT('Ctrl Pts',(-42.2122788312625,44.8339566456983,-5.35744022010934));
#43371=CARTESIAN_POINT('Ctrl Pts',(-42.1666692197098,44.7909059160422,-5.37781140783887));
#43372=CARTESIAN_POINT('Ctrl Pts',(-42.0872212431615,44.6885725964396,-5.42717314417569));
#43373=CARTESIAN_POINT('Ctrl Pts',(-42.0554640174147,44.6277094584301,-5.45704131989472));
#43374=CARTESIAN_POINT('Ctrl Pts',(-42.0117784211058,44.4993327569534,-5.52143090175417));
#43375=CARTESIAN_POINT('Ctrl Pts',(-42.0003916727879,44.431048067398,-5.55638285908588));
#43376=CARTESIAN_POINT('Ctrl Pts',(-42.00000331059,44.3621090125528,-5.5924035000473));
#43377=CARTESIAN_POINT('Ctrl Pts',(-42.,44.3609341213816,-5.59301759162487));
#43378=CARTESIAN_POINT('Ctrl Pts',(-42.,44.3597593181683,-5.59363184821719));
#43379=CARTESIAN_POINT('',(-42.,40.3243975531895,-3.72837640711721));
#43380=CARTESIAN_POINT('',(-42.,44.7270136458737,-5.76338692171892));
#43381=CARTESIAN_POINT('Ctrl Pts',(-42.,40.3243975531895,-3.72837640711721));
#43382=CARTESIAN_POINT('Ctrl Pts',(-42.,40.3240403816243,-3.72705225349016));
#43383=CARTESIAN_POINT('Ctrl Pts',(-42.0000033207593,40.3236830750716,-3.72572813403057));
#43384=CARTESIAN_POINT('Ctrl Pts',(-42.0004541950922,40.2994116461814,-3.63581851390176));
#43385=CARTESIAN_POINT('Ctrl Pts',(-42.0157573105942,40.2747122081378,-3.54683042359109));
#43386=CARTESIAN_POINT('Ctrl Pts',(-42.0728019198682,40.2300648181134,-3.39000514927648));
#43387=CARTESIAN_POINT('Ctrl Pts',(-42.1117195110958,40.2096120486903,-3.31992019235924));
#43388=CARTESIAN_POINT('Ctrl Pts',(-42.2018967293794,40.1784437356806,-3.21492170975514));
#43389=CARTESIAN_POINT('Ctrl Pts',(-42.2479008339596,40.1665637525278,-3.17555129913948));
#43390=CARTESIAN_POINT('Ctrl Pts',(-42.3442168820676,40.1502391476712,-3.12183541479049));
#43391=CARTESIAN_POINT('Ctrl Pts',(-42.3916288820851,40.1450378828802,-3.10489199315609));
#43392=CARTESIAN_POINT('Ctrl Pts',(-42.4610040616797,40.141819202885,-3.09440760124827));
#43393=CARTESIAN_POINT('Ctrl Pts',(-42.4805205119926,40.1413699032525,-3.09294608072936));
#43394=CARTESIAN_POINT('Ctrl Pts',(-42.5,40.1413699032525,-3.09294608072936));
#43395=CARTESIAN_POINT('Origin',(-41.5,40.600288616337,-10.0442405058834));
#43396=CARTESIAN_POINT('',(-42.,40.600288616337,-8.54424050588343));
#43397=CARTESIAN_POINT('Origin',(-42.,40.600288616337,-10.0442405058834));
#43398=CARTESIAN_POINT('Origin',(-41.5,40.600288616337,-8.54424050588343));
#43399=CARTESIAN_POINT('Origin',(-42.5,48.5946168001447,-6.3392739254555));
#43400=CARTESIAN_POINT('',(-42.,44.902988110908,-8.54424050588343));
#43401=CARTESIAN_POINT('Origin',(-42.5,44.902988110908,-8.54424050588343));
#43402=CARTESIAN_POINT('Origin',(-42.,48.5946168001447,-6.3392739254555));
#43403=CARTESIAN_POINT('Origin',(-41.5,34.999999994595,-8.54424050588343));
#43404=CARTESIAN_POINT('Ctrl Pts',(-42.,44.902988110908,-8.54424050588343));
#43405=CARTESIAN_POINT('Ctrl Pts',(-42.,44.9217152275532,-8.55991728673912));
#43406=CARTESIAN_POINT('Ctrl Pts',(-41.99926699101,44.9405761487081,-8.5752530958335));
#43407=CARTESIAN_POINT('Ctrl Pts',(-41.9978770235583,44.9595626840342,-8.59027607382555));
#43408=CARTESIAN_POINT('Ctrl Pts',(-41.9973455416108,44.9668225668177,-8.59602041092588));
#43409=CARTESIAN_POINT('Ctrl Pts',(-41.9967179453166,44.9741007887899,-8.60171894364661));
#43410=CARTESIAN_POINT('Ctrl Pts',(-41.9959982552416,44.9813969174924,-8.60737315034953));
#43411=CARTESIAN_POINT('Ctrl Pts',(-41.9948357632704,44.9931821168892,-8.61650620654169));
#43412=CARTESIAN_POINT('Ctrl Pts',(-41.9934327691023,45.0050141049486,-8.62552362355322));
#43413=CARTESIAN_POINT('Ctrl Pts',(-41.9917995123892,45.0168907527111,-8.63443039129122));
#43414=CARTESIAN_POINT('Ctrl Pts',(-41.9897181963016,45.0320255798673,-8.64578059657901));
#43415=CARTESIAN_POINT('Ctrl Pts',(-41.9872630045812,45.0472328338408,-8.65695106915648));
#43416=CARTESIAN_POINT('Ctrl Pts',(-41.984453841326,45.0625086902382,-8.6679517649698));
#43417=CARTESIAN_POINT('Ctrl Pts',(-41.9801247004088,45.0860499831313,-8.68490470007424));
#43418=CARTESIAN_POINT('Ctrl Pts',(-41.9749549181365,45.1097541946394,-8.70145443366791));
#43419=CARTESIAN_POINT('Ctrl Pts',(-41.9689740864101,45.1336046186899,-8.7176289419902));
#43420=CARTESIAN_POINT('Ctrl Pts',(-41.9679244873749,45.13779022083,-8.72046746832024));
#43421=CARTESIAN_POINT('Ctrl Pts',(-41.966849894493,45.1419803414508,-8.72329444248294));
#43422=CARTESIAN_POINT('Ctrl Pts',(-41.9657504515975,45.1461749072067,-8.72611001084982));
#43423=CARTESIAN_POINT('Ctrl Pts',(-41.9642673716375,45.1518331150488,-8.72990803713926));
#43424=CARTESIAN_POINT('Ctrl Pts',(-41.9627388825222,45.1574993790093,-8.73368527854127));
#43425=CARTESIAN_POINT('Ctrl Pts',(-41.9611650123427,45.1631734698631,-8.73744204070059));
#43426=CARTESIAN_POINT('Ctrl Pts',(-41.9607679814752,45.1646048390084,-8.73838973674212));
#43427=CARTESIAN_POINT('Ctrl Pts',(-41.9603681175447,45.1660365084498,-8.73933599886251));
#43428=CARTESIAN_POINT('Ctrl Pts',(-41.9599653926612,45.1674685814126,-8.74028090364377));
#43429=CARTESIAN_POINT('Ctrl Pts',(-41.9579598774666,45.1746001101675,-8.74498640105417));
#43430=CARTESIAN_POINT('Ctrl Pts',(-41.955880829506,45.1817504452265,-8.74966397918282));
#43431=CARTESIAN_POINT('Ctrl Pts',(-41.9537330860392,45.1889019974108,-8.75430308378186));
#43432=CARTESIAN_POINT('Ctrl Pts',(-41.953335044313,45.1902273960073,-8.75516284996496));
#43433=CARTESIAN_POINT('Ctrl Pts',(-41.9529347426312,45.1915525258364,-8.75602109581612));
#43434=CARTESIAN_POINT('Ctrl Pts',(-41.9525321577263,45.1928774682436,-8.75687788307363));
#43435=CARTESIAN_POINT('Ctrl Pts',(-41.948591555106,45.2058463388042,-8.7652643329151));
#43436=CARTESIAN_POINT('Ctrl Pts',(-41.9444306648395,45.2188024265432,-8.7735143558228));
#43437=CARTESIAN_POINT('Ctrl Pts',(-41.9400504090668,45.231742825263,-8.78163392930062));
#43438=CARTESIAN_POINT('Ctrl Pts',(-41.9377366778172,45.238578180652,-8.78592283658468));
#43439=CARTESIAN_POINT('Ctrl Pts',(-41.9353619641797,45.2454093037384,-8.79017544543466));
#43440=CARTESIAN_POINT('Ctrl Pts',(-41.9329257017781,45.2522353739754,-8.79439229947627));
#43441=CARTESIAN_POINT('Ctrl Pts',(-41.9258772129349,45.2719842646844,-8.80659231891841));
#43442=CARTESIAN_POINT('Ctrl Pts',(-41.9183136346165,45.2916915246547,-8.81849347201985));
#43443=CARTESIAN_POINT('Ctrl Pts',(-41.910217493462,45.3113410897915,-8.83011052782056));
#43444=CARTESIAN_POINT('Ctrl Pts',(-41.9094845927378,45.3131198607202,-8.83116215827605));
#43445=CARTESIAN_POINT('Ctrl Pts',(-41.9087473256333,45.3148981526486,-8.83221145929809));
#43446=CARTESIAN_POINT('Ctrl Pts',(-41.9080056754341,45.3166759591509,-8.83325844445048));
#43447=CARTESIAN_POINT('Ctrl Pts',(-41.9005545315738,45.3345370640473,-8.84377719978644));
#43448=CARTESIAN_POINT('Ctrl Pts',(-41.8926617593855,45.3523499135917,-8.85406244540301));
#43449=CARTESIAN_POINT('Ctrl Pts',(-41.8842899617511,45.3700942133327,-8.86411913234023));
#43450=CARTESIAN_POINT('Ctrl Pts',(-41.8795553606888,45.380129355613,-8.86980660864286));
#43451=CARTESIAN_POINT('Ctrl Pts',(-41.8746675657325,45.3901422940905,-8.87542085810376));
#43452=CARTESIAN_POINT('Ctrl Pts',(-41.8696184988485,45.4001301957612,-8.8809631889771));
#43453=CARTESIAN_POINT('Ctrl Pts',(-41.8648510912,45.4095609281936,-8.88619634417246));
#43454=CARTESIAN_POINT('Ctrl Pts',(-41.8599393529639,45.4189689378561,-8.89136515656763));
#43455=CARTESIAN_POINT('Ctrl Pts',(-41.8548730788033,45.4283492718046,-8.89646937487582));
#43456=CARTESIAN_POINT('Ctrl Pts',(-41.8525827714795,45.4325898333813,-8.89877683558625));
#43457=CARTESIAN_POINT('Ctrl Pts',(-41.8502613638914,45.4368238606404,-8.90107060968825));
#43458=CARTESIAN_POINT('Ctrl Pts',(-41.8479069515496,45.4410525278538,-8.90335156539488));
#43459=CARTESIAN_POINT('Ctrl Pts',(-41.8448994391838,45.4464542022802,-8.90626524469058));
#43460=CARTESIAN_POINT('Ctrl Pts',(-41.8418352055889,45.4518516438432,-8.90916037727808));
#43461=CARTESIAN_POINT('Ctrl Pts',(-41.8387233732327,45.4572239437181,-8.91202638213873));
#43462=CARTESIAN_POINT('Ctrl Pts',(-41.8379490304162,45.4585607772424,-8.91273955367935));
#43463=CARTESIAN_POINT('Ctrl Pts',(-41.8371715840211,45.4598963309502,-8.91345106303885));
#43464=CARTESIAN_POINT('Ctrl Pts',(-41.8363912062383,45.4612302114177,-8.91416070858338));
#43465=CARTESIAN_POINT('Ctrl Pts',(-41.8325053766855,45.4678721638856,-8.91769433254054));
#43466=CARTESIAN_POINT('Ctrl Pts',(-41.8285427447655,45.4744804257973,-8.92118599460502));
#43467=CARTESIAN_POINT('Ctrl Pts',(-41.8245000582813,45.4810503220176,-8.92463465959361));
#43468=CARTESIAN_POINT('Ctrl Pts',(-41.8235377795384,45.4826141512931,-8.92545554368212));
#43469=CARTESIAN_POINT('Ctrl Pts',(-41.8225709901412,45.4841758442149,-8.92627400994534));
#43470=CARTESIAN_POINT('Ctrl Pts',(-41.8215996339254,45.4857353191729,-8.92709003533626));
#43471=CARTESIAN_POINT('Ctrl Pts',(-41.8098562016529,45.5045889469695,-8.93695556021317));
#43472=CARTESIAN_POINT('Ctrl Pts',(-41.7974460451304,45.5231265694832,-8.9464672375347));
#43473=CARTESIAN_POINT('Ctrl Pts',(-41.7842200516186,45.5412462580514,-8.95560374436775));
#43474=CARTESIAN_POINT('Ctrl Pts',(-41.7805875545163,45.5462228003549,-8.95811307076099));
#43475=CARTESIAN_POINT('Ctrl Pts',(-41.7768935421867,45.5511671810966,-8.9605938588154));
#43476=CARTESIAN_POINT('Ctrl Pts',(-41.7731337798956,45.5560776923919,-8.96304587628849));
#43477=CARTESIAN_POINT('Ctrl Pts',(-41.7632041736153,45.5690464494629,-8.96952170274114));
#43478=CARTESIAN_POINT('Ctrl Pts',(-41.75281858549,45.5817832043924,-8.97579859997023));
#43479=CARTESIAN_POINT('Ctrl Pts',(-41.7418680590367,45.5942087950184,-8.98185051649874));
#43480=CARTESIAN_POINT('Ctrl Pts',(-41.7343196332262,45.6027740132655,-8.98602222852756));
#43481=CARTESIAN_POINT('Ctrl Pts',(-41.7265018645057,45.6111916179132,-8.99008727610328));
#43482=CARTESIAN_POINT('Ctrl Pts',(-41.7183666093141,45.6194329653189,-8.99403617303334));
#43483=CARTESIAN_POINT('Ctrl Pts',(-41.7172568243484,45.6205572230382,-8.99457486866619));
#43484=CARTESIAN_POINT('Ctrl Pts',(-41.7161408581521,45.6216784231438,-8.99511152314756));
#43485=CARTESIAN_POINT('Ctrl Pts',(-41.7150187648596,45.6227962934492,-8.99564601178507));
#43486=CARTESIAN_POINT('Ctrl Pts',(-41.7120281175915,45.6257756854456,-8.99707055196744));
#43487=CARTESIAN_POINT('Ctrl Pts',(-41.70900015992,45.6287243075931,-8.9984763094132));
#43488=CARTESIAN_POINT('Ctrl Pts',(-41.7059403448518,45.6316334313436,-8.99985935990986));
#43489=CARTESIAN_POINT('Ctrl Pts',(-41.703763557296,45.6337030153665,-9.0008432779059));
#43490=CARTESIAN_POINT('Ctrl Pts',(-41.7015691398645,45.6357540055558,-9.0018163966474));
#43491=CARTESIAN_POINT('Ctrl Pts',(-41.6993578766797,45.6377842033898,-9.0027777857267));
#43492=CARTESIAN_POINT('Ctrl Pts',(-41.6972946362417,45.6396784990562,-9.00367481907793));
#43493=CARTESIAN_POINT('Ctrl Pts',(-41.6952158521099,45.641555574399,-9.00456206138067));
#43494=CARTESIAN_POINT('Ctrl Pts',(-41.6931210371443,45.6434146521169,-9.00543924012301));
#43495=CARTESIAN_POINT('Ctrl Pts',(-41.6899079491655,45.6462661594648,-9.00678468233083));
#43496=CARTESIAN_POINT('Ctrl Pts',(-41.6866574181238,45.6490750873074,-9.00810634480957));
#43497=CARTESIAN_POINT('Ctrl Pts',(-41.683367132931,45.6518388544561,-9.00940337473763));
#43498=CARTESIAN_POINT('Ctrl Pts',(-41.6777690417215,45.6565411278684,-9.01161014145035));
#43499=CARTESIAN_POINT('Ctrl Pts',(-41.6720560193021,45.6611131196413,-9.01374581468396));
#43500=CARTESIAN_POINT('Ctrl Pts',(-41.6662154610016,45.665538373007,-9.01580446686645));
#43501=CARTESIAN_POINT('Ctrl Pts',(-41.6610327553656,45.669465186914,-9.01763124227383));
#43502=CARTESIAN_POINT('Ctrl Pts',(-41.6557496367553,45.6732762891216,-9.01939737122132));
#43503=CARTESIAN_POINT('Ctrl Pts',(-41.6503549411668,45.6769591907994,-9.02109833759718));
#43504=CARTESIAN_POINT('Ctrl Pts',(-41.6460969718104,45.6798660614893,-9.02244089021871));
#43505=CARTESIAN_POINT('Ctrl Pts',(-41.6417694968915,45.6826930774886,-9.02374285555159));
#43506=CARTESIAN_POINT('Ctrl Pts',(-41.6373663141285,45.6854319287458,-9.02500100931356));
#43507=CARTESIAN_POINT('Ctrl Pts',(-41.6304024527032,45.6897635637577,-9.0269908446036));
#43508=CARTESIAN_POINT('Ctrl Pts',(-41.6232495947523,45.693875048068,-9.02887130000535));
#43509=CARTESIAN_POINT('Ctrl Pts',(-41.6158751354701,45.6977294272706,-9.03062816298464));
#43510=CARTESIAN_POINT('Ctrl Pts',(-41.6126791934946,45.6993998375084,-9.03138955197952));
#43511=CARTESIAN_POINT('Ctrl Pts',(-41.6094415604145,45.7010217444016,-9.03212762696971));
#43512=CARTESIAN_POINT('Ctrl Pts',(-41.6061592594077,45.7025911406349,-9.03284077776707));
#43513=CARTESIAN_POINT('Ctrl Pts',(-41.6034837334275,45.703870414043,-9.03342209358249));
#43514=CARTESIAN_POINT('Ctrl Pts',(-41.6007783569267,45.7051148711038,-9.03398688253731));
#43515=CARTESIAN_POINT('Ctrl Pts',(-41.5980413638051,45.7063221317373,-9.03453418418577));
#43516=CARTESIAN_POINT('Ctrl Pts',(-41.5980019984786,45.706339495394,-9.0345420558563));
#43517=CARTESIAN_POINT('Ctrl Pts',(-41.5979626261383,45.7063568515059,-9.03454992397607));
#43518=CARTESIAN_POINT('Ctrl Pts',(-41.5979232468274,45.7063742000469,-9.03455778853368));
#43519=CARTESIAN_POINT('Ctrl Pts',(-41.5951459020883,45.707597758257,-9.03511246019182));
#43520=CARTESIAN_POINT('Ctrl Pts',(-41.5923316176566,45.7087845416927,-9.03564980619242));
#43521=CARTESIAN_POINT('Ctrl Pts',(-41.5895072796806,45.7099207110941,-9.03616371707989));
#43522=CARTESIAN_POINT('Ctrl Pts',(-41.5893316400524,45.7099913670754,-9.03619567611524));
#43523=CARTESIAN_POINT('Ctrl Pts',(-41.5891559504675,45.7100618323782,-9.03622754675872));
#43524=CARTESIAN_POINT('Ctrl Pts',(-41.5889802150548,45.7101321047206,-9.03625932801202));
#43525=CARTESIAN_POINT('Ctrl Pts',(-41.5859677707848,45.7113367083446,-9.03680412005438));
#43526=CARTESIAN_POINT('Ctrl Pts',(-41.5829376777973,45.7124865784167,-9.03732353620516));
#43527=CARTESIAN_POINT('Ctrl Pts',(-41.5798897584861,45.7135797785149,-9.03781686926509));
#43528=CARTESIAN_POINT('Ctrl Pts',(-41.5773971702446,45.7144737974938,-9.03822031701379));
#43529=CARTESIAN_POINT('Ctrl Pts',(-41.5748926681928,45.7153299965749,-9.03860642538735));
#43530=CARTESIAN_POINT('Ctrl Pts',(-41.5723761485838,45.7161472393841,-9.03897472984346));
#43531=CARTESIAN_POINT('Ctrl Pts',(-41.5637163275296,45.7189595268228,-9.04024213529982));
#43532=CARTESIAN_POINT('Ctrl Pts',(-41.5549125428017,45.7213117106978,-9.04129922850373));
#43533=CARTESIAN_POINT('Ctrl Pts',(-41.5459499111192,45.7231558414443,-9.04212652536896));
#43534=CARTESIAN_POINT('Ctrl Pts',(-41.5412041320697,45.7241323221668,-9.04256458511188));
#43535=CARTESIAN_POINT('Ctrl Pts',(-41.5364138582115,45.7249662131444,-9.04293815642914));
#43536=CARTESIAN_POINT('Ctrl Pts',(-41.5315766337177,45.7256494547312,-9.04324396659871));
#43537=CARTESIAN_POINT('Ctrl Pts',(-41.5284280862249,45.7260941764074,-9.04344301831605));
#43538=CARTESIAN_POINT('Ctrl Pts',(-41.5252569314378,45.726475340385,-9.04361348204527));
#43539=CARTESIAN_POINT('Ctrl Pts',(-41.5220695810843,45.7267898067094,-9.043754052548));
#43540=CARTESIAN_POINT('Ctrl Pts',(-41.5209058550529,45.7269046207735,-9.04380537591542));
#43541=CARTESIAN_POINT('Ctrl Pts',(-41.5197405027109,45.727010497462,-9.04385269377214));
#43542=CARTESIAN_POINT('Ctrl Pts',(-41.5185746234031,45.7271072918289,-9.04389594637392));
#43543=CARTESIAN_POINT('Ctrl Pts',(-41.5145270192726,45.727443334571,-9.04404610720827));
#43544=CARTESIAN_POINT('Ctrl Pts',(-41.5104730713073,45.7276699868093,-9.04414730118872));
#43545=CARTESIAN_POINT('Ctrl Pts',(-41.5064127138504,45.7277864292123,-9.04419938129327));
#43546=CARTESIAN_POINT('Ctrl Pts',(-41.5042769250897,45.7278476790845,-9.04422677595079));
#43547=CARTESIAN_POINT('Ctrl Pts',(-41.5021393585781,45.7278783937086,-9.04424052634312));
#43548=CARTESIAN_POINT('Ctrl Pts',(-41.5000000000005,45.7278784053971,-9.04424054928485));
#43549=CARTESIAN_POINT('',(-42.,34.999999994595,-8.54424050588343));
#43550=CARTESIAN_POINT('Ctrl Pts',(-42.,44.902988110908,-8.54424050588343));
#43551=CARTESIAN_POINT('Ctrl Pts',(-42.,45.3322472608192,-8.28784904304297));
#43552=CARTESIAN_POINT('Ctrl Pts',(-42.5,45.3322472608192,-8.28784904304297));
#43553=CARTESIAN_POINT('Ctrl Pts',(-42.,44.9286604045246,-8.56573120990982));
#43554=CARTESIAN_POINT('Ctrl Pts',(-42.0108999708817,45.3453293288621,-8.30975148851287));
#43555=CARTESIAN_POINT('Ctrl Pts',(-42.4999999895151,45.3549342921599,-8.32583242860273));
#43556=CARTESIAN_POINT('Ctrl Pts',(-41.9986214707204,44.9548030624169,-8.58676399861629));
#43557=CARTESIAN_POINT('Ctrl Pts',(-42.0202495830765,45.3594232689745,-8.33310036955195));
#43558=CARTESIAN_POINT('Ctrl Pts',(-42.497242938469,45.3780372174225,-8.36300684416903));
#43559=CARTESIAN_POINT('Ctrl Pts',(-41.9933750391373,45.0079907648268,-8.6279823069976));
#43560=CARTESIAN_POINT('Ctrl Pts',(-42.0351385937246,45.3894870614958,-8.38178650312646));
#43561=CARTESIAN_POINT('Ctrl Pts',(-42.4867500812463,45.4250403043614,-8.43585780778609));
#43562=CARTESIAN_POINT('Ctrl Pts',(-41.9895059097455,45.0350362147751,-8.64816784262251));
#43563=CARTESIAN_POINT('Ctrl Pts',(-42.0407565860507,45.4054076846729,-8.40706640877658));
#43564=CARTESIAN_POINT('Ctrl Pts',(-42.4790118184447,45.4489409335363,-8.47153456853107));
#43565=CARTESIAN_POINT('Ctrl Pts',(-41.979401772684,45.0899811643642,-8.68773568818862));
#43566=CARTESIAN_POINT('Ctrl Pts',(-42.04788943116,45.4390859958032,-8.45907111556724));
#43567=CARTESIAN_POINT('Ctrl Pts',(-42.4588035464137,45.4974969364344,-8.54146843493532));
#43568=CARTESIAN_POINT('Ctrl Pts',(-41.9731666254647,45.1178808703317,-8.70711789767085));
#43569=CARTESIAN_POINT('Ctrl Pts',(-42.0494921140164,45.4567992240739,-8.48575669704656));
#43570=CARTESIAN_POINT('Ctrl Pts',(-42.4463332516214,45.5221524896634,-8.57572536395869));
#43571=CARTESIAN_POINT('Ctrl Pts',(-41.9638964057752,45.1532484070924,-8.73085804517682));
#43572=CARTESIAN_POINT('Ctrl Pts',(-42.0487386127422,45.4802136676926,-8.51997409646917));
#43573=CARTESIAN_POINT('Ctrl Pts',(-42.4277928113774,45.5534075226671,-8.61768469375029));
#43574=CARTESIAN_POINT('Ctrl Pts',(-41.9619682484332,45.1603465096623,-8.7355816459985));
#43575=CARTESIAN_POINT('Ctrl Pts',(-42.0484549927054,45.4849117932795,-8.52679133797057));
#43576=CARTESIAN_POINT('Ctrl Pts',(-42.4239364971452,45.5596802642686,-8.62603338389302));
#43577=CARTESIAN_POINT('Ctrl Pts',(-41.9579625363262,45.1745906511032,-8.74498016260993));
#43578=CARTESIAN_POINT('Ctrl Pts',(-42.0476113931016,45.4944127529898,-8.54047636109722));
#43579=CARTESIAN_POINT('Ctrl Pts',(-42.4159250723737,45.5722681103951,-8.64264471521523));
#43580=CARTESIAN_POINT('Ctrl Pts',(-41.955882303473,45.1817455281307,-8.74966079550314));
#43581=CARTESIAN_POINT('Ctrl Pts',(-42.0470519527415,45.4992210657315,-8.54735241762345));
#43582=CARTESIAN_POINT('Ctrl Pts',(-42.411764606457,45.5785910245723,-8.65091746194013));
#43583=CARTESIAN_POINT('Ctrl Pts',(-41.9494346473223,45.2032149228718,-8.76358766865384));
#43584=CARTESIAN_POINT('Ctrl Pts',(-42.0449628041206,45.5137178535233,-8.56792941843968));
#43585=CARTESIAN_POINT('Ctrl Pts',(-42.3988692956227,45.5975639789771,-8.6755324004288));
#43586=CARTESIAN_POINT('Ctrl Pts',(-41.9448722632192,45.2174978104266,-8.77269577610381));
#43587=CARTESIAN_POINT('Ctrl Pts',(-42.0430249734493,45.5235278259453,-8.58165311177667));
#43588=CARTESIAN_POINT('Ctrl Pts',(-42.3897445259251,45.6101860644684,-8.69163045108915));
#43589=CARTESIAN_POINT('Ctrl Pts',(-41.9304066859268,45.2602328103821,-8.79951026319421));
#43590=CARTESIAN_POINT('Ctrl Pts',(-42.0356031360407,45.5531189722808,-8.62243545445269));
#43591=CARTESIAN_POINT('Ctrl Pts',(-42.3608133728757,45.6479518801124,-8.73902349739317));
#43592=CARTESIAN_POINT('Ctrl Pts',(-41.9197290595943,45.2885738141815,-8.81670858590767));
#43593=CARTESIAN_POINT('Ctrl Pts',(-42.0285011256322,45.573363377834,-8.64954189109913));
#43594=CARTESIAN_POINT('Ctrl Pts',(-42.3394581198824,45.6729974161304,-8.76942053466115));
#43595=CARTESIAN_POINT('Ctrl Pts',(-41.8962822187091,45.3447779229183,-8.84980840543283));
#43596=CARTESIAN_POINT('Ctrl Pts',(-42.0098501467087,45.6143697759043,-8.70284461529763));
#43597=CARTESIAN_POINT('Ctrl Pts',(-42.2925644367244,45.7226661655264,-8.8279225385782));
#43598=CARTESIAN_POINT('Ctrl Pts',(-41.8835140806194,45.3726424029527,-8.86571009100462));
#43599=CARTESIAN_POINT('Ctrl Pts',(-41.9983779043733,45.6351418297266,-8.72908283607111));
#43600=CARTESIAN_POINT('Ctrl Pts',(-42.2670281635762,45.7472905876327,-8.85602784747157));
#43601=CARTESIAN_POINT('Ctrl Pts',(-41.862670707963,45.4138740921654,-8.88858973796334));
#43602=CARTESIAN_POINT('Ctrl Pts',(-41.9776044328624,45.6665359773409,-8.76763025951353));
#43603=CARTESIAN_POINT('Ctrl Pts',(-42.2253414147564,45.7837278959388,-8.8964662890298));
#43604=CARTESIAN_POINT('Ctrl Pts',(-41.8554398788958,45.427522950843,-8.89605366242561));
#43605=CARTESIAN_POINT('Ctrl Pts',(-41.9701420076706,45.6769743994332,-8.78026942647067));
#43606=CARTESIAN_POINT('Ctrl Pts',(-42.2108797593804,45.795789676984,-8.90965834491112));
#43607=CARTESIAN_POINT('Ctrl Pts',(-41.8441404753721,45.4478172893659,-8.90700052899381));
#43608=CARTESIAN_POINT('Ctrl Pts',(-41.958022565088,45.6926462815954,-8.79898741435063));
#43609=CARTESIAN_POINT('Ctrl Pts',(-42.1882809499499,45.8137242094849,-8.92900629222498));
#43610=CARTESIAN_POINT('Ctrl Pts',(-41.8402940153966,45.4545592291316,-8.91061164426722));
#43611=CARTESIAN_POINT('Ctrl Pts',(-41.9538372921188,45.6978624661921,-8.80517489813451));
#43612=CARTESIAN_POINT('Ctrl Pts',(-42.1805880309734,45.8196822021074,-8.93538873003764));
#43613=CARTESIAN_POINT('Ctrl Pts',(-41.8324883720422,45.4679011401808,-8.91770979566791));
#43614=CARTESIAN_POINT('Ctrl Pts',(-41.9452093359132,45.7082222863744,-8.81738175445068));
#43615=CARTESIAN_POINT('Ctrl Pts',(-42.1649767439042,45.8314727289465,-8.9479342988573));
#43616=CARTESIAN_POINT('Ctrl Pts',(-41.8285250186428,45.4745089647429,-8.92120111745386));
#43617=CARTESIAN_POINT('Ctrl Pts',(-41.940763007093,45.7133726477466,-8.82340956419523));
#43618=CARTESIAN_POINT('Ctrl Pts',(-42.1570500375643,45.8373122010236,-8.95410500834317));
#43619=CARTESIAN_POINT('Ctrl Pts',(-41.8083998462294,45.5072149631162,-8.93836914430218));
#43620=CARTESIAN_POINT('Ctrl Pts',(-41.9179983851406,45.7388018091337,-8.85297773751299));
#43621=CARTESIAN_POINT('Ctrl Pts',(-42.1167996913393,45.8662151783001,-8.98444849433146));
#43622=CARTESIAN_POINT('Ctrl Pts',(-41.7913199828142,45.5323245258358,-8.95118532573511));
#43623=CARTESIAN_POINT('Ctrl Pts',(-41.8975757846378,45.7587513033878,-8.87555470746898));
#43624=CARTESIAN_POINT('Ctrl Pts',(-42.0826399682652,45.8884050213045,-9.00710035766719));
#43625=CARTESIAN_POINT('Ctrl Pts',(-41.7549472623746,45.5798301722945,-8.97490663201676));
#43626=CARTESIAN_POINT('Ctrl Pts',(-41.8522755408233,45.7968273270403,-8.91768065668701));
#43627=CARTESIAN_POINT('Ctrl Pts',(-42.0098945221124,45.9303867584722,-9.04902637713643));
#43628=CARTESIAN_POINT('Ctrl Pts',(-41.7356587556976,45.6022335718975,-8.98581453285689));
#43629=CARTESIAN_POINT('Ctrl Pts',(-41.827418348961,45.8150217309514,-8.9373171564491));
#43630=CARTESIAN_POINT('Ctrl Pts',(-41.9713175153897,45.9501851085395,-9.06830547181726));
#43631=CARTESIAN_POINT('Ctrl Pts',(-41.7098586873126,45.6279367771953,-8.99810391954615));
#43632=CARTESIAN_POINT('Ctrl Pts',(-41.7930929437521,45.8361032447929,-8.95964586975483));
#43633=CARTESIAN_POINT('Ctrl Pts',(-41.9197173736266,45.9728995709431,-9.09002623703225));
#43634=CARTESIAN_POINT('Ctrl Pts',(-41.704632773787,45.6329411844467,-9.00048442311758));
#43635=CARTESIAN_POINT('Ctrl Pts',(-41.7861251546753,45.8401999741684,-8.9639626962812));
#43636=CARTESIAN_POINT('Ctrl Pts',(-41.9092655478991,45.9773220695307,-9.09423364209421));
#43637=CARTESIAN_POINT('Ctrl Pts',(-41.6940829685631,45.6426271938172,-9.00507115312237));
#43638=CARTESIAN_POINT('Ctrl Pts',(-41.7719775499116,45.8481422955614,-8.97229352456195));
#43639=CARTESIAN_POINT('Ctrl Pts',(-41.8881659368007,45.9858817996664,-9.10234041840881));
#43640=CARTESIAN_POINT('Ctrl Pts',(-41.6887533114059,45.6473145875886,-9.00728014401976));
#43641=CARTESIAN_POINT('Ctrl Pts',(-41.76478941984,45.8519939510722,-8.97631403485392));
#43642=CARTESIAN_POINT('Ctrl Pts',(-41.877506623199,45.9900241467431,-9.10624468388211));
#43643=CARTESIAN_POINT('Ctrl Pts',(-41.6725947699906,45.6608873717108,-9.01364983853488));
#43644=CARTESIAN_POINT('Ctrl Pts',(-41.7429102615715,45.8631498532122,-8.98790974948757));
#43645=CARTESIAN_POINT('Ctrl Pts',(-41.8451895392067,46.0020187014886,-9.11750274457941));
#43646=CARTESIAN_POINT('Ctrl Pts',(-41.6615966611876,45.6692843712125,-9.01755378461365));
#43647=CARTESIAN_POINT('Ctrl Pts',(-41.7278472754948,45.8700901815488,-8.9950561303503));
#43648=CARTESIAN_POINT('Ctrl Pts',(-41.8231933233325,46.0094393040033,-9.12440274854059));
#43649=CARTESIAN_POINT('Ctrl Pts',(-41.639113172241,45.6846338528735,-9.02464290600063));
#43650=CARTESIAN_POINT('Ctrl Pts',(-41.6968062378558,45.8827994607731,-9.0080542913267));
#43651=CARTESIAN_POINT('Ctrl Pts',(-41.7782263435246,46.0230039638273,-9.13693235132219));
#43652=CARTESIAN_POINT('Ctrl Pts',(-41.6276278973201,45.691586658138,-9.02782822994433));
#43653=CARTESIAN_POINT('Ctrl Pts',(-41.6808195592107,45.8885783031742,-9.01391663064739));
#43654=CARTESIAN_POINT('Ctrl Pts',(-41.7552557956688,46.0291483018663,-9.14256223432903));
#43655=CARTESIAN_POINT('Ctrl Pts',(-41.6099987545451,45.7008008118369,-9.03202812950479));
#43656=CARTESIAN_POINT('Ctrl Pts',(-41.6561159186992,45.8962508251284,-9.02165960285725));
#43657=CARTESIAN_POINT('Ctrl Pts',(-41.7199975085757,46.037291043381,-9.14998530576052));
#43658=CARTESIAN_POINT('Ctrl Pts',(-41.6040554010528,45.7036694039868,-9.03333158983249));
#43659=CARTESIAN_POINT('Ctrl Pts',(-41.6477683894613,45.8986408027904,-9.02406393261697));
#43660=CARTESIAN_POINT('Ctrl Pts',(-41.7081108026102,46.0398260776494,-9.15228910096591));
#43661=CARTESIAN_POINT('Ctrl Pts',(-41.5950343440379,45.707648490221,-9.03513548159103));
#43662=CARTESIAN_POINT('Ctrl Pts',(-41.6350621829909,45.9019591498723,-9.0273943698628));
#43663=CARTESIAN_POINT('Ctrl Pts',(-41.6900686878235,46.0433424799017,-9.15547737091504));
#43664=CARTESIAN_POINT('Ctrl Pts',(-41.5920068986027,45.7089217810477,-9.03571196085561));
#43665=CARTESIAN_POINT('Ctrl Pts',(-41.6307939033919,45.9030212106372,-9.02845888268938));
#43666=CARTESIAN_POINT('Ctrl Pts',(-41.6840137971755,46.0444677133423,-9.1564962658135));
#43667=CARTESIAN_POINT('Ctrl Pts',(-41.5859535254763,45.7113423972445,-9.03680669625905));
#43668=CARTESIAN_POINT('Ctrl Pts',(-41.6222498275285,45.9050409290163,-9.0304810243379));
#43669=CARTESIAN_POINT('Ctrl Pts',(-41.6719070509825,46.0466068628566,-9.15843114693368));
#43670=CARTESIAN_POINT('Ctrl Pts',(-41.5829233752423,45.7124917049892,-9.03732585120345));
#43671=CARTESIAN_POINT('Ctrl Pts',(-41.6179678487693,45.9060003613735,-9.03144043622865));
#43672=CARTESIAN_POINT('Ctrl Pts',(-41.6658467504665,46.047622529863,-9.15934872320473));
#43673=CARTESIAN_POINT('Ctrl Pts',(-41.5556208222111,45.7222843539839,-9.04174501411847));
#43674=CARTESIAN_POINT('Ctrl Pts',(-41.5794217634366,45.9141617518149,-9.03959362376309));
#43675=CARTESIAN_POINT('Ctrl Pts',(-41.6112416445666,46.0562765000394,-9.16715933617831));
#43676=CARTESIAN_POINT('Ctrl Pts',(-41.5311308076983,45.7270775602764,-9.04388233509682));
#43677=CARTESIAN_POINT('Ctrl Pts',(-41.5444292326109,45.9181968905741,-9.04357633437154));
#43678=CARTESIAN_POINT('Ctrl Pts',(-41.5622616154321,46.0605123555124,-9.17093692978999));
#43679=CARTESIAN_POINT('Ctrl Pts',(-41.4940536667479,45.7281408512266,-9.04435790439379));
#43680=CARTESIAN_POINT('Ctrl Pts',(-41.4915166863813,45.9190876289001,-9.04445814124235));
#43681=CARTESIAN_POINT('Ctrl Pts',(-41.488107333478,46.0614520081263,-9.17177746703914));
#43682=CARTESIAN_POINT('Ctrl Pts',(-41.4816374541537,45.7274728039395,-9.04405951499495));
#43683=CARTESIAN_POINT('Ctrl Pts',(-41.4737840688501,45.9185271854623,-9.04390407525488));
#43684=CARTESIAN_POINT('Ctrl Pts',(-41.4632749081632,46.0608616409463,-9.17125008419945));
#43685=CARTESIAN_POINT('Ctrl Pts',(-41.4629246490349,45.7248907522696,-9.0429031920658));
#43686=CARTESIAN_POINT('Ctrl Pts',(-41.4471201591405,45.9163657707925,-9.04176155338066));
#43687=CARTESIAN_POINT('Ctrl Pts',(-41.425849298142,46.0585798274846,-9.16920634795539));
#43688=CARTESIAN_POINT('Ctrl Pts',(-41.4566624705733,45.7237626947943,-9.04239772264832));
#43689=CARTESIAN_POINT('Ctrl Pts',(-41.4382011712065,45.9154212255412,-9.04082471749996));
#43690=CARTESIAN_POINT('Ctrl Pts',(-41.4133249413372,46.0575829397824,-9.16831295915316));
#43691=CARTESIAN_POINT('Ctrl Pts',(-41.4442731608293,45.7210143399589,-9.04116431640955));
#43692=CARTESIAN_POINT('Ctrl Pts',(-41.4205799986544,45.9131217963581,-9.03854049004602));
#43693=CARTESIAN_POINT('Ctrl Pts',(-41.388546321468,46.0551541607308,-9.16613298912151));
#43694=CARTESIAN_POINT('Ctrl Pts',(-41.4381262046785,45.7193922594189,-9.0404355851954));
#43695=CARTESIAN_POINT('Ctrl Pts',(-41.4118473895139,45.911764846025,-9.03719104617774));
#43696=CARTESIAN_POINT('Ctrl Pts',(-41.3762524095784,46.053720694625,-9.16484499548513));
#43697=CARTESIAN_POINT('Ctrl Pts',(-41.407621134817,45.7100931492939,-9.0362495685661));
#43698=CARTESIAN_POINT('Ctrl Pts',(-41.3685291843857,45.9039820475746,-9.02943568588035));
#43699=CARTESIAN_POINT('Ctrl Pts',(-41.3152422687481,46.0455028751849,-9.15744646291901));
#43700=CARTESIAN_POINT('Ctrl Pts',(-41.3839484100396,45.6988653534475,-9.03117626479338));
#43701=CARTESIAN_POINT('Ctrl Pts',(-41.3351481982956,45.8945772852277,-9.02002671647569));
#43702=CARTESIAN_POINT('Ctrl Pts',(-41.2678968207294,46.0355806396204,-9.14847968289344));
#43703=CARTESIAN_POINT('Ctrl Pts',(-41.3551721676721,45.6807380719283,-9.02284347211491));
#43704=CARTESIAN_POINT('Ctrl Pts',(-41.2953272780234,45.8795837361382,-9.00476516996006));
#43705=CARTESIAN_POINT('Ctrl Pts',(-41.2103443351816,46.0195611794421,-9.13375196105432));
#43706=CARTESIAN_POINT('Ctrl Pts',(-41.3494454368654,45.6768975505525,-9.02107227041025));
#43707=CARTESIAN_POINT('Ctrl Pts',(-41.287409656368,45.8764014737269,-9.00151523627819));
#43708=CARTESIAN_POINT('Ctrl Pts',(-41.1988908745363,46.0161672311216,-9.13062146148794));
#43709=CARTESIAN_POINT('Ctrl Pts',(-41.3381720289335,45.6688915109853,-9.01736513631701));
#43710=CARTESIAN_POINT('Ctrl Pts',(-41.2718899027242,45.8697790039318,-8.99472450291166));
#43711=CARTESIAN_POINT('Ctrl Pts',(-41.1763440570616,46.0090921256199,-9.12406932266754));
#43712=CARTESIAN_POINT('Ctrl Pts',(-41.3326168231151,45.6647216906387,-9.01542726254812));
#43713=CARTESIAN_POINT('Ctrl Pts',(-41.2642748270683,45.8663339932396,-8.99117880533118));
#43714=CARTESIAN_POINT('Ctrl Pts',(-41.1652336469978,46.0054071688866,-9.12064423860081));
#43715=CARTESIAN_POINT('Ctrl Pts',(-41.3161815155429,45.6517477750581,-9.00937179381302));
#43716=CARTESIAN_POINT('Ctrl Pts',(-41.241826326959,45.8556226394696,-8.98010650018481));
#43717=CARTESIAN_POINT('Ctrl Pts',(-41.1323630295511,45.9939418469458,-9.10994155647637));
#43718=CARTESIAN_POINT('Ctrl Pts',(-41.3055311846566,45.6424803476347,-9.00501290349459));
#43719=CARTESIAN_POINT('Ctrl Pts',(-41.2274362460732,45.8479980985234,-8.97216285930692));
#43720=CARTESIAN_POINT('Ctrl Pts',(-41.1110623706261,45.985752028998,-9.10223746326134));
#43721=CARTESIAN_POINT('Ctrl Pts',(-41.2744096325773,45.6130614999026,-8.99103607019868));
#43722=CARTESIAN_POINT('Ctrl Pts',(-41.1857604875355,45.8238434014517,-8.9467425861811));
#43723=CARTESIAN_POINT('Ctrl Pts',(-41.0488192625286,45.9597539749973,-9.07753423341684));
#43724=CARTESIAN_POINT('Ctrl Pts',(-41.2547598251768,45.5913023257157,-8.98052231633313));
#43725=CARTESIAN_POINT('Ctrl Pts',(-41.1601629016934,45.8061099177734,-8.92775042784227));
#43726=CARTESIAN_POINT('Ctrl Pts',(-41.0095243303217,45.9405275308553,-9.05895435738375));
#43727=CARTESIAN_POINT('Ctrl Pts',(-41.2360638672433,45.567851127476,-8.96890239236004));
#43728=CARTESIAN_POINT('Ctrl Pts',(-41.1367508806195,45.7873702696317,-8.90717732011608));
#43729=CARTESIAN_POINT('Ctrl Pts',(-40.9721277344869,45.9198006242979,-9.03841423774551));
#43730=CARTESIAN_POINT('Origin',(-39.,48.5946168001447,-6.3392739254555));
#43731=CARTESIAN_POINT('',(-46.,52.2061427793358,-5.15737710185882));
#43732=CARTESIAN_POINT('Origin',(-46.,48.5946168001447,-6.3392739254555));
#43733=CARTESIAN_POINT('Ctrl Pts',(-46.,52.2061427793358,-5.15737710185883));
#43734=CARTESIAN_POINT('Ctrl Pts',(-46.,52.1813102167619,-5.08149615939848));
#43735=CARTESIAN_POINT('Ctrl Pts',(-45.9868485706877,52.1541549603842,-5.00673960430385));
#43736=CARTESIAN_POINT('Ctrl Pts',(-45.9274064730372,52.0781955342347,-4.81574086290611));
#43737=CARTESIAN_POINT('Ctrl Pts',(-45.8652318634837,52.0272394525228,-4.70527038001436));
#43738=CARTESIAN_POINT('Ctrl Pts',(-45.7071137304848,51.9128490522269,-4.48235789714551));
#43739=CARTESIAN_POINT('Ctrl Pts',(-45.6026237298735,51.8461984168199,-4.36873234959023));
#43740=CARTESIAN_POINT('Ctrl Pts',(-45.5017843995202,51.7768809810558,-4.26245040303759));
#43741=CARTESIAN_POINT('Ctrl Pts',(-45.5008921986149,51.7762672711454,-4.26151033429702));
#43742=CARTESIAN_POINT('Ctrl Pts',(-45.5,51.7756531463268,-4.26057054010477));
#43743=CARTESIAN_POINT('Origin',(-45.,48.5946168001447,-6.3392739254555));
#43744=CARTESIAN_POINT('Origin',(-45.5,52.6127679742695,-3.71354333343353));
#43745=CARTESIAN_POINT('Origin',(-46.,52.6127679742695,-3.71354333343353));
#43746=CARTESIAN_POINT('Origin',(-46.,52.6127679742695,-3.71354333343353));
#43747=CARTESIAN_POINT('Origin',(-45.,20.1123922190465,-8.20726109677752));
#43748=CARTESIAN_POINT('Origin',(-45.,19.0050007760892,0.400000000655));
#43749=CARTESIAN_POINT('Origin',(-45.,20.1123922190465,-8.20726109677752));
#43750=CARTESIAN_POINT('',(-45.,47.8027400910494,-6.80733765974042));
#43751=CARTESIAN_POINT('Origin',(-46.,34.999999994595,6.54998265276524E-10));
#43752=CARTESIAN_POINT('',(-46.,39.9275186688271,-2.44326824394971));
#43753=CARTESIAN_POINT('',(-46.,34.9369175583481,-0.136474846523149));
#43754=CARTESIAN_POINT('',(-46.,29.500909160648,-0.099999999345));
#43755=CARTESIAN_POINT('Origin',(-46.,34.999999994595,6.55E-10));
#43756=CARTESIAN_POINT('',(-46.,34.999999994595,-0.099999999345));
#43757=CARTESIAN_POINT('',(-46.,24.0004545494414,0.100000000654999));
#43758=CARTESIAN_POINT('',(-46.,29.0008333858067,0.100000000655));
#43759=CARTESIAN_POINT('',(-46.,34.999999994595,0.100000000655));
#43760=CARTESIAN_POINT('',(-46.,29.4923003031304,2.38017732779692));
#43761=CARTESIAN_POINT('Origin',(-46.,34.999999994595,6.55E-10));
#43762=CARTESIAN_POINT('',(-46.,24.952916660542,4.47840557391373));
#43763=CARTESIAN_POINT('',(-46.,34.9369175583481,-0.13647484652315));
#43764=CARTESIAN_POINT('Origin',(-46.,34.999999994595,6.55E-10));
#43765=CARTESIAN_POINT('Origin',(-46.,34.999999994595,6.55E-10));
#43766=CARTESIAN_POINT('Origin',(-29.,48.5946168001447,-3.5392739254555));
#43767=CARTESIAN_POINT('Origin',(-39.,56.5946168001448,-3.5392739254555));
#43768=CARTESIAN_POINT('Origin',(-33.5,53.0946168001448,-3.5392739254555));
#43769=CARTESIAN_POINT('',(-39.,48.5946168001447,-3.5392739254555));
#43770=CARTESIAN_POINT('Ctrl Pts',(-41.,51.6274934940962,-3.5392739254555));
#43771=CARTESIAN_POINT('Ctrl Pts',(-40.8774289857881,51.6274934940962,-3.5392739254555));
#43772=CARTESIAN_POINT('Ctrl Pts',(-40.7332628863176,51.6566516291422,-3.5392739254555));
#43773=CARTESIAN_POINT('Ctrl Pts',(-40.505929311989,51.7520470879015,-3.5392739254555));
#43774=CARTESIAN_POINT('Ctrl Pts',(-40.3828782109269,51.8356412158619,-3.5392739254555));
#43775=CARTESIAN_POINT('Ctrl Pts',(-40.2076014610043,52.0132462040385,-3.5392739254555));
#43776=CARTESIAN_POINT('Ctrl Pts',(-40.1248075750373,52.1391374121605,-3.5392739254555));
#43777=CARTESIAN_POINT('Ctrl Pts',(-40.0292644975066,52.3726433492684,-3.5392739254555));
#43778=CARTESIAN_POINT('Ctrl Pts',(-40.,52.5218803109357,-3.5392739254555));
#43779=CARTESIAN_POINT('Ctrl Pts',(-40.,52.6486129734088,-3.5392739254555));
#43780=CARTESIAN_POINT('Origin',(-42.,34.999999994595,6.55E-10));
#43781=CARTESIAN_POINT('Origin',(-42.,34.999999994595,6.55E-10));
#43782=CARTESIAN_POINT('Origin',(-42.5,34.999999994595,6.55E-10));
#43783=CARTESIAN_POINT('Origin',(-42.,34.999999994595,6.55E-10));
#43784=CARTESIAN_POINT('',(-42.5,24.5171568688013,0.600000000655));
#43785=CARTESIAN_POINT('Origin',(-42.5,34.999999994595,6.55E-10));
#43786=CARTESIAN_POINT('',(-45.5,24.5171568688013,0.600000000655));
#43787=CARTESIAN_POINT('',(-46.,24.5171568688013,0.600000000655));
#43788=CARTESIAN_POINT('Origin',(-45.5,34.999999994595,6.55E-10));
#43789=CARTESIAN_POINT('Origin',(-42.,34.999999994595,6.55E-10));
#43790=CARTESIAN_POINT('',(-42.,47.8027400910494,-6.80733765974042));
#43791=CARTESIAN_POINT('',(-42.,20.5417843370527,-1.099999999345));
#43792=CARTESIAN_POINT('Origin',(-42.,34.999999994595,6.55E-10));
#43793=CARTESIAN_POINT('',(-42.,28.5937530433762,-1.099999999345));
#43794=CARTESIAN_POINT('',(-42.,29.0300753719553,-1.099999999345));
#43795=CARTESIAN_POINT('Origin',(-42.,34.999999994595,6.55E-10));
#43796=CARTESIAN_POINT('Origin',(-42.,34.999999994595,6.55E-10));
#43797=CARTESIAN_POINT('',(-42.,38.1717829354129,9.48365926152771));
#43798=CARTESIAN_POINT('',(-42.,36.6893998635448,6.27661756768842));
#43799=CARTESIAN_POINT('',(-42.,36.5063304560983,5.88055852351209));
#43800=CARTESIAN_POINT('',(-42.,29.6176568283776,3.64422585000525));
#43801=CARTESIAN_POINT('Origin',(-42.,34.999999994595,6.55E-10));
#43802=CARTESIAN_POINT('',(-42.,26.4133371006572,5.12535075410315));
#43803=CARTESIAN_POINT('',(-42.,25.9224009791377,5.35227496195084));
#43804=CARTESIAN_POINT('Origin',(-42.,34.999999994595,6.55E-10));
#43805=CARTESIAN_POINT('Origin',(-42.,34.999999994595,6.55E-10));
#43806=CARTESIAN_POINT('',(-42.,25.0606841227656,1.100000000655));
#43807=CARTESIAN_POINT('',(-42.,25.0180162238208,1.100000000655));
#43808=CARTESIAN_POINT('',(-42.,25.5003909094963,3.12368808212367));
#43809=CARTESIAN_POINT('Origin',(-42.,34.999999994595,6.55E-10));
#43810=CARTESIAN_POINT('',(-42.,29.1031045477543,1.45841453098734));
#43811=CARTESIAN_POINT('Origin',(-46.,24.5171568688013,0.600000000655));
#43812=CARTESIAN_POINT('',(-42.5,29.0300753719553,0.600000000655));
#43813=CARTESIAN_POINT('',(-45.5,29.0300753719553,0.600000000655));
#43814=CARTESIAN_POINT('',(-42.,29.0300753719553,0.600000000655));
#43815=CARTESIAN_POINT('',(-45.5,24.5171568688013,0.600000000655));
#43816=CARTESIAN_POINT('Origin',(-42.,34.999999994595,6.55E-10));
#43817=CARTESIAN_POINT('Origin',(-42.5,34.999999994595,6.55E-10));
#43818=CARTESIAN_POINT('Origin',(-45.5,34.999999994595,6.55E-10));
#43819=CARTESIAN_POINT('Origin',(-42.,34.999999994595,6.55E-10));
#43820=CARTESIAN_POINT('Origin',(-42.,34.999999994595,6.55E-10));
#43821=CARTESIAN_POINT('Origin',(-42.5,34.999999994595,6.55E-10));
#43822=CARTESIAN_POINT('Origin',(-45.5,34.999999994595,6.55E-10));
#43823=CARTESIAN_POINT('Origin',(-42.,34.999999994595,6.55E-10));
#43824=CARTESIAN_POINT('Ctrl Pts',(-45.5,29.3128914363174,1.91227514988591));
#43825=CARTESIAN_POINT('Ctrl Pts',(-45.5628391134956,29.3128914363174,1.91227514988591));
#43826=CARTESIAN_POINT('Ctrl Pts',(-45.6298331441263,29.3168834840241,1.92427779549175));
#43827=CARTESIAN_POINT('Ctrl Pts',(-45.7530108833858,29.3335483580741,1.97281123155531));
#43828=CARTESIAN_POINT('Ctrl Pts',(-45.8091981254106,29.3462726308219,2.00931537180972));
#43829=CARTESIAN_POINT('Ctrl Pts',(-45.8979247274123,29.3767120398422,2.09299196879008));
#43830=CARTESIAN_POINT('Ctrl Pts',(-45.9363923973194,29.3964723731256,2.14575933493431));
#43831=CARTESIAN_POINT('Ctrl Pts',(-45.9874312621461,29.4417718124439,2.26050976623123));
#43832=CARTESIAN_POINT('Ctrl Pts',(-46.,29.4673632318665,2.32247326594399));
#43833=CARTESIAN_POINT('Ctrl Pts',(-46.,29.4923003031304,2.38017732779691));
#43834=CARTESIAN_POINT('Ctrl Pts',(-46.,29.0008333858068,0.100000000654999));
#43835=CARTESIAN_POINT('Ctrl Pts',(-46.,29.0018807488039,0.162833051853196));
#43836=CARTESIAN_POINT('Ctrl Pts',(-45.987434136778,29.0040858280371,0.229815422305264));
#43837=CARTESIAN_POINT('Ctrl Pts',(-45.9363958048209,29.0100749953873,0.352987712488953));
#43838=CARTESIAN_POINT('Ctrl Pts',(-45.897925533031,29.0138032964881,0.409181248810524));
#43839=CARTESIAN_POINT('Ctrl Pts',(-45.8091901150632,29.0205302518391,0.49791666677831));
#43840=CARTESIAN_POINT('Ctrl Pts',(-45.7529965530102,29.0239694137344,0.536391275967779));
#43841=CARTESIAN_POINT('Ctrl Pts',(-45.6298176902908,29.0287707804367,0.587434063339562));
#43842=CARTESIAN_POINT('Ctrl Pts',(-45.5628292221247,29.0300753719553,0.600000000654999));
#43843=CARTESIAN_POINT('Ctrl Pts',(-45.5,29.0300753719553,0.600000000654999));
#43844=CARTESIAN_POINT('Origin',(-45.5,34.999999994595,6.55E-10));
#43845=CARTESIAN_POINT('Origin',(-45.5,34.999999994595,6.55E-10));
#43846=CARTESIAN_POINT('Ctrl Pts',(-46.,24.952916660542,4.47840557391373));
#43847=CARTESIAN_POINT('Ctrl Pts',(-46.,24.9534438587617,4.47700178764069));
#43848=CARTESIAN_POINT('Ctrl Pts',(-45.9999966732694,24.9539711604922,4.47559803619075));
#43849=CARTESIAN_POINT('Ctrl Pts',(-45.9994155814552,25.000042193889,4.35297758352556));
#43850=CARTESIAN_POINT('Ctrl Pts',(-45.9740798347619,25.0455855649062,4.23423066579828));
#43851=CARTESIAN_POINT('Ctrl Pts',(-45.8905117508397,25.1174860867329,4.04969045435885));
#43852=CARTESIAN_POINT('Ctrl Pts',(-45.8415534230064,25.1451044879621,3.97986335572903));
#43853=CARTESIAN_POINT('Ctrl Pts',(-45.7413191892353,25.1822011485462,3.8867107561863));
#43854=CARTESIAN_POINT('Ctrl Pts',(-45.6923971848574,25.195297523774,3.85407797624252));
#43855=CARTESIAN_POINT('Ctrl Pts',(-45.5936828209341,25.21066817034,3.81586538743094));
#43856=CARTESIAN_POINT('Ctrl Pts',(-45.5474486391928,25.2143573355172,3.80673058592582));
#43857=CARTESIAN_POINT('Ctrl Pts',(-45.5,25.2143573355172,3.80673058592582));
#43858=CARTESIAN_POINT('Ctrl Pts',(-46.,24.0004545494414,0.100000000655013));
#43859=CARTESIAN_POINT('Ctrl Pts',(-46.,24.0015172240447,0.101053058095808));
#43860=CARTESIAN_POINT('Ctrl Pts',(-45.9999966732101,24.0025799776156,0.102106041183611));
#43861=CARTESIAN_POINT('Ctrl Pts',(-45.9996481828921,24.0582582442755,0.157264429326908));
#43862=CARTESIAN_POINT('Ctrl Pts',(-45.9905229793199,24.113427651011,0.211504412924178));
#43863=CARTESIAN_POINT('Ctrl Pts',(-45.9552065634892,24.2178946933341,0.313459887982052));
#43864=CARTESIAN_POINT('Ctrl Pts',(-45.9295269357133,24.2681331179157,0.362125603591196));
#43865=CARTESIAN_POINT('Ctrl Pts',(-45.8607273465329,24.3600964972318,0.450654394481858));
#43866=CARTESIAN_POINT('Ctrl Pts',(-45.8173190858306,24.4027631032684,0.491431360067023));
#43867=CARTESIAN_POINT('Ctrl Pts',(-45.7252137953263,24.4630158614508,0.54876653070038));
#43868=CARTESIAN_POINT('Ctrl Pts',(-45.6810126507288,24.484178630487,0.568815347785938));
#43869=CARTESIAN_POINT('Ctrl Pts',(-45.5900334171141,24.5105597708073,0.593774499405668));
#43870=CARTESIAN_POINT('Ctrl Pts',(-45.5456486747149,24.5171385264558,0.599982678137806));
#43871=CARTESIAN_POINT('Ctrl Pts',(-45.5001267533779,24.5171568560425,0.599999988604697));
#43872=CARTESIAN_POINT('Ctrl Pts',(-45.5000633756126,24.5171568688013,0.600000000654999));
#43873=CARTESIAN_POINT('Ctrl Pts',(-45.5,24.5171568688013,0.600000000654999));
#43874=CARTESIAN_POINT('Origin',(-45.5,34.9369175583481,-0.136474846523149));
#43875=CARTESIAN_POINT('Origin',(-45.5,34.9369175583481,-0.136474846523149));
#43876=CARTESIAN_POINT('Ctrl Pts',(-45.5,40.1413699032525,-3.09294608072936));
#43877=CARTESIAN_POINT('Ctrl Pts',(-45.5491501916832,40.1413699032525,-3.09294608072936));
#43878=CARTESIAN_POINT('Ctrl Pts',(-45.5972692604454,40.138519820516,-3.08364786424418));
#43879=CARTESIAN_POINT('Ctrl Pts',(-45.6941793711978,40.1270402998169,-3.04649616739224));
#43880=CARTESIAN_POINT('Ctrl Pts',(-45.7405959310225,40.1179528663737,-3.01720069323527));
#43881=CARTESIAN_POINT('Ctrl Pts',(-45.8337415969986,40.0922525585882,-2.93547744772848));
#43882=CARTESIAN_POINT('Ctrl Pts',(-45.8761467093307,40.0744137826655,-2.87945196974603));
#43883=CARTESIAN_POINT('Ctrl Pts',(-45.9391011359062,40.0366703300967,-2.76344022534597));
#43884=CARTESIAN_POINT('Ctrl Pts',(-45.961318424291,40.0169300538135,-2.70376918947611));
#43885=CARTESIAN_POINT('Ctrl Pts',(-45.9919234108107,39.9747588404363,-2.57887452839208));
#43886=CARTESIAN_POINT('Ctrl Pts',(-45.9996764174093,39.9520381992281,-2.51291999016442));
#43887=CARTESIAN_POINT('Ctrl Pts',(-45.9999966934192,39.9284920364042,-2.44603148477463));
#43888=CARTESIAN_POINT('Ctrl Pts',(-46.,39.9280054482978,-2.44464982890693));
#43889=CARTESIAN_POINT('Ctrl Pts',(-46.,39.9275186688271,-2.44326824394971));
#43890=CARTESIAN_POINT('Origin',(-45.5,34.999999994595,0.100000000655));
#43891=CARTESIAN_POINT('Origin',(-45.5,34.999999994595,6.55E-10));
#43892=CARTESIAN_POINT('Ctrl Pts',(-45.5,29.0300753719553,-0.599999999345));
#43893=CARTESIAN_POINT('Ctrl Pts',(-45.548970157778,29.0300753719553,-0.599999999345));
#43894=CARTESIAN_POINT('Ctrl Pts',(-45.5969081567834,29.0365711967785,-0.592808580903382));
#43895=CARTESIAN_POINT('Ctrl Pts',(-45.6935221969332,29.0626157928012,-0.564105664860167));
#43896=CARTESIAN_POINT('Ctrl Pts',(-45.7398209612911,29.0831997568478,-0.54147109065902));
#43897=CARTESIAN_POINT('Ctrl Pts',(-45.8328892935188,29.1409993072008,-0.478410110413383));
#43898=CARTESIAN_POINT('Ctrl Pts',(-45.8753161788561,29.1808820841999,-0.435208680228837));
#43899=CARTESIAN_POINT('Ctrl Pts',(-45.9385897729846,29.2644717707674,-0.345802317210053));
#43900=CARTESIAN_POINT('Ctrl Pts',(-45.9609910872763,29.3079608495334,-0.299750899422561));
#43901=CARTESIAN_POINT('Ctrl Pts',(-45.9918589780637,29.3998033012657,-0.203702083584708));
#43902=CARTESIAN_POINT('Ctrl Pts',(-45.9996751413528,29.448752394715,-0.153142830446623));
#43903=CARTESIAN_POINT('Ctrl Pts',(-45.9999966939211,29.498847589825,-0.102099695500558));
#43904=CARTESIAN_POINT('Ctrl Pts',(-46.,29.4998783026423,-0.101049773754294));
#43905=CARTESIAN_POINT('Ctrl Pts',(-46.,29.500909160648,-0.0999999993449992));
#43906=CARTESIAN_POINT('Origin',(-45.5,34.999999994595,-0.099999999345));
#43907=CARTESIAN_POINT('Ctrl Pts',(-45.9555887800306,18.2967958718846,-0.306006949495302));
#43908=CARTESIAN_POINT('Ctrl Pts',(-45.9286742504228,18.3561332001619,-0.365529007853841));
#43909=CARTESIAN_POINT('Ctrl Pts',(-45.8916577250397,18.4215697732152,-0.415449055491825));
#43910=CARTESIAN_POINT('Ctrl Pts',(-45.7584535062404,18.6397957575259,-0.548653274291119));
#43911=CARTESIAN_POINT('Ctrl Pts',(-45.6188300321941,18.8369497329432,-0.599999999344998));
#43912=CARTESIAN_POINT('Ctrl Pts',(-45.5,19.0050007760892,-0.599999999344998));
#43913=CARTESIAN_POINT('Origin',(-39.,20.2255401693197,4.45249206217833));
#43914=CARTESIAN_POINT('',(-39.,20.2255401693197,4.45249206217833));
#43915=CARTESIAN_POINT('Origin',(-46.,19.0050007760892,0.400000000655));
#43916=CARTESIAN_POINT('Origin',(-30.,39.9592920728172,13.6255430020507));
#43917=CARTESIAN_POINT('Origin',(-39.,56.5946168001448,6.5496670161002E-10));
#43918=CARTESIAN_POINT('',(-39.7071067811866,57.3017235813313,0.915815935106727));
#43919=CARTESIAN_POINT('Ctrl Pts',(-40.,56.5946168001448,0.460726074544506));
#43920=CARTESIAN_POINT('Ctrl Pts',(-40.,56.6851510498546,0.524743456443905));
#43921=CARTESIAN_POINT('Ctrl Pts',(-39.9870743510596,56.783707730714,0.594529537273628));
#43922=CARTESIAN_POINT('Ctrl Pts',(-39.9298163989785,56.9760781041861,0.726060874194729));
#43923=CARTESIAN_POINT('Ctrl Pts',(-39.8854254499147,57.0699455247195,0.787701988575014));
#43924=CARTESIAN_POINT('Ctrl Pts',(-39.7965927093604,57.2020671761929,0.865686530039721));
#43925=CARTESIAN_POINT('Ctrl Pts',(-39.7551464473864,57.2536839151314,0.893953570114362));
#43926=CARTESIAN_POINT('Ctrl Pts',(-39.7071067811866,57.3017235813313,0.915815935106716));
#43927=CARTESIAN_POINT('Ctrl Pts',(-39.7071067811866,57.3017235813313,0.915815935106747));
#43928=CARTESIAN_POINT('Ctrl Pts',(-39.6590671149867,57.3497632475312,0.893953570114389));
#43929=CARTESIAN_POINT('Ctrl Pts',(-39.6074503760481,57.3912095095051,0.865686530039736));
#43930=CARTESIAN_POINT('Ctrl Pts',(-39.4753287245747,57.4800422500596,0.787701988575014));
#43931=CARTESIAN_POINT('Ctrl Pts',(-39.3814613040413,57.5244331991233,0.726060874194723));
#43932=CARTESIAN_POINT('Ctrl Pts',(-39.1890909305692,57.5816911512044,0.594529537273623));
#43933=CARTESIAN_POINT('Ctrl Pts',(-39.0905342497097,57.5946168001448,0.524743456443903));
#43934=CARTESIAN_POINT('Ctrl Pts',(-39.,57.5946168001448,0.460726074544505));
#43935=CARTESIAN_POINT('Origin',(-29.,49.0946168001447,0.460726074544506));
#43936=CARTESIAN_POINT('',(-29.,49.0946168001447,0.960726074544506));
#43937=CARTESIAN_POINT('Origin',(-36.7071067811866,49.0946168001449,0.460726074544334));
#43938=CARTESIAN_POINT('Origin',(-41.,34.999999994595,6.54998265276524E-10));
#43939=CARTESIAN_POINT('Ctrl Pts',(-40.9999916854225,51.9933714024979,0.474687470722451));
#43940=CARTESIAN_POINT('Ctrl Pts',(-40.9669669960565,51.9933716766225,0.474687466548977));
#43941=CARTESIAN_POINT('Ctrl Pts',(-40.9012775948277,51.9966387486667,0.4746377262469));
#43942=CARTESIAN_POINT('Ctrl Pts',(-40.8363006666026,52.0063215827071,0.474490566145437));
#43943=CARTESIAN_POINT('Ctrl Pts',(-40.7878360936142,52.01601685831,0.474343539939905));
#43944=CARTESIAN_POINT('Ctrl Pts',(-40.7717013944448,52.0196627095898,0.474288294394399));
#43945=CARTESIAN_POINT('Ctrl Pts',(-40.7398056090422,52.0277029666335,0.474166606459729));
#43946=CARTESIAN_POINT('Ctrl Pts',(-40.6924300624422,52.040902120181,0.473967040272293));
#43947=CARTESIAN_POINT('Ctrl Pts',(-40.6157642654392,52.0684797155497,0.473551566584779));
#43948=CARTESIAN_POINT('Ctrl Pts',(-40.5568449560762,52.0964124422323,0.473133577527132));
#43949=CARTESIAN_POINT('Ctrl Pts',(-40.5135744864942,52.1195975832219,0.472788208703002));
#43950=CARTESIAN_POINT('Ctrl Pts',(-40.4993044370294,52.1276992237301,0.472667764625631));
#43951=CARTESIAN_POINT('Ctrl Pts',(-40.4781338636937,52.1404221344366,0.472479067172326));
#43952=CARTESIAN_POINT('Ctrl Pts',(-40.4711065130498,52.1447644052945,0.472414737515416));
#43953=CARTESIAN_POINT('Ctrl Pts',(-40.4571840957994,52.1536074404532,0.472283888769367));
#43954=CARTESIAN_POINT('Ctrl Pts',(-40.4227223611727,52.1761016382909,0.471951435217613));
#43955=CARTESIAN_POINT('Ctrl Pts',(-40.363742898356,52.220017783896,0.471306160137212));
#43956=CARTESIAN_POINT('Ctrl Pts',(-40.2914457842733,52.2856940685341,0.470351766833669));
#43957=CARTESIAN_POINT('Ctrl Pts',(-40.247486690588,52.3342381117076,0.469654917353387));
#43958=CARTESIAN_POINT('Ctrl Pts',(-40.2213795506908,52.3661134507234,0.469200546860636));
#43959=CARTESIAN_POINT('Ctrl Pts',(-40.216222153751,52.3725716342351,0.469108641273594));
#43960=CARTESIAN_POINT('Ctrl Pts',(-40.2060999842062,52.3855731513054,0.468923937574523));
#43961=CARTESIAN_POINT('Ctrl Pts',(-40.1911870321444,52.4052251480644,0.468645228815098));
#43962=CARTESIAN_POINT('Ctrl Pts',(-40.1582619483118,52.4521166070354,0.467983631257275));
#43963=CARTESIAN_POINT('Ctrl Pts',(-40.1164784540024,52.5220137105018,0.467007786904805));
#43964=CARTESIAN_POINT('Ctrl Pts',(-40.0885974238781,52.5810032526374,0.466196427926919));
#43965=CARTESIAN_POINT('Ctrl Pts',(-40.069805896849,52.6264192897992,0.46557672633137));
#43966=CARTESIAN_POINT('Ctrl Pts',(-40.0638958909063,52.6417539639008,0.465368290852179));
#43967=CARTESIAN_POINT('Ctrl Pts',(-40.0555726258997,52.6650560555401,0.465052833465107));
#43968=CARTESIAN_POINT('Ctrl Pts',(-40.0528914574447,52.6728662080822,0.464947312131413));
#43969=CARTESIAN_POINT('Ctrl Pts',(-40.0477386832659,52.688501047461,0.464736497152779));
#43970=CARTESIAN_POINT('Ctrl Pts',(-40.0353635450435,52.7276744199,0.464209352250129));
#43971=CARTESIAN_POINT('Ctrl Pts',(-40.0175847433647,52.7989519400502,0.463259743685644));
#43972=CARTESIAN_POINT('Ctrl Pts',(-40.0032590220346,52.8955853337854,0.461993031367599));
#43973=CARTESIAN_POINT('Ctrl Pts',(-40.,52.961078630892,0.461148437744956));
#43974=CARTESIAN_POINT('Ctrl Pts',(-40.,52.9941026808875,0.460726074544506));
#43975=CARTESIAN_POINT('Origin',(-29.,48.5946168001447,0.960726074544506));
#43976=CARTESIAN_POINT('',(-39.5,57.0946168001448,0.960726074544506));
#43977=CARTESIAN_POINT('',(-29.,57.0946168001448,0.960726074544506));
#43978=CARTESIAN_POINT('',(-39.5,52.9941026808875,0.960726074544506));
#43979=CARTESIAN_POINT('',(-39.5,52.9743429703744,0.960726074544506));
#43980=CARTESIAN_POINT('Origin',(-41.0008349053211,52.9940758729588,0.960726074536255));
#43981=CARTESIAN_POINT('Origin',(-39.5,34.999999994595,0.460726074544506));
#43982=CARTESIAN_POINT('Origin',(-39.4999999999966,57.0946168001405,0.460726074522097));
#43983=CARTESIAN_POINT('Origin',(-39.5,52.9941026808875,0.460726074544506));
#43984=CARTESIAN_POINT('Origin',(-29.,57.0946168001448,0.460726074544506));
#43985=CARTESIAN_POINT('Ctrl Pts',(-40.0001655039079,53.0123407644378,0.460493170805832));
#43986=CARTESIAN_POINT('Ctrl Pts',(-40.0003984920697,53.012336506285,0.960745122447957));
#43987=CARTESIAN_POINT('Ctrl Pts',(-39.5002292175527,53.0214512149348,0.960726074182035));
#43988=CARTESIAN_POINT('Ctrl Pts',(-39.9994498624972,52.9728908588742,0.460996190252693));
#43989=CARTESIAN_POINT('Ctrl Pts',(-39.9991801743049,52.9729248253368,0.960745093722174));
#43990=CARTESIAN_POINT('Ctrl Pts',(-39.499155759087,52.9622948946583,0.9607260741824));
#43991=CARTESIAN_POINT('Ctrl Pts',(-40.0010599694177,52.9338359806619,0.461499117712378));
#43992=CARTESIAN_POINT('Ctrl Pts',(-40.0002848056282,52.9338282680843,0.960745065037616));
#43993=CARTESIAN_POINT('Ctrl Pts',(-39.5015709557979,52.903731217001,0.960726074182764));
#43994=CARTESIAN_POINT('Ctrl Pts',(-40.0081477928623,52.8624555520283,0.462427261950409));
#43995=CARTESIAN_POINT('Ctrl Pts',(-40.0064631934232,52.8622602496085,0.960745012189611));
#43996=CARTESIAN_POINT('Ctrl Pts',(-39.512202841528,52.7966951634192,0.960726074183437));
#43997=CARTESIAN_POINT('Ctrl Pts',(-40.0129905514434,52.8300215069154,0.462852495681728));
#43998=CARTESIAN_POINT('Ctrl Pts',(-40.0108949524489,52.8297015577819,0.960744988014785));
#43999=CARTESIAN_POINT('Ctrl Pts',(-39.5194670799186,52.7480600167976,0.960726074183745));
#44000=CARTESIAN_POINT('Ctrl Pts',(-40.0258472542811,52.7656933673554,0.463702766417071));
#44001=CARTESIAN_POINT('Ctrl Pts',(-40.0229589514936,52.7650452541844,0.960744939747848));
#44002=CARTESIAN_POINT('Ctrl Pts',(-39.5387523946349,52.6515997894431,0.960726074184361));
#44003=CARTESIAN_POINT('Ctrl Pts',(-40.0338610657608,52.7337992504474,0.464127804316484));
#44004=CARTESIAN_POINT('Ctrl Pts',(-40.0305883230144,52.7329471688104,0.960744915655539));
#44005=CARTESIAN_POINT('Ctrl Pts',(-39.5507732701283,52.6037746745126,0.960726074184669));
#44006=CARTESIAN_POINT('Ctrl Pts',(-40.0459065884668,52.6942769582217,0.464658757667562));
#44007=CARTESIAN_POINT('Ctrl Pts',(-40.0421830649057,52.6931098486124,0.960744885594489));
#44008=CARTESIAN_POINT('Ctrl Pts',(-39.5688417936154,52.5445113921488,0.960726074185053));
#44009=CARTESIAN_POINT('Ctrl Pts',(-40.0484173432833,52.686389808028,0.464764930564257));
#44010=CARTESIAN_POINT('Ctrl Pts',(-40.0446041297497,52.6851598207343,0.9607448795874));
#44011=CARTESIAN_POINT('Ctrl Pts',(-39.5726079746068,52.5326847014799,0.96072607418513));
#44012=CARTESIAN_POINT('Ctrl Pts',(-40.0536442942955,52.6706504884901,0.464977232783128));
#44013=CARTESIAN_POINT('Ctrl Pts',(-40.0496543933496,52.6692900276159,0.960744867580106));
#44014=CARTESIAN_POINT('Ctrl Pts',(-39.5804485047973,52.5090837996536,0.960726074185284));
#44015=CARTESIAN_POINT('Ctrl Pts',(-40.0563645657016,52.6627872826563,0.465083511790395));
#44016=CARTESIAN_POINT('Ctrl Pts',(-40.0522875048945,52.6613591123839,0.960744861571438));
#44017=CARTESIAN_POINT('Ctrl Pts',(-39.5845289653705,52.4972930389892,0.960726074185361));
#44018=CARTESIAN_POINT('Ctrl Pts',(-40.0648010481868,52.6393500297714,0.465400924687527));
#44019=CARTESIAN_POINT('Ctrl Pts',(-40.0604670716587,52.6377151220421,0.960744843634412));
#44020=CARTESIAN_POINT('Ctrl Pts',(-39.5971838533673,52.4621492626542,0.960726074185592));
#44021=CARTESIAN_POINT('Ctrl Pts',(-40.0707911880509,52.623927967324,0.465610636191831));
#44022=CARTESIAN_POINT('Ctrl Pts',(-40.0662935062176,52.6221453256381,0.960744831791026));
#44023=CARTESIAN_POINT('Ctrl Pts',(-39.6061691817211,52.4390241844292,0.960726074185743));
#44024=CARTESIAN_POINT('Ctrl Pts',(-40.0898370304849,52.5782578888926,0.466234080194723));
#44025=CARTESIAN_POINT('Ctrl Pts',(-40.084867712451,52.5760195290014,0.960744796614806));
#44026=CARTESIAN_POINT('Ctrl Pts',(-39.6347383153858,52.3705429448364,0.960726074186195));
#44027=CARTESIAN_POINT('Ctrl Pts',(-40.1039655757069,52.5486045524486,0.466642140861632));
#44028=CARTESIAN_POINT('Ctrl Pts',(-40.0987139813306,52.5460250690031,0.960744773619268));
#44029=CARTESIAN_POINT('Ctrl Pts',(-39.6559314088288,52.3260786404838,0.96072607418649));
#44030=CARTESIAN_POINT('Ctrl Pts',(-40.1350337723299,52.4908561093173,0.467442665085129));
#44031=CARTESIAN_POINT('Ctrl Pts',(-40.1292885679029,52.487546836494,0.960744728569577));
#44032=CARTESIAN_POINT('Ctrl Pts',(-39.702534304357,52.2394869022988,0.960726074187071));
#44033=CARTESIAN_POINT('Ctrl Pts',(-40.1519734728763,52.4627610299867,0.467835129764516));
#44034=CARTESIAN_POINT('Ctrl Pts',(-40.1460151229703,52.4590609364356,0.960744706513894));
#44035=CARTESIAN_POINT('Ctrl Pts',(-39.727944181063,52.19735950989,0.960726074187355));
#44036=CARTESIAN_POINT('Ctrl Pts',(-40.1795147094014,52.421800055698,0.468411323187832));
#44037=CARTESIAN_POINT('Ctrl Pts',(-40.1733008051782,52.4174778892912,0.960744674169833));
#44038=CARTESIAN_POINT('Ctrl Pts',(-39.7692565659718,52.1359404926989,0.960726074187773));
#44039=CARTESIAN_POINT('Ctrl Pts',(-40.1890510386164,52.4083436912061,0.468601298890646));
#44040=CARTESIAN_POINT('Ctrl Pts',(-40.1827597525983,52.4038117349707,0.960744663514773));
#44041=CARTESIAN_POINT('Ctrl Pts',(-39.7835612418075,52.1157633598134,0.96072607418791));
#44042=CARTESIAN_POINT('Ctrl Pts',(-40.203898320647,52.3884600286176,0.468882980831395));
#44043=CARTESIAN_POINT('Ctrl Pts',(-40.1975076720815,52.3836053509173,0.96074464772499));
#44044=CARTESIAN_POINT('Ctrl Pts',(-39.8058324502274,52.0859488816049,0.960726074188115));
#44045=CARTESIAN_POINT('Ctrl Pts',(-40.2089379225118,52.3818823125493,0.468976327560764));
#44046=CARTESIAN_POINT('Ctrl Pts',(-40.2025162200678,52.3769196053701,0.960744642494575));
#44047=CARTESIAN_POINT('Ctrl Pts',(-39.8133919488952,52.076085960794,0.960726074188182));
#44048=CARTESIAN_POINT('Ctrl Pts',(-40.2192001688965,52.3688283470369,0.469161897284951));
#44049=CARTESIAN_POINT('Ctrl Pts',(-40.2127215810503,52.3636476684092,0.960744632100017));
#44050=CARTESIAN_POINT('Ctrl Pts',(-39.8287855156091,52.0565122835928,0.960726074188316));
#44051=CARTESIAN_POINT('Ctrl Pts',(-40.2244232075698,52.3623522299886,0.469254119011349));
#44052=CARTESIAN_POINT('Ctrl Pts',(-40.2179187794572,52.3570615644569,0.960744626935923));
#44053=CARTESIAN_POINT('Ctrl Pts',(-39.8366201735086,52.0468017246971,0.960726074188384));
#44054=CARTESIAN_POINT('Ctrl Pts',(-40.2508489212739,52.3304076335106,0.469709778885052));
#44055=CARTESIAN_POINT('Ctrl Pts',(-40.2442221313025,52.3245746168839,0.960744601435455));
#44056=CARTESIAN_POINT('Ctrl Pts',(-39.8762592480715,51.9989027144972,0.960726074188714));
#44057=CARTESIAN_POINT('Ctrl Pts',(-40.273095635695,52.3060951210873,0.470059023733022));
#44058=CARTESIAN_POINT('Ctrl Pts',(-40.2664202498769,52.2998131605779,0.960744581909348));
#44059=CARTESIAN_POINT('Ctrl Pts',(-39.9096297458151,51.9624477101716,0.960726074188967));
#44060=CARTESIAN_POINT('Ctrl Pts',(-40.3197348873262,52.2598817711329,0.47072674893928));
#44061=CARTESIAN_POINT('Ctrl Pts',(-40.3130496584301,52.2527055307459,0.960744544620133));
#44062=CARTESIAN_POINT('Ctrl Pts',(-39.9795895104191,51.8931540832812,0.96072607418945));
#44063=CARTESIAN_POINT('Ctrl Pts',(-40.3441275914038,52.2379811214821,0.471045228543483));
#44064=CARTESIAN_POINT('Ctrl Pts',(-40.3374810791704,52.2303564867772,0.960744526854748));
#44065=CARTESIAN_POINT('Ctrl Pts',(-40.0161790302021,51.8603157450578,0.960726074189681));
#44066=CARTESIAN_POINT('Ctrl Pts',(-40.3950567662191,52.1965892330283,0.471650299906407));
#44067=CARTESIAN_POINT('Ctrl Pts',(-40.3885742287628,52.1880843837587,0.96074449313787));
#44068=CARTESIAN_POINT('Ctrl Pts',(-40.0925737593492,51.7982519901567,0.960726074190119));
#44069=CARTESIAN_POINT('Ctrl Pts',(-40.4215930942303,52.1770978340976,0.471936895541539));
#44070=CARTESIAN_POINT('Ctrl Pts',(-40.4152361106502,52.168158359676,0.960744477184023));
#44071=CARTESIAN_POINT('Ctrl Pts',(-40.1323787528732,51.7690263311577,0.960726074190327));
#44072=CARTESIAN_POINT('Ctrl Pts',(-40.4630511915683,52.1497192822008,0.472341311397696));
#44073=CARTESIAN_POINT('Ctrl Pts',(-40.4569521385459,52.1401467612328,0.960744454689427));
#44074=CARTESIAN_POINT('Ctrl Pts',(-40.1945666842034,51.7279746912277,0.96072607419062));
#44075=CARTESIAN_POINT('Ctrl Pts',(-40.4771781181886,52.1408868781905,0.472472109426542));
#44076=CARTESIAN_POINT('Ctrl Pts',(-40.4711742927655,52.1311074238323,0.960744447418406));
#44077=CARTESIAN_POINT('Ctrl Pts',(-40.2157573411748,51.7147313274549,0.960726074190715));
#44078=CARTESIAN_POINT('Ctrl Pts',(-40.5056906476565,52.1240325721919,0.47272224767737));
#44079=CARTESIAN_POINT('Ctrl Pts',(-40.4998960757661,52.113852479979,0.960744433519271));
#44080=CARTESIAN_POINT('Ctrl Pts',(-40.2585266732872,51.689459904419,0.960726074190896));
#44081=CARTESIAN_POINT('Ctrl Pts',(-40.5201047475496,52.1159897576834,0.472841895424202));
#44082=CARTESIAN_POINT('Ctrl Pts',(-40.514424530058,52.1056151429109,0.960744426873757));
#44083=CARTESIAN_POINT('Ctrl Pts',(-40.2801480959472,51.6774004912111,0.960726074190983));
#44084=CARTESIAN_POINT('Ctrl Pts',(-40.5638122296279,52.0929940680948,0.473184660310897));
#44085=CARTESIAN_POINT('Ctrl Pts',(-40.5584969221185,52.0820589039531,0.96074440784537));
#44086=CARTESIAN_POINT('Ctrl Pts',(-40.345710143499,51.6429207424569,0.960726074191231));
#44087=CARTESIAN_POINT('Ctrl Pts',(-40.5935696830967,52.0791712433114,0.473391632961349));
#44088=CARTESIAN_POINT('Ctrl Pts',(-40.588538086652,52.0678858991667,0.960744396362926));
#44089=CARTESIAN_POINT('Ctrl Pts',(-40.3903468851132,51.6221948521615,0.960726074191381));
#44090=CARTESIAN_POINT('Ctrl Pts',(-40.6543065460004,52.0545011905415,0.4737621108513));
#44091=CARTESIAN_POINT('Ctrl Pts',(-40.6499035064575,52.0425809534879,0.960744375822678));
#44092=CARTESIAN_POINT('Ctrl Pts',(-40.4814533235621,51.5852047365437,0.96072607419165));
#44093=CARTESIAN_POINT('Ctrl Pts',(-40.6852859475085,52.043653943586,0.47392561750322));
#44094=CARTESIAN_POINT('Ctrl Pts',(-40.6812299251525,52.0314467950658,0.960744366763052));
#44095=CARTESIAN_POINT('Ctrl Pts',(-40.5279230084688,51.5689404826149,0.960726074191768));
#44096=CARTESIAN_POINT('Ctrl Pts',(-40.7326861808497,52.0296505042667,0.474137149769106));
#44097=CARTESIAN_POINT('Ctrl Pts',(-40.7291925714429,52.0170682302869,0.960744355047342));
#44098=CARTESIAN_POINT('Ctrl Pts',(-40.5990242502966,51.5479438967512,0.960726074191921));
#44099=CARTESIAN_POINT('Ctrl Pts',(-40.7486417259643,52.0253612757894,0.474202030566825));
#44100=CARTESIAN_POINT('Ctrl Pts',(-40.7453413637245,52.0126633195588,0.960744351455017));
#44101=CARTESIAN_POINT('Ctrl Pts',(-40.6229578676032,51.5415126836689,0.960726074191969));
#44102=CARTESIAN_POINT('Ctrl Pts',(-40.772812741707,52.0195062621464,0.474290680866358));
#44103=CARTESIAN_POINT('Ctrl Pts',(-40.7698118586169,52.0066494175163,0.960744346547479));
#44104=CARTESIAN_POINT('Ctrl Pts',(-40.6592148458315,51.5327337612339,0.960726074192033));
#44105=CARTESIAN_POINT('Ctrl Pts',(-40.7809209123333,52.0176487217575,0.474318821429952));
#44106=CARTESIAN_POINT('Ctrl Pts',(-40.778021312729,52.0047413385575,0.960744344989861));
#44107=CARTESIAN_POINT('Ctrl Pts',(-40.6713772541575,51.5299485927647,0.960726074192054));
#44108=CARTESIAN_POINT('Ctrl Pts',(-40.7971478395831,52.0141437354624,0.474371943666935));
#44109=CARTESIAN_POINT('Ctrl Pts',(-40.7944527664113,52.0011407470928,0.960744342049743));
#44110=CARTESIAN_POINT('Ctrl Pts',(-40.6957179497932,51.5246932689571,0.960726074192092));
#44111=CARTESIAN_POINT('Ctrl Pts',(-40.8052667802835,52.0124958472928,0.474396931937503));
#44112=CARTESIAN_POINT('Ctrl Pts',(-40.8026749958654,51.9994477605747,0.960744340666859));
#44113=CARTESIAN_POINT('Ctrl Pts',(-40.7078965135666,51.5222224521958,0.96072607419211));
#44114=CARTESIAN_POINT('Ctrl Pts',(-40.8458885680889,52.0047736588639,0.474514075775359));
#44115=CARTESIAN_POINT('Ctrl Pts',(-40.843814734944,51.9915143162406,0.960744334184926));
#44116=CARTESIAN_POINT('Ctrl Pts',(-40.768829958314,51.5106439255071,0.960726074192195));
#44117=CARTESIAN_POINT('Ctrl Pts',(-40.878472462022,52.0002472210685,0.474582886620358));
#44118=CARTESIAN_POINT('Ctrl Pts',(-40.8768310261112,51.986861668354,0.960744330378307));
#44119=CARTESIAN_POINT('Ctrl Pts',(-40.8177064113942,51.5038570687547,0.960726074192245));
#44120=CARTESIAN_POINT('Ctrl Pts',(-40.9438088155039,51.9944136675709,0.47467159909151));
#44121=CARTESIAN_POINT('Ctrl Pts',(-40.9430436333268,51.9808656960017,0.960744325471528));
#44122=CARTESIAN_POINT('Ctrl Pts',(-40.9157121683823,51.4951103457,0.960726074192309));
#44123=CARTESIAN_POINT('Ctrl Pts',(-40.9765613745278,51.9931067249951,0.474691498565247));
#44124=CARTESIAN_POINT('Ctrl Pts',(-40.9762432211227,51.9795219679182,0.960744324371349));
#44125=CARTESIAN_POINT('Ctrl Pts',(-40.9648416217445,51.4931507434584,0.960726074192323));
#44126=CARTESIAN_POINT('Ctrl Pts',(-41.0093983575033,51.9934156040182,0.474686798057427));
#44127=CARTESIAN_POINT('Ctrl Pts',(-41.0095260061652,51.9798394813421,0.960744324630973));
#44128=CARTESIAN_POINT('Ctrl Pts',(-41.0140977126992,51.4936138694024,0.96072607419232));
#44129=CARTESIAN_POINT('Ctrl Pts',(-39.0000040107747,39.1144560173486,15.9767070126905));
#44130=CARTESIAN_POINT('Ctrl Pts',(-38.997993285275,39.2396510906292,16.4628478279265));
#44131=CARTESIAN_POINT('Ctrl Pts',(-39.5,39.2396510906291,16.4628478279265));
#44132=CARTESIAN_POINT('Ctrl Pts',(-38.9999710932286,39.1281993640875,15.9816539819137));
#44133=CARTESIAN_POINT('Ctrl Pts',(-39.0061770165812,39.2517434266058,16.4597337088979));
#44134=CARTESIAN_POINT('Ctrl Pts',(-39.4999999961727,39.2572581017962,16.4583135222598));
#44135=CARTESIAN_POINT('Ctrl Pts',(-38.9999389637471,39.1421528140174,15.9865420342591));
#44136=CARTESIAN_POINT('Ctrl Pts',(-39.014035614548,39.2643832154332,16.4564671712221));
#44137=CARTESIAN_POINT('Ctrl Pts',(-39.499705301717,39.2748828882628,16.4537445183042));
#44138=CARTESIAN_POINT('Ctrl Pts',(-38.9998764799205,39.1704877658621,15.9961825392357));
#44139=CARTESIAN_POINT('Ctrl Pts',(-39.0289560950027,39.2904676116262,16.449694614346));
#44140=CARTESIAN_POINT('Ctrl Pts',(-39.4985567623278,39.3101653714108,16.4445372951836));
#44141=CARTESIAN_POINT('Ctrl Pts',(-38.9998460867676,39.1848893574197,16.0009413430847));
#44142=CARTESIAN_POINT('Ctrl Pts',(-39.0360421116469,39.3039238546721,16.4461859930947));
#44143=CARTESIAN_POINT('Ctrl Pts',(-39.4977012327184,39.3278472445554,16.4398926700023));
#44144=CARTESIAN_POINT('Ctrl Pts',(-38.9997581301385,39.2285967746172,16.0149383729164));
#44145=CARTESIAN_POINT('Ctrl Pts',(-39.0559248124238,39.344910686845,16.4354437398195));
#44146=CARTESIAN_POINT('Ctrl Pts',(-39.4943483441076,39.3807573812163,16.425903199997));
#44147=CARTESIAN_POINT('Ctrl Pts',(-38.9997039330361,39.2583318414788,16.0238756193564));
#44148=CARTESIAN_POINT('Ctrl Pts',(-39.0677029509203,39.3735823596466,16.4278595602795));
#44149=CARTESIAN_POINT('Ctrl Pts',(-39.4910758730554,39.4157676793138,16.4165250387018));
#44150=CARTESIAN_POINT('Ctrl Pts',(-38.999604938088,39.3190178033854,16.0408596441778));
#44151=CARTESIAN_POINT('Ctrl Pts',(-39.0882518025141,39.4325885301134,16.412067946938));
#44152=CARTESIAN_POINT('Ctrl Pts',(-39.4827310120233,39.4853254063385,16.3976569833155));
#44153=CARTESIAN_POINT('Ctrl Pts',(-38.9995601408619,39.3499685976509,16.0489061580615));
#44154=CARTESIAN_POINT('Ctrl Pts',(-39.0971196495093,39.4629323923524,16.4038627674137));
#44155=CARTESIAN_POINT('Ctrl Pts',(-39.477657772467,39.5198726423859,16.3881671255767));
#44156=CARTESIAN_POINT('Ctrl Pts',(-38.9994801961035,39.4130852578651,16.0639945121934));
#44157=CARTESIAN_POINT('Ctrl Pts',(-39.1121948841364,39.5248397888183,16.3869197775902));
#44158=CARTESIAN_POINT('Ctrl Pts',(-39.4659272469331,39.5885541732129,16.3690696448498));
#44159=CARTESIAN_POINT('Ctrl Pts',(-38.9994450516092,39.4452510448586,16.0710360960569));
#44160=CARTESIAN_POINT('Ctrl Pts',(-39.1184775000691,39.5564256521688,16.378180606244));
#44161=CARTESIAN_POINT('Ctrl Pts',(-39.459269437904,39.6226883492881,16.3594620443941));
#44162=CARTESIAN_POINT('Ctrl Pts',(-38.9993541639804,39.5435429335581,16.0904717711952));
#44163=CARTESIAN_POINT('Ctrl Pts',(-39.1336266951939,39.6515152942701,16.3515497917151));
#44164=CARTESIAN_POINT('Ctrl Pts',(-39.4371887494363,39.7245336577965,16.3304551567704));
#44165=CARTESIAN_POINT('Ctrl Pts',(-38.9993130686179,39.61146453535,16.1011742849298));
#44166=CARTESIAN_POINT('Ctrl Pts',(-39.1394434604447,39.7175866597975,16.3326419457149));
#44167=CARTESIAN_POINT('Ctrl Pts',(-39.4196659843394,39.7916893166733,16.3108717173562));
#44168=CARTESIAN_POINT('Ctrl Pts',(-38.9992682955953,39.7516550808854,16.117053677644));
#44169=CARTESIAN_POINT('Ctrl Pts',(-39.1435098339892,39.8515050401373,16.2933507973697));
#44170=CARTESIAN_POINT('Ctrl Pts',(-39.3801865982225,39.9247885133103,16.2711794528008));
#44171=CARTESIAN_POINT('Ctrl Pts',(-38.9992646285835,39.8239232615503,16.1222252243025));
#44172=CARTESIAN_POINT('Ctrl Pts',(-39.1420289111712,39.9196949489101,16.272899676181));
#44173=CARTESIAN_POINT('Ctrl Pts',(-39.3582250294553,39.9907309434165,16.2510708476132));
#44174=CARTESIAN_POINT('Ctrl Pts',(-38.9992908400457,39.9719736471985,16.1260514269948));
#44175=CARTESIAN_POINT('Ctrl Pts',(-39.1333004854831,40.0568779685301,16.2307569206561));
#44176=CARTESIAN_POINT('Ctrl Pts',(-39.3108390135054,40.1216262610997,16.2102943675883));
#44177=CARTESIAN_POINT('Ctrl Pts',(-38.9993206376677,40.0473915068889,16.1246923030909));
#44178=CARTESIAN_POINT('Ctrl Pts',(-39.1262064141833,40.1259439037555,16.2090697109808));
#44179=CARTESIAN_POINT('Ctrl Pts',(-39.2855296954197,40.1862633392644,16.1897252160385));
#44180=CARTESIAN_POINT('Ctrl Pts',(-38.9994069311823,40.1999218820111,16.1148017033617));
#44181=CARTESIAN_POINT('Ctrl Pts',(-39.1079941481566,40.2637234010117,16.1648101024219));
#44182=CARTESIAN_POINT('Ctrl Pts',(-39.2325813022676,40.3142937443227,16.1481519683413));
#44183=CARTESIAN_POINT('Ctrl Pts',(-38.9994634274222,40.2770321041362,16.1062664623901));
#44184=CARTESIAN_POINT('Ctrl Pts',(-39.0968995045256,40.3328826748058,16.142114510182));
#44185=CARTESIAN_POINT('Ctrl Pts',(-39.2049393098256,40.3776888833517,16.1271472128044));
#44186=CARTESIAN_POINT('Ctrl Pts',(-38.9995951129803,40.4316194825974,16.081643859639));
#44187=CARTESIAN_POINT('Ctrl Pts',(-39.072159950563,40.4706330784677,16.095916469794));
#44188=CARTESIAN_POINT('Ctrl Pts',(-39.1481308710056,40.5035902044287,16.0846171794634));
#44189=CARTESIAN_POINT('Ctrl Pts',(-38.999670291757,40.5090898760604,16.0655543496676));
#44190=CARTESIAN_POINT('Ctrl Pts',(-39.0584715863085,40.5396732906564,16.072276576533));
#44191=CARTESIAN_POINT('Ctrl Pts',(-39.1189633371598,40.5660959131574,16.0630920071615));
#44192=CARTESIAN_POINT('Ctrl Pts',(-38.9997902995226,40.6244575672009,16.0357256794342));
#44193=CARTESIAN_POINT('Ctrl Pts',(-39.0370060054887,40.6428892089116,16.0361908002652));
#44194=CARTESIAN_POINT('Ctrl Pts',(-39.0746438817091,40.6594331070692,16.0303432281553));
#44195=CARTESIAN_POINT('Ctrl Pts',(-38.9998315025215,40.6627730639081,16.024836482104));
#44196=CARTESIAN_POINT('Ctrl Pts',(-39.0296982884772,40.6772372709639,16.0240596836177));
#44197=CARTESIAN_POINT('Ctrl Pts',(-39.0597758040782,40.6904751380211,16.0193500439252));
#44198=CARTESIAN_POINT('Ctrl Pts',(-38.9998942165126,40.7198948523673,16.0071060901951));
#44199=CARTESIAN_POINT('Ctrl Pts',(-39.0186217778953,40.7286878641882,16.0057033726188));
#44200=CARTESIAN_POINT('Ctrl Pts',(-39.0374020341813,40.7369624565466,16.002735157554));
#44201=CARTESIAN_POINT('Ctrl Pts',(-38.9999152726188,40.7388768849487,16.0009633713224));
#44202=CARTESIAN_POINT('Ctrl Pts',(-39.014910542557,40.7458261614915,15.9995581052332));
#44203=CARTESIAN_POINT('Ctrl Pts',(-39.0299321594339,40.7524456017426,15.9971760044345));
#44204=CARTESIAN_POINT('Ctrl Pts',(-38.9999575371806,40.7767006320785,15.9882187582803));
#44205=CARTESIAN_POINT('Ctrl Pts',(-39.0074696557041,40.7800779010963,15.9872148913379));
#44206=CARTESIAN_POINT('Ctrl Pts',(-39.0149802525177,40.7833915593417,15.986014280891));
#44207=CARTESIAN_POINT('Ctrl Pts',(-38.9999787159053,40.7955159485185,15.9816268333025));
#44208=CARTESIAN_POINT('Ctrl Pts',(-39.0037437085471,40.7971742516858,15.9810232603102));
#44209=CARTESIAN_POINT('Ctrl Pts',(-39.0075087112142,40.798832545426,15.9804196907491));
#44210=CARTESIAN_POINT('Ctrl Pts',(-39.,40.8143424311314,15.9747745540155));
#44211=CARTESIAN_POINT('Ctrl Pts',(-39.,40.8143424311314,15.9747745540155));
#44212=CARTESIAN_POINT('Ctrl Pts',(-39.,40.8143424311314,15.9747745540155));
#44213=CARTESIAN_POINT('Origin',(-33.5,53.0946168001448,6.54972098527501E-10));
#44214=CARTESIAN_POINT('Origin',(-39.,34.999999994595,6.54998265276524E-10));
#44215=CARTESIAN_POINT('',(-39.,34.999999994595,-5.04750793782168));
#44216=CARTESIAN_POINT('',(-39.,35.0898188972248,14.8657974082861));
#44217=CARTESIAN_POINT('Origin',(-35.3179607461319,20.7255401693197,-5.04750793782167));
#44218=CARTESIAN_POINT('Origin',(-42.5,34.8957733482214,1.2045349051092));
#44219=CARTESIAN_POINT('Ctrl Pts',(-42.5,25.7126140905746,4.89841434305228));
#44220=CARTESIAN_POINT('Ctrl Pts',(-42.4544360876625,25.7126140905746,4.89841434305228));
#44221=CARTESIAN_POINT('Ctrl Pts',(-42.4099205589807,25.7211751731272,4.90131450985059));
#44222=CARTESIAN_POINT('Ctrl Pts',(-42.3189430447185,25.7556046238125,4.91292843604643));
#44223=CARTESIAN_POINT('Ctrl Pts',(-42.2748783192192,25.7831784389946,4.92220957382935));
#44224=CARTESIAN_POINT('Ctrl Pts',(-42.1833702395799,25.8618864121522,4.94850465259141));
#44225=CARTESIAN_POINT('Ctrl Pts',(-42.1405089721587,25.9175895123965,4.96697887534569));
#44226=CARTESIAN_POINT('Ctrl Pts',(-42.0712695189332,26.0405218463918,5.00723555150006));
#44227=CARTESIAN_POINT('Ctrl Pts',(-42.0453333388046,26.1092745195586,5.0294917844871));
#44228=CARTESIAN_POINT('Ctrl Pts',(-42.009448637647,26.2541174515733,5.07570493574361));
#44229=CARTESIAN_POINT('Ctrl Pts',(-42.0003510591406,26.3317096755902,5.10009922095507));
#44230=CARTESIAN_POINT('Ctrl Pts',(-42.0000033224979,26.4103312392474,5.12442130473777));
#44231=CARTESIAN_POINT('Ctrl Pts',(-42.,26.4118341518126,5.12488609601442));
#44232=CARTESIAN_POINT('Ctrl Pts',(-42.,26.4133371006572,5.12535075410316));
#44233=CARTESIAN_POINT('Ctrl Pts',(-42.5,29.807193045783,3.00578708432712));
#44234=CARTESIAN_POINT('Ctrl Pts',(-42.4826491826238,29.807193045783,3.00578708432712));
#44235=CARTESIAN_POINT('Ctrl Pts',(-42.4652566053828,29.8068240402059,3.00695243590386));
#44236=CARTESIAN_POINT('Ctrl Pts',(-42.3984104029602,29.8039651162076,3.01599095899508));
#44237=CARTESIAN_POINT('Ctrl Pts',(-42.3512786216694,29.7989069718977,3.03197933804397));
#44238=CARTESIAN_POINT('Ctrl Pts',(-42.2553373204745,29.7827689996808,3.08348287759294));
#44239=CARTESIAN_POINT('Ctrl Pts',(-42.2093703460395,29.7709244144044,3.12153688374801));
#44240=CARTESIAN_POINT('Ctrl Pts',(-42.1185333929893,29.7396094754438,3.2237433121557));
#44241=CARTESIAN_POINT('Ctrl Pts',(-42.0788703599454,29.7189044820864,3.29243451923833));
#44242=CARTESIAN_POINT('Ctrl Pts',(-42.0174426176904,29.6718912445443,3.45220337209255));
#44243=CARTESIAN_POINT('Ctrl Pts',(-42.0004779950666,29.6448701695635,3.5464777915612));
#44244=CARTESIAN_POINT('Ctrl Pts',(-42.0000033202246,29.6183969280026,3.64156592368197));
#44245=CARTESIAN_POINT('Ctrl Pts',(-42.,29.6180268093032,3.64289586884436));
#44246=CARTESIAN_POINT('Ctrl Pts',(-42.,29.6176568283776,3.64422585000526));
#44247=CARTESIAN_POINT('Origin',(-42.5,34.2321258407597,0.960461174773771));
#44248=CARTESIAN_POINT('Ctrl Pts',(-42.,38.1717829354129,9.48365926152771));
#44249=CARTESIAN_POINT('Ctrl Pts',(-42.,38.1732312920561,9.48428452066275));
#44250=CARTESIAN_POINT('Ctrl Pts',(-42.0000033223958,38.1746797081854,9.48490965401909));
#44251=CARTESIAN_POINT('Ctrl Pts',(-42.0003519017721,38.2506410915851,9.51768648885896));
#44252=CARTESIAN_POINT('Ctrl Pts',(-42.0094939504563,38.3258766921555,9.54973837417019));
#44253=CARTESIAN_POINT('Ctrl Pts',(-42.0455618257965,38.466697942878,9.60902145670787));
#44254=CARTESIAN_POINT('Ctrl Pts',(-42.0716251146577,38.5337398417288,9.63690992139051));
#44255=CARTESIAN_POINT('Ctrl Pts',(-42.1410737799586,38.6535794559786,9.68628167508754));
#44256=CARTESIAN_POINT('Ctrl Pts',(-42.1839363914962,38.7079106249327,9.70842519372085));
#44257=CARTESIAN_POINT('Ctrl Pts',(-42.2753727862073,38.7847364479714,9.73954067383277));
#44258=CARTESIAN_POINT('Ctrl Pts',(-42.3193584730603,38.8116785080646,9.75038190390326));
#44259=CARTESIAN_POINT('Ctrl Pts',(-42.4101445564636,38.8453212413905,9.76389368020581));
#44260=CARTESIAN_POINT('Ctrl Pts',(-42.4545481243919,38.8536933372283,9.7672436047095));
#44261=CARTESIAN_POINT('Ctrl Pts',(-42.5,38.8536933372283,9.7672436047095));
#44262=CARTESIAN_POINT('Ctrl Pts',(-42.,36.6893998635448,6.27661756768842));
#44263=CARTESIAN_POINT('Ctrl Pts',(-42.,36.6899827586311,6.27537117437134));
#44264=CARTESIAN_POINT('Ctrl Pts',(-42.0000033204919,36.6905655271129,6.27412471941368));
#44265=CARTESIAN_POINT('Ctrl Pts',(-42.0004662363704,36.731188818525,6.18721435730615));
#44266=CARTESIAN_POINT('Ctrl Pts',(-42.0165992209749,36.7708781213347,6.10065128632007));
#44267=CARTESIAN_POINT('Ctrl Pts',(-42.0758441660175,36.8385492890082,5.95035856080122));
#44268=CARTESIAN_POINT('Ctrl Pts',(-42.1151456113166,36.8678277552101,5.88417276489002));
#44269=CARTESIAN_POINT('Ctrl Pts',(-42.2056695167071,36.911145913672,5.78502383058571));
#44270=CARTESIAN_POINT('Ctrl Pts',(-42.2516602512676,36.9271867915193,5.74785640724485));
#44271=CARTESIAN_POINT('Ctrl Pts',(-42.3477951889101,36.948899442058,5.69727843691421));
#44272=CARTESIAN_POINT('Ctrl Pts',(-42.3950686181708,36.9556558410848,5.68141836584189));
#44273=CARTESIAN_POINT('Ctrl Pts',(-42.4631644468274,36.959654908806,5.67203138674556));
#44274=CARTESIAN_POINT('Ctrl Pts',(-42.4816022135789,36.9601910749969,5.67077163494895));
#44275=CARTESIAN_POINT('Ctrl Pts',(-42.5,36.9601910749969,5.67077163494895));
#44276=CARTESIAN_POINT('Ctrl Pts',(-39.5,42.3343534352396,15.3364682905744));
#44277=CARTESIAN_POINT('Ctrl Pts',(-38.9979932851518,42.3343534352396,15.3364682905744));
#44278=CARTESIAN_POINT('Ctrl Pts',(-39.0000040107752,42.1177731327825,14.8835889784804));
#44279=CARTESIAN_POINT('Ctrl Pts',(-39.4999999961727,42.3179510866741,15.3443123795369));
#44280=CARTESIAN_POINT('Ctrl Pts',(-39.006177016461,42.323088451335,15.3418555407348));
#44281=CARTESIAN_POINT('Ctrl Pts',(-38.9999710932271,42.110424968906,14.8962126297643));
#44282=CARTESIAN_POINT('Ctrl Pts',(-39.499705301717,42.3015128178088,15.3521413138102));
#44283=CARTESIAN_POINT('Ctrl Pts',(-39.0140356144307,42.3113061213981,15.3474779273468));
#44284=CARTESIAN_POINT('Ctrl Pts',(-38.9999389637436,42.1028779856087,14.9089261998295));
#44285=CARTESIAN_POINT('Ctrl Pts',(-39.4985567623277,42.2685665787124,15.3677673147087));
#44286=CARTESIAN_POINT('Ctrl Pts',(-39.0289560948911,42.2869709989985,15.3590565744642));
#44287=CARTESIAN_POINT('Ctrl Pts',(-38.9998764799132,42.0873689503535,14.9345246110643));
#44288=CARTESIAN_POINT('Ctrl Pts',(-39.4977012327184,42.252035970528,15.3755750143715));
#44289=CARTESIAN_POINT('Ctrl Pts',(-39.036042111538,42.2744076205215,15.365018320954));
#44290=CARTESIAN_POINT('Ctrl Pts',(-38.9998460867584,42.0793955913205,14.9474272309225));
#44291=CARTESIAN_POINT('Ctrl Pts',(-39.4943483441076,42.2025121963684,15.3988684388844));
#44292=CARTESIAN_POINT('Ctrl Pts',(-39.0559248123225,42.2361048981911,15.3831351054061));
#44293=CARTESIAN_POINT('Ctrl Pts',(-38.9997581301239,42.054910884604,14.9862441640743));
#44294=CARTESIAN_POINT('Ctrl Pts',(-39.4910758730554,42.1696645861769,15.4141885363659));
#44295=CARTESIAN_POINT('Ctrl Pts',(-39.0677029508239,42.2092661059301,15.3957550828391));
#44296=CARTESIAN_POINT('Ctrl Pts',(-38.9997039330181,42.0378772531472,15.0122038246002));
#44297=CARTESIAN_POINT('Ctrl Pts',(-39.4827310120233,42.1042521236924,15.4444456124742));
#44298=CARTESIAN_POINT('Ctrl Pts',(-39.0882518024267,42.1539141035433,15.4215864404609));
#44299=CARTESIAN_POINT('Ctrl Pts',(-38.9996049380639,42.0023062299753,15.0642225268363));
#44300=CARTESIAN_POINT('Ctrl Pts',(-39.4776577724669,42.071687442521,15.4593824949676));
#44301=CARTESIAN_POINT('Ctrl Pts',(-39.097119649426,42.1253951687597,15.4348055669586));
#44302=CARTESIAN_POINT('Ctrl Pts',(-38.9995601408351,41.9837687454459,15.0902813011494));
#44303=CARTESIAN_POINT('Ctrl Pts',(-39.4659272469331,42.0067987134986,15.4889006130091));
#44304=CARTESIAN_POINT('Ctrl Pts',(-39.1121948840609,42.0670806077806,15.4616197911504));
#44305=CARTESIAN_POINT('Ctrl Pts',(-38.9994801960717,41.9451171857117,15.1424102581432));
#44306=CARTESIAN_POINT('Ctrl Pts',(-39.4592694379039,41.9744747710641,15.5034817895162));
#44307=CARTESIAN_POINT('Ctrl Pts',(-39.1184774999971,42.0372670016198,15.4752281991058));
#44308=CARTESIAN_POINT('Ctrl Pts',(-38.9994450515753,41.9250030061892,15.1684801936704));
#44309=CARTESIAN_POINT('Ctrl Pts',(-39.4371887494363,41.8778114704634,15.5467261268538));
#44310=CARTESIAN_POINT('Ctrl Pts',(-39.1336266951318,41.947306152076,15.5159502553722));
#44311=CARTESIAN_POINT('Ctrl Pts',(-38.9993541639409,41.862200062219,15.2465495928052));
#44312=CARTESIAN_POINT('Ctrl Pts',(-39.4196659843393,41.8137792589468,15.5748911673596));
#44313=CARTESIAN_POINT('Ctrl Pts',(-39.1394434603886,41.8845388205298,15.5439358601282));
#44314=CARTESIAN_POINT('Ctrl Pts',(-38.9993130685758,41.8170485398245,15.2984073580465));
#44315=CARTESIAN_POINT('Ctrl Pts',(-39.3801865982225,41.6863056631219,15.63003964312));
#44316=CARTESIAN_POINT('Ctrl Pts',(-39.1435098339433,41.7566955261113,15.5999181698673));
#44317=CARTESIAN_POINT('Ctrl Pts',(-38.9992682955504,41.7198634283339,15.4006844242726));
#44318=CARTESIAN_POINT('Ctrl Pts',(-39.3582250294554,41.6228652687111,15.6570225348818));
#44319=CARTESIAN_POINT('Ctrl Pts',(-39.1420289111301,41.6913132981144,15.6280833305903));
#44320=CARTESIAN_POINT('Ctrl Pts',(-38.9992646285384,41.6678269962403,15.4510991499646));
#44321=CARTESIAN_POINT('Ctrl Pts',(-39.3108390135053,41.496383021843,15.7099238273215));
#44322=CARTESIAN_POINT('Ctrl Pts',(-39.1333004854501,41.5591361671536,15.6839796521741));
#44323=CARTESIAN_POINT('Ctrl Pts',(-38.9992908400022,41.5568732567025,15.5491951447912));
#44324=CARTESIAN_POINT('Ctrl Pts',(-39.2855296954198,41.4336465515375,15.7357148560477));
#44325=CARTESIAN_POINT('Ctrl Pts',(-39.1262064141541,41.4922883215965,15.7117610131304));
#44326=CARTESIAN_POINT('Ctrl Pts',(-38.999320637626,41.4982261963719,15.5966316612412));
#44327=CARTESIAN_POINT('Ctrl Pts',(-39.2325813022674,41.3088468026781,15.7861642587015));
#44328=CARTESIAN_POINT('Ctrl Pts',(-39.1079941481342,41.3582935753545,15.7664191396453));
#44329=CARTESIAN_POINT('Ctrl Pts',(-38.9994069311459,41.3750235951481,15.6870996575201));
#44330=CARTESIAN_POINT('Ctrl Pts',(-39.2049393098254,41.2467817121011,15.8108232923254));
#44331=CARTESIAN_POINT('Ctrl Pts',(-39.0968995045062,41.2907260524874,15.7934880316164));
#44332=CARTESIAN_POINT('Ctrl Pts',(-38.9994634273892,41.3104673908405,15.7301267789704));
#44333=CARTESIAN_POINT('Ctrl Pts',(-39.1481308710058,41.1229979262366,15.8591712058507));
#44334=CARTESIAN_POINT('Ctrl Pts',(-39.0721599505498,41.1555075932688,15.846642532199));
#44335=CARTESIAN_POINT('Ctrl Pts',(-38.9995951129554,41.1762194846274,15.8106316224558));
#44336=CARTESIAN_POINT('Ctrl Pts',(-39.1189633371598,41.0612796613498,15.8828598623271));
#44337=CARTESIAN_POINT('Ctrl Pts',(-39.058471586298,41.0874242918864,15.872911516296));
#44338=CARTESIAN_POINT('Ctrl Pts',(-38.9996702917367,41.1065315825528,15.848103351789));
#44339=CARTESIAN_POINT('Ctrl Pts',(-39.0746438817091,40.9687287132405,15.9177688339196));
#44340=CARTESIAN_POINT('Ctrl Pts',(-39.0370060054821,40.9851608213935,15.9116141212873));
#44341=CARTESIAN_POINT('Ctrl Pts',(-38.9997902995097,40.9989813041981,15.8994101871385));
#44342=CARTESIAN_POINT('Ctrl Pts',(-39.0597758040783,40.9378828553123,15.9293009991034));
#44343=CARTESIAN_POINT('Ctrl Pts',(-39.0296982884719,40.9510509478529,15.924399655495));
#44344=CARTESIAN_POINT('Ctrl Pts',(-38.9998315025111,40.9626304897362,15.9156973045773));
#44345=CARTESIAN_POINT('Ctrl Pts',(-39.0374020341813,40.8915916601846,15.9464547300814));
#44346=CARTESIAN_POINT('Ctrl Pts',(-39.018621777892,40.8998382975478,15.9434097092941));
#44347=CARTESIAN_POINT('Ctrl Pts',(-38.9998942165061,40.9074757848707,15.9388322142473));
#44348=CARTESIAN_POINT('Ctrl Pts',(-39.0299321594335,40.8761575280997,15.9521485456168));
#44349=CARTESIAN_POINT('Ctrl Pts',(-39.0149105425542,40.8827594984001,15.9497184465192));
#44350=CARTESIAN_POINT('Ctrl Pts',(-38.9999152726136,40.8889862407112,15.9463280339396));
#44351=CARTESIAN_POINT('Ctrl Pts',(-39.014980252518,40.8452769316474,15.9634898474352));
#44352=CARTESIAN_POINT('Ctrl Pts',(-39.0074696557029,40.8485870786527,15.9622795899339));
#44353=CARTESIAN_POINT('Ctrl Pts',(-38.999957537178,40.8518194900493,15.9608777299468));
#44354=CARTESIAN_POINT('Ctrl Pts',(-39.0075087112135,40.829852316837,15.9691294172817));
#44355=CARTESIAN_POINT('Ctrl Pts',(-39.0037437085461,40.8315106105773,15.9685258477206));
#44356=CARTESIAN_POINT('Ctrl Pts',(-38.999978715904,40.8331689137449,15.9679222747282));
#44357=CARTESIAN_POINT('Ctrl Pts',(-39.,40.8143424311314,15.9747745540155));
#44358=CARTESIAN_POINT('Ctrl Pts',(-39.,40.8143424311314,15.9747745540155));
#44359=CARTESIAN_POINT('Ctrl Pts',(-39.,40.8143424311314,15.9747745540155));
#44360=CARTESIAN_POINT('Origin',(-42.5,34.999999994595,6.55E-10));
#44361=CARTESIAN_POINT('Origin',(-42.5,34.999999994595,6.55E-10));
#44362=CARTESIAN_POINT('Origin',(-42.5,34.999999994595,6.55E-10));
#44363=CARTESIAN_POINT('Ctrl Pts',(-42.,25.0606841227656,1.100000000655));
#44364=CARTESIAN_POINT('Ctrl Pts',(-42.,25.0595088693021,1.09894763890697));
#44365=CARTESIAN_POINT('Ctrl Pts',(-42.0000033223958,25.058333705052,1.09789517038892));
#44366=CARTESIAN_POINT('Ctrl Pts',(-42.0003519017721,24.99671007141,1.04269570981911));
#44367=CARTESIAN_POINT('Ctrl Pts',(-42.0094939504564,24.9360490092969,0.987850887928174));
#44368=CARTESIAN_POINT('Ctrl Pts',(-42.0455618257965,24.8231515921703,0.884898074774389));
#44369=CARTESIAN_POINT('Ctrl Pts',(-42.0716251146577,24.7697076177618,0.835743987830459));
#44370=CARTESIAN_POINT('Ctrl Pts',(-42.1410737799586,24.6746102687835,0.747678118028473));
#44371=CARTESIAN_POINT('Ctrl Pts',(-42.1839363914962,24.6317141928668,0.707651401846346));
#44372=CARTESIAN_POINT('Ctrl Pts',(-42.2753727862072,24.5712359099918,0.650970210180581));
#44373=CARTESIAN_POINT('Ctrl Pts',(-42.3193584730602,24.550090913296,0.631063025893261));
#44374=CARTESIAN_POINT('Ctrl Pts',(-42.4101445564636,24.5237103782914,0.606193989374706));
#44375=CARTESIAN_POINT('Ctrl Pts',(-42.4545481243919,24.5171568688013,0.60000000065501));
#44376=CARTESIAN_POINT('Ctrl Pts',(-42.5,24.5171568688013,0.60000000065501));
#44377=CARTESIAN_POINT('Ctrl Pts',(-42.5,25.2143573355172,3.80673058592581));
#44378=CARTESIAN_POINT('Ctrl Pts',(-42.4546604723592,25.2143573355172,3.80673058592581));
#44379=CARTESIAN_POINT('Ctrl Pts',(-42.410369154297,25.2177192828128,3.79838660971661));
#44380=CARTESIAN_POINT('Ctrl Pts',(-42.3197752645317,25.2312813982443,3.76485163764536));
#44381=CARTESIAN_POINT('Ctrl Pts',(-42.2758690263218,25.2421675242903,3.73798453911452));
#44382=CARTESIAN_POINT('Ctrl Pts',(-42.184505343157,25.2734307410951,3.66132378610309));
#44383=CARTESIAN_POINT('Ctrl Pts',(-42.141641846796,25.2956984958726,3.60706178152292));
#44384=CARTESIAN_POINT('Ctrl Pts',(-42.0719829628829,25.345457581468,3.48710459800191));
#44385=CARTESIAN_POINT('Ctrl Pts',(-42.0457917884805,25.3736439183274,3.41980920565272));
#44386=CARTESIAN_POINT('Ctrl Pts',(-42.0095395323332,25.4335707666125,3.27843423840761));
#44387=CARTESIAN_POINT('Ctrl Pts',(-42.0003527473331,25.4659862397681,3.20286907923119));
#44388=CARTESIAN_POINT('Ctrl Pts',(-42.0000033222927,25.4991296293867,3.126589852694));
#44389=CARTESIAN_POINT('Ctrl Pts',(-42.,25.4997602061239,3.12513893728405));
#44390=CARTESIAN_POINT('Ctrl Pts',(-42.,25.5003909094963,3.12368808212368));
#44391=CARTESIAN_POINT('Origin',(-42.5,31.9421285471778,0.146139381756428));
#44392=CARTESIAN_POINT('Origin',(-42.5,24.5171568688013,1.100000000655));
#44393=CARTESIAN_POINT('Origin',(-42.5,34.999999994595,6.55E-10));
#44394=CARTESIAN_POINT('Ctrl Pts',(-42.,28.5937530433762,-1.099999999345));
#44395=CARTESIAN_POINT('Ctrl Pts',(-42.,28.5946398535677,-1.09894793914394));
#44396=CARTESIAN_POINT('Ctrl Pts',(-42.0000033204919,28.5955267728317,-1.09789596800162));
#44397=CARTESIAN_POINT('Ctrl Pts',(-42.0004662363704,28.6573726864841,-1.02455603473682));
#44398=CARTESIAN_POINT('Ctrl Pts',(-42.0165992209748,28.7192952337358,-0.952209617009781));
#44399=CARTESIAN_POINT('Ctrl Pts',(-42.0758441660175,28.8273260851525,-0.827724174405475));
#44400=CARTESIAN_POINT('Ctrl Pts',(-42.1151456113167,28.8751198610887,-0.773377664441317));
#44401=CARTESIAN_POINT('Ctrl Pts',(-42.2056695167071,28.9469442910977,-0.692456559159142));
#44402=CARTESIAN_POINT('Ctrl Pts',(-42.2516602512676,28.9739516189116,-0.662301437467018));
#44403=CARTESIAN_POINT('Ctrl Pts',(-42.3477951889101,29.0107522579474,-0.621371213393126));
#44404=CARTESIAN_POINT('Ctrl Pts',(-42.3950686181708,29.0223139734333,-0.608583816580183));
#44405=CARTESIAN_POINT('Ctrl Pts',(-42.4631644468274,29.029156829769,-0.601015247603024));
#44406=CARTESIAN_POINT('Ctrl Pts',(-42.4816022135789,29.0300753719553,-0.599999999345001));
#44407=CARTESIAN_POINT('Ctrl Pts',(-42.5,29.0300753719553,-0.599999999345001));
#44408=CARTESIAN_POINT('Origin',(-42.5,24.5171568688013,-1.099999999345));
#44409=CARTESIAN_POINT('Ctrl Pts',(-42.4999999999992,21.3792341097314,-0.599999999345));
#44410=CARTESIAN_POINT('Ctrl Pts',(-42.4490140835651,21.3497688309388,-0.599999999345));
#44411=CARTESIAN_POINT('Ctrl Pts',(-42.4007729318771,21.3161690037742,-0.607751395428307));
#44412=CARTESIAN_POINT('Ctrl Pts',(-42.285433335349,21.2206234281771,-0.642356903987189));
#44413=CARTESIAN_POINT('Ctrl Pts',(-42.2250431349784,21.154461459802,-0.677422925574331));
#44414=CARTESIAN_POINT('Ctrl Pts',(-42.1177385329819,21.0028381404881,-0.76878542539937));
#44415=CARTESIAN_POINT('Ctrl Pts',(-42.0745545865654,20.9152860451152,-0.828340175668635));
#44416=CARTESIAN_POINT('Ctrl Pts',(-42.0155723848691,20.7344912244631,-0.956764117541972));
#44417=CARTESIAN_POINT('Ctrl Pts',(-42.0004519323175,20.6399172853836,-1.02689744515237));
#44418=CARTESIAN_POINT('Ctrl Pts',(-42.0000033273437,20.5446114752944,-1.09789375193343));
#44419=CARTESIAN_POINT('Ctrl Pts',(-42.,20.5431978887484,-1.09894685426265));
#44420=CARTESIAN_POINT('Ctrl Pts',(-42.,20.5417843370527,-1.099999999345));
#44421=CARTESIAN_POINT('Origin',(-35.8316689588642,34.999999994595,6.55E-10));
#44422=CARTESIAN_POINT('Origin',(-43.,34.999999994595,6.55E-10));
#44423=CARTESIAN_POINT('Origin',(-43.,34.999999994595,6.55E-10));
#44424=CARTESIAN_POINT('Origin',(-44.,47.8027400910494,-6.80733765974042));
#44425=CARTESIAN_POINT('Origin',(-42.5,39.7882820011544,13.1556966916577));
#44426=CARTESIAN_POINT('',(-34.,37.4390504491896,14.0107470499719));
#44427=CARTESIAN_POINT('',(-34.,37.4390504491896,14.0107470499719));
#44428=CARTESIAN_POINT('',(-39.,35.0898188972248,14.8657974082861));
#44429=CARTESIAN_POINT('Origin',(-34.,38.5965482096145,9.88143500940095));
#44430=CARTESIAN_POINT('',(-34.,37.7810705925152,14.9504396707578));
#44431=CARTESIAN_POINT('Origin',(-39.,35.4318390405505,15.805490029072));
#44432=CARTESIAN_POINT('Origin',(-30.8535533905933,49.0946168001447,-5.39282731604877));
#44433=CARTESIAN_POINT('Origin',(-46.,34.999999994595,6.54998265276524E-10));
#44434=CARTESIAN_POINT('Origin',(-46.,34.999999994595,6.54998265276524E-10));
#44435=CARTESIAN_POINT('Origin',(-31.,34.999999994595,6.54998265276524E-10));
#44436=CARTESIAN_POINT('',(0.,0.,0.));
#44437=CARTESIAN_POINT('Origin',(32.2,20.9999992399189,6.));
#44438=CARTESIAN_POINT('',(37.3961524227066,20.999999239919,3.));
#44439=CARTESIAN_POINT('Origin',(37.3961524227066,20.999999239919,6.));
#44440=CARTESIAN_POINT('',(37.7511260119006,23.249999239919,6.35));
#44441=CARTESIAN_POINT('',(37.7511260119006,23.249999239919,5.65));
#44442=CARTESIAN_POINT('Origin',(32.2,23.249999239919,6.));
#44443=CARTESIAN_POINT('',(38.1795484779371,21.349999239919,5.65));
#44444=CARTESIAN_POINT('Origin',(32.2,20.9999992399189,5.65));
#44445=CARTESIAN_POINT('',(37.7511260119007,21.349999239919,3.75));
#44446=CARTESIAN_POINT('Origin',(32.2,21.349999239919,6.));
#44447=CARTESIAN_POINT('',(37.7511260119007,20.649999239919,3.75));
#44448=CARTESIAN_POINT('Origin',(32.2,20.9999992399189,3.75));
#44449=CARTESIAN_POINT('',(38.1795484779371,20.649999239919,5.65));
#44450=CARTESIAN_POINT('Origin',(32.2,20.649999239919,6.));
#44451=CARTESIAN_POINT('',(37.7511260119007,18.749999239919,5.65));
#44452=CARTESIAN_POINT('Origin',(32.2,20.9999992399189,5.65));
#44453=CARTESIAN_POINT('',(37.7511260119007,18.749999239919,6.35));
#44454=CARTESIAN_POINT('Origin',(32.2,18.749999239919,5.99999999999999));
#44455=CARTESIAN_POINT('',(38.1795484779371,20.649999239919,6.35));
#44456=CARTESIAN_POINT('Origin',(32.2,20.9999992399189,6.35));
#44457=CARTESIAN_POINT('',(37.7511260119007,20.649999239919,8.25));
#44458=CARTESIAN_POINT('Origin',(32.2,20.649999239919,6.));
#44459=CARTESIAN_POINT('',(37.7511260119007,21.349999239919,8.25));
#44460=CARTESIAN_POINT('Origin',(32.2,20.9999992399189,8.25));
#44461=CARTESIAN_POINT('',(38.1795484779371,21.349999239919,6.35));
#44462=CARTESIAN_POINT('Origin',(32.2,21.349999239919,6.));
#44463=CARTESIAN_POINT('Origin',(32.2,20.9999992399189,6.35));
#44464=CARTESIAN_POINT('Origin',(25.8,20.999999239919,5.99999999999999));
#44465=CARTESIAN_POINT('',(26.1065,20.999999239919,4.49999999999999));
#44466=CARTESIAN_POINT('',(26.1065,20.999999239919,7.49999999999999));
#44467=CARTESIAN_POINT('Origin',(26.1065,20.999999239919,5.99999999999999));
#44468=CARTESIAN_POINT('',(25.8,20.999999239919,7.19349999999999));
#44469=CARTESIAN_POINT('',(25.8,20.999999239919,7.19349999999999));
#44470=CARTESIAN_POINT('Origin',(25.8,20.999999239919,5.99999999999999));
#44471=CARTESIAN_POINT('Origin',(26.1065,20.999999239919,5.99999999999999));
#44472=CARTESIAN_POINT('Origin',(85.8,20.9999992399189,6.00000000000005));
#44473=CARTESIAN_POINT('',(35.8,20.999999239919,3.));
#44474=CARTESIAN_POINT('',(85.8,20.999999239919,3.00000000000005));
#44475=CARTESIAN_POINT('Origin',(35.8,20.999999239919,6.));
#44476=CARTESIAN_POINT('Origin',(85.8,20.9999992399189,6.00000000000005));
#44477=CARTESIAN_POINT('',(35.8,20.999999239919,4.5));
#44478=CARTESIAN_POINT('Origin',(35.8,20.999999239919,6.));
#44479=CARTESIAN_POINT('',(85.8,20.9999992399189,4.50000000000005));
#44480=CARTESIAN_POINT('Origin',(35.8,22.499999239919,6.));
#44481=CARTESIAN_POINT('Origin',(36.4,21.349999239919,8.25));
#44482=CARTESIAN_POINT('',(36.4,21.349999239919,8.25));
#44483=CARTESIAN_POINT('',(36.4,21.349999239919,8.25));
#44484=CARTESIAN_POINT('',(36.4,21.349999239919,6.35));
#44485=CARTESIAN_POINT('',(36.4,21.349999239919,8.25));
#44486=CARTESIAN_POINT('',(36.4,21.349999239919,6.35));
#44487=CARTESIAN_POINT('Origin',(36.4,21.349999239919,6.35));
#44488=CARTESIAN_POINT('',(36.4,23.249999239919,6.35));
#44489=CARTESIAN_POINT('',(36.4,21.349999239919,6.35));
#44490=CARTESIAN_POINT('',(36.4,23.249999239919,6.35));
#44491=CARTESIAN_POINT('Origin',(36.4,23.249999239919,6.35));
#44492=CARTESIAN_POINT('',(36.4,23.249999239919,5.65));
#44493=CARTESIAN_POINT('',(36.4,23.249999239919,6.35));
#44494=CARTESIAN_POINT('',(36.4,23.249999239919,5.65));
#44495=CARTESIAN_POINT('Origin',(36.4,23.249999239919,5.65));
#44496=CARTESIAN_POINT('',(36.4,21.349999239919,5.65));
#44497=CARTESIAN_POINT('',(36.4,23.249999239919,5.65));
#44498=CARTESIAN_POINT('',(36.4,21.349999239919,5.65));
#44499=CARTESIAN_POINT('Origin',(36.4,21.349999239919,5.65));
#44500=CARTESIAN_POINT('',(36.4,21.349999239919,3.75));
#44501=CARTESIAN_POINT('',(36.4,21.349999239919,5.65));
#44502=CARTESIAN_POINT('',(36.4,21.349999239919,3.75));
#44503=CARTESIAN_POINT('Origin',(36.4,21.349999239919,3.75));
#44504=CARTESIAN_POINT('',(36.4,20.649999239919,3.75));
#44505=CARTESIAN_POINT('',(36.4,21.349999239919,3.75));
#44506=CARTESIAN_POINT('',(36.4,20.649999239919,3.75));
#44507=CARTESIAN_POINT('Origin',(36.4,20.649999239919,8.25));
#44508=CARTESIAN_POINT('',(36.4,20.649999239919,8.25));
#44509=CARTESIAN_POINT('',(36.4,20.649999239919,8.25));
#44510=CARTESIAN_POINT('',(36.4,20.649999239919,8.25));
#44511=CARTESIAN_POINT('Origin',(36.4,20.649999239919,6.35));
#44512=CARTESIAN_POINT('',(36.4,20.649999239919,6.35));
#44513=CARTESIAN_POINT('',(36.4,20.649999239919,6.35));
#44514=CARTESIAN_POINT('',(36.4,20.649999239919,6.35));
#44515=CARTESIAN_POINT('Origin',(36.4,20.649999239919,3.75));
#44516=CARTESIAN_POINT('',(36.4,20.649999239919,5.65));
#44517=CARTESIAN_POINT('',(36.4,20.649999239919,3.75));
#44518=CARTESIAN_POINT('',(36.4,20.649999239919,5.65));
#44519=CARTESIAN_POINT('Origin',(36.4,20.649999239919,5.65));
#44520=CARTESIAN_POINT('',(36.4,18.749999239919,5.65));
#44521=CARTESIAN_POINT('',(36.4,20.649999239919,5.65));
#44522=CARTESIAN_POINT('',(36.4,18.749999239919,5.65));
#44523=CARTESIAN_POINT('Origin',(36.4,18.749999239919,6.35));
#44524=CARTESIAN_POINT('',(36.4,18.749999239919,6.35));
#44525=CARTESIAN_POINT('',(36.4,18.749999239919,6.35));
#44526=CARTESIAN_POINT('',(36.4,18.749999239919,6.35));
#44527=CARTESIAN_POINT('Origin',(36.4,18.749999239919,5.65));
#44528=CARTESIAN_POINT('',(36.4,18.749999239919,5.65));
#44529=CARTESIAN_POINT('Origin',(36.4,18.749999239919,6.35));
#44530=CARTESIAN_POINT('Origin',(25.8,20.999999239919,5.99999999999999));
#44531=CARTESIAN_POINT('',(0.,0.,0.));
#44532=CARTESIAN_POINT('Origin',(-12.6095156787167,81.500000021449,118.014000374155));
#44533=CARTESIAN_POINT('',(2.32160098384069,81.500000021449,23.5811578282542));
#44534=CARTESIAN_POINT('',(2.3435029334033,81.500000021449,23.3823606838951));
#44535=CARTESIAN_POINT('',(-8.13657993063557,81.500000021449,118.506794239313));
#44536=CARTESIAN_POINT('',(1.55268733299948,78.977364418784,23.4964448005445));
#44537=CARTESIAN_POINT('Origin',(-2.15133476424044,81.5,23.0883639630957));
#44538=CARTESIAN_POINT('',(1.30589978067932,78.5789363917495,22.9662303004148));
#44539=CARTESIAN_POINT('Ctrl Pts',(1.55268732841254,78.9773644228491,23.4964448000391));
#44540=CARTESIAN_POINT('Ctrl Pts',(1.51761375586145,78.9252402998144,23.4925806618552));
#44541=CARTESIAN_POINT('Ctrl Pts',(1.48036107708696,78.8704476794957,23.4759347437579));
#44542=CARTESIAN_POINT('Ctrl Pts',(1.41282928245068,78.7711847504358,23.4172138237909));
#44543=CARTESIAN_POINT('Ctrl Pts',(1.38261235100385,78.7266711800993,23.3751404616741));
#44544=CARTESIAN_POINT('Ctrl Pts',(1.33718570603301,78.657182012345,23.2807163565727));
#44545=CARTESIAN_POINT('Ctrl Pts',(1.31893775138881,78.6275451314688,23.2221451156177));
#44546=CARTESIAN_POINT('Ctrl Pts',(1.29982863988694,78.5884467386214,23.0961031394044));
#44547=CARTESIAN_POINT('Ctrl Pts',(1.29902406364269,78.5789363962849,23.0286389844206));
#44548=CARTESIAN_POINT('Ctrl Pts',(1.30589977539658,78.5789363962849,22.9662302998328));
#44549=CARTESIAN_POINT('',(1.36065465458583,78.5789363917495,22.4692374395169));
#44550=CARTESIAN_POINT('',(0.867860795006342,78.5789363869598,26.9421731882127));
#44551=CARTESIAN_POINT('',(1.07173072593556,78.2166828749042,21.9343806755756));
#44552=CARTESIAN_POINT('Ctrl Pts',(1.36065464930308,78.5789363962848,22.4692374389349));
#44553=CARTESIAN_POINT('Ctrl Pts',(1.36753036105647,78.5789363962848,22.4068287543516));
#44554=CARTESIAN_POINT('Ctrl Pts',(1.3668087207202,78.5693548526245,22.3393737366166));
#44555=CARTESIAN_POINT('Ctrl Pts',(1.34704682518434,78.5308168815584,22.2132598416578));
#44556=CARTESIAN_POINT('Ctrl Pts',(1.32794969506718,78.5019090265213,22.154595045046));
#44557=CARTESIAN_POINT('Ctrl Pts',(1.2781466042549,78.4361770822946,22.0596887765826));
#44558=CARTESIAN_POINT('Ctrl Pts',(1.24408431979824,78.3949647868373,22.0171917628595));
#44559=CARTESIAN_POINT('Ctrl Pts',(1.16372704304608,78.3067126653714,21.9570578293212));
#44560=CARTESIAN_POINT('Ctrl Pts',(1.1173804610504,78.2597272540181,21.9394100143986));
#44561=CARTESIAN_POINT('Ctrl Pts',(1.07173071992196,78.2166828799263,21.934380674913));
#44562=CARTESIAN_POINT('',(2.48586560556021,81.500000021449,22.0901792455605));
#44563=CARTESIAN_POINT('Origin',(-1.98707014252092,81.5,21.597385380402));
#44564=CARTESIAN_POINT('',(2.81439485066613,81.500000021449,19.1082220597325));
#44565=CARTESIAN_POINT('',(-8.13657993063557,81.500000021449,118.506794239313));
#44566=CARTESIAN_POINT('Origin',(-1.658540897415,81.500000021449,18.615428194574));
#44567=CARTESIAN_POINT('',(2.22867057917708,79.9960688658798,22.061843463808));
#44568=CARTESIAN_POINT('Origin',(-1.98707014252092,81.5,21.597385380402));
#44569=CARTESIAN_POINT('',(2.08630790702017,79.9960688658798,23.3540249021425));
#44570=CARTESIAN_POINT('',(1.681121840112,79.9960688658798,27.031772072787));
#44571=CARTESIAN_POINT('Origin',(-2.12943281467784,81.5,22.8895668187365));
#44572=CARTESIAN_POINT('Origin',(-12.6095156787167,81.500000021449,118.014000374155));
#44573=CARTESIAN_POINT('',(2.08067953865206,81.500000021449,25.767926416205));
#44574=CARTESIAN_POINT('',(2.10258148821465,81.500000021449,25.5691292718459));
#44575=CARTESIAN_POINT('',(-8.13657993063557,81.500000021449,118.506794239313));
#44576=CARTESIAN_POINT('',(1.84538646183153,83.0039311341202,25.5407934900933));
#44577=CARTESIAN_POINT('Origin',(-2.37035425986648,81.5,25.0763354066873));
#44578=CARTESIAN_POINT('',(2.06440595745756,83.0039311341202,23.5528220465017));
#44579=CARTESIAN_POINT('',(1.681121840112,83.0039311341202,27.031772072787));
#44580=CARTESIAN_POINT('Origin',(-2.15133476424044,81.5,23.0883639630957));
#44581=CARTESIAN_POINT('',(-2.12943281467784,86.0000000007247,22.8895668187365));
#44582=CARTESIAN_POINT('Origin',(-2.12943281467784,81.5,22.8895668187365));
#44583=CARTESIAN_POINT('',(-2.39225620942908,86.0000000007247,25.2751325510465));
#44584=CARTESIAN_POINT('',(-2.12943281467784,86.,22.8895668187365));
#44585=CARTESIAN_POINT('Origin',(-2.39225620942908,81.5,25.2751325510465));
#44586=CARTESIAN_POINT('Origin',(-12.6095156787167,81.500000021449,118.014000374155));
#44587=CARTESIAN_POINT('',(-7.31525682145931,81.500000021449,111.051901325908));
#44588=CARTESIAN_POINT('',(-7.2933548718967,81.500000021449,110.853104181549));
#44589=CARTESIAN_POINT('',(-8.13657993063557,81.500000021449,118.506794239313));
#44590=CARTESIAN_POINT('',(-8.0841704721213,78.9773644192325,110.967188298218));
#44591=CARTESIAN_POINT('Origin',(-11.7881925695404,81.5,110.55910746075));
#44592=CARTESIAN_POINT('',(-8.33095802467381,78.5789363917952,110.436973798063));
#44593=CARTESIAN_POINT('Ctrl Pts',(-8.0841704768878,78.9773644228493,110.967188297693));
#44594=CARTESIAN_POINT('Ctrl Pts',(-8.11924404944169,78.9252402998083,110.963324159568));
#44595=CARTESIAN_POINT('Ctrl Pts',(-8.15649672821697,78.8704476794907,110.94667824141));
#44596=CARTESIAN_POINT('Ctrl Pts',(-8.22402852285583,78.7711847504269,110.887957321438));
#44597=CARTESIAN_POINT('Ctrl Pts',(-8.25424545430345,78.7266711800892,110.845883959318));
#44598=CARTESIAN_POINT('Ctrl Pts',(-8.29967209927197,78.6571820123377,110.751459854213));
#44599=CARTESIAN_POINT('Ctrl Pts',(-8.31792005391415,78.6275451314643,110.69288861326));
#44600=CARTESIAN_POINT('Ctrl Pts',(-8.33702916541348,78.5884467386206,110.566846637052));
#44601=CARTESIAN_POINT('Ctrl Pts',(-8.33783374165725,78.5789363962851,110.499382482071));
#44602=CARTESIAN_POINT('Ctrl Pts',(-8.33095802990372,78.5789363962851,110.436973797487));
#44603=CARTESIAN_POINT('',(-8.27620315076731,78.5789363917951,109.939980937165));
#44604=CARTESIAN_POINT('',(-8.76899701029366,78.5789363869598,114.412916685867));
#44605=CARTESIAN_POINT('',(-8.56512707942982,78.2166828749152,109.405124173222));
#44606=CARTESIAN_POINT('Ctrl Pts',(-8.27620315599722,78.5789363962851,109.939980936589));
#44607=CARTESIAN_POINT('Ctrl Pts',(-8.26932744424383,78.5789363962851,109.877572252006));
#44608=CARTESIAN_POINT('Ctrl Pts',(-8.2700490845801,78.5693548526248,109.810117234271));
#44609=CARTESIAN_POINT('Ctrl Pts',(-8.28981098011595,78.5308168815586,109.684003339312));
#44610=CARTESIAN_POINT('Ctrl Pts',(-8.30890811023311,78.5019090265215,109.6253385427));
#44611=CARTESIAN_POINT('Ctrl Pts',(-8.35871120104538,78.4361770822949,109.530432274237));
#44612=CARTESIAN_POINT('Ctrl Pts',(-8.39277348550203,78.3949647868375,109.487935260513));
#44613=CARTESIAN_POINT('Ctrl Pts',(-8.47313076225417,78.3067126653716,109.427801326975));
#44614=CARTESIAN_POINT('Ctrl Pts',(-8.51947734424986,78.2597272540184,109.410153512053));
#44615=CARTESIAN_POINT('Ctrl Pts',(-8.56512708537829,78.2166828799266,109.405124172567));
#44616=CARTESIAN_POINT('',(-7.15099219973979,81.500000021449,109.560922743215));
#44617=CARTESIAN_POINT('Origin',(-11.6239279478209,81.5,109.068128878056));
#44618=CARTESIAN_POINT('',(1.93831686649513,81.500000021449,27.0601078545396));
#44619=CARTESIAN_POINT('',(-8.13657993063557,81.500000021449,118.506794239313));
#44620=CARTESIAN_POINT('',(0.524181986870476,78.2166828749042,26.9043092845546));
#44621=CARTESIAN_POINT('Origin',(-2.534618881586,81.5,26.567313989381));
#44622=CARTESIAN_POINT('',(0.922615663333761,78.5789363917495,26.4451803267001));
#44623=CARTESIAN_POINT('Ctrl Pts',(0.524181980856895,78.2166828799263,26.9043092838921));
#44624=CARTESIAN_POINT('Ctrl Pts',(0.569831721989357,78.2597272540282,26.9093386232555));
#44625=CARTESIAN_POINT('Ctrl Pts',(0.618908660925751,78.3067126653714,26.9022038424795));
#44626=CARTESIAN_POINT('Ctrl Pts',(0.71042987961836,78.3949647868373,26.8610061675593));
#44627=CARTESIAN_POINT('Ctrl Pts',(0.752926883593083,78.4361770822946,26.8269438709403));
#44628=CARTESIAN_POINT('Ctrl Pts',(0.822196767061209,78.5019090265213,26.7451561524711));
#44629=CARTESIAN_POINT('Ctrl Pts',(0.853607315213045,78.5308168815584,26.69205590572));
#44630=CARTESIAN_POINT('Ctrl Pts',(0.900350505106304,78.5693548526245,26.5732690326429));
#44631=CARTESIAN_POINT('Ctrl Pts',(0.915739946297612,78.5789363962848,26.5075890107014));
#44632=CARTESIAN_POINT('Ctrl Pts',(0.922615658051007,78.5789363962848,26.4451803261182));
#44633=CARTESIAN_POINT('',(0.977370537240269,78.5789363917495,25.9481874658022));
#44634=CARTESIAN_POINT('',(0.867860795006342,78.5789363869598,26.9421731882127));
#44635=CARTESIAN_POINT('',(1.33366783737344,78.977364418784,25.4844162441361));
#44636=CARTESIAN_POINT('Ctrl Pts',(0.977370531957515,78.5789363962848,25.9481874652202));
#44637=CARTESIAN_POINT('Ctrl Pts',(0.984246243711048,78.5789363962848,25.8857787806357));
#44638=CARTESIAN_POINT('Ctrl Pts',(0.999718620810108,78.5884467386204,25.8201078959373));
#44639=CARTESIAN_POINT('Ctrl Pts',(1.04580902666772,78.627545131464,25.7012491041017));
#44640=CARTESIAN_POINT('Ctrl Pts',(1.07637039934524,78.6571820123375,25.6480553016858));
#44641=CARTESIAN_POINT('Ctrl Pts',(1.14126383696667,78.726671180089,25.5657854198846));
#44642=CARTESIAN_POINT('Ctrl Pts',(1.17991548793108,78.7711847504267,25.5312994716744));
#44643=CARTESIAN_POINT('Ctrl Pts',(1.25861122451092,78.8704476794904,25.4886887831835));
#44644=CARTESIAN_POINT('Ctrl Pts',(1.29859426023195,78.9252402998056,25.4805521055439));
#44645=CARTESIAN_POINT('Ctrl Pts',(1.33366783278649,78.977364422849,25.4844162436308));
#44646=CARTESIAN_POINT('Origin',(-2.37035425986648,81.5,25.0763354066873));
#44647=CARTESIAN_POINT('',(1.82348451226893,79.9960688658798,25.7395906344525));
#44648=CARTESIAN_POINT('Origin',(-2.39225620942908,81.5,25.2751325510465));
#44649=CARTESIAN_POINT('',(1.681121840112,79.9960688658798,27.031772072787));
#44650=CARTESIAN_POINT('',(1.681121840112,79.9960688658798,27.031772072787));
#44651=CARTESIAN_POINT('Origin',(-2.534618881586,81.5,26.567313989381));
#44652=CARTESIAN_POINT('',(-7.40818722558546,79.9960688674047,109.532586961521));
#44653=CARTESIAN_POINT('Origin',(-11.6239279478209,81.5,109.068128878056));
#44654=CARTESIAN_POINT('',(-7.55054989827983,79.9960688658798,110.824768399797));
#44655=CARTESIAN_POINT('',(-7.955735965188,79.9960688658798,114.502515570441));
#44656=CARTESIAN_POINT('Origin',(-11.7662906199778,81.5,110.360310316391));
#44657=CARTESIAN_POINT('Origin',(-12.6095156787167,81.500000021449,118.014000374155));
#44658=CARTESIAN_POINT('',(-8.13657993063557,81.500000021449,118.506794239313));
#44659=CARTESIAN_POINT('Origin',(-12.6095156787167,81.500000021449,118.014000374155));
#44660=CARTESIAN_POINT('',(-7.69854093880487,81.500000021449,114.530851352194));
#44661=CARTESIAN_POINT('',(-8.13657993063557,81.500000021449,118.506794239313));
#44662=CARTESIAN_POINT('',(-9.11267581892563,78.2166828745796,114.375052782154));
#44663=CARTESIAN_POINT('Origin',(-12.171476686886,81.5,114.038057487035));
#44664=CARTESIAN_POINT('',(-8.71424214201937,78.5789363917952,113.915923824348));
#44665=CARTESIAN_POINT('Ctrl Pts',(-9.11267582444339,78.2166828799266,114.375052781546));
#44666=CARTESIAN_POINT('Ctrl Pts',(-9.06702608331569,78.2597272540202,114.380082120982));
#44667=CARTESIAN_POINT('Ctrl Pts',(-9.01794914437927,78.3067126653671,114.372947340134));
#44668=CARTESIAN_POINT('Ctrl Pts',(-8.92642792569046,78.3949647868293,114.331749665219));
#44669=CARTESIAN_POINT('Ctrl Pts',(-8.88393092171716,78.4361770822852,114.297687368603));
#44670=CARTESIAN_POINT('Ctrl Pts',(-8.81466103824691,78.5019090265143,114.215899650137));
#44671=CARTESIAN_POINT('Ctrl Pts',(-8.78325049009251,78.530816881554,114.162799403385));
#44672=CARTESIAN_POINT('Ctrl Pts',(-8.73650730019552,78.5693548526238,114.044012530303));
#44673=CARTESIAN_POINT('Ctrl Pts',(-8.72111785900304,78.5789363962851,113.978332508359));
#44674=CARTESIAN_POINT('Ctrl Pts',(-8.71424214724929,78.5789363962851,113.915923823772));
#44675=CARTESIAN_POINT('',(-8.65948726811286,78.5789363917952,113.41893096345));
#44676=CARTESIAN_POINT('',(-8.76899701029366,78.5789363869598,114.412916685867));
#44677=CARTESIAN_POINT('',(-8.30318996795119,78.9773644188579,112.955159741787));
#44678=CARTESIAN_POINT('Ctrl Pts',(-8.65948727334278,78.5789363962851,113.418930962874));
#44679=CARTESIAN_POINT('Ctrl Pts',(-8.65261156158889,78.5789363962851,113.356522278286));
#44680=CARTESIAN_POINT('Ctrl Pts',(-8.63713918448864,78.5884467386216,113.290851393585));
#44681=CARTESIAN_POINT('Ctrl Pts',(-8.59104877862742,78.627545131469,113.171992601745));
#44682=CARTESIAN_POINT('Ctrl Pts',(-8.5604874059475,78.6571820123452,113.118798799327));
#44683=CARTESIAN_POINT('Ctrl Pts',(-8.49559396832452,78.7266711800996,113.03652891753));
#44684=CARTESIAN_POINT('Ctrl Pts',(-8.45694231736169,78.771184750436,113.002042969323));
#44685=CARTESIAN_POINT('Ctrl Pts',(-8.37824658078551,78.870447679496,112.959432280837));
#44686=CARTESIAN_POINT('Ctrl Pts',(-8.33826354506655,78.9252402998085,112.951295603198));
#44687=CARTESIAN_POINT('Ctrl Pts',(-8.30318997251383,78.9773644228493,112.955159741285));
#44688=CARTESIAN_POINT('',(-7.53427631708535,81.500000021449,113.0398727695));
#44689=CARTESIAN_POINT('Origin',(-12.0072120651665,81.5,112.547078904341));
#44690=CARTESIAN_POINT('',(-7.55617826664794,81.500000021449,113.238669913859));
#44691=CARTESIAN_POINT('',(-8.13657993063557,81.500000021449,118.506794239313));
#44692=CARTESIAN_POINT('',(-7.81337329303107,79.9960688658798,113.210334132106));
#44693=CARTESIAN_POINT('Origin',(-12.0291140147291,81.5,112.7458760487));
#44694=CARTESIAN_POINT('',(-7.95573596518799,79.9960688658798,114.502515570441));
#44695=CARTESIAN_POINT('',(-7.955735965188,79.9960688658798,114.502515570441));
#44696=CARTESIAN_POINT('Origin',(-12.171476686886,81.5,114.038057487035));
#44697=CARTESIAN_POINT('Origin',(-2.534618881586,81.5,26.567313989381));
#44698=CARTESIAN_POINT('',(-7.45399161239785,81.5,20.9950817674304));
#44699=CARTESIAN_POINT('',(-8.00154035146294,81.5,25.9650103764094));
#44700=CARTESIAN_POINT('',(-8.00154035146294,81.5,25.9650103764094));
#44701=CARTESIAN_POINT('',(1.83168562221586,77.5642538212272,22.0181066961974));
#44702=CARTESIAN_POINT('Origin',(-1.98707014252092,81.5,21.597385380402));
#44703=CARTESIAN_POINT('',(2.11676125496322,77.9298111396176,22.5525394843164));
#44704=CARTESIAN_POINT('Ctrl Pts',(1.83168562221586,77.5642538212272,22.0181066961974));
#44705=CARTESIAN_POINT('Ctrl Pts',(1.87641861446953,77.6081839481971,22.0230350353005));
#44706=CARTESIAN_POINT('Ctrl Pts',(1.9219453311641,77.6558998044383,22.0406193987957));
#44707=CARTESIAN_POINT('Ctrl Pts',(2.00111428556866,77.7451420947154,22.1006406181192));
#44708=CARTESIAN_POINT('Ctrl Pts',(2.03479950715842,77.786624874732,22.1430856683949));
#44709=CARTESIAN_POINT('Ctrl Pts',(2.08418676443722,77.8526750346387,22.2379141585008));
#44710=CARTESIAN_POINT('Ctrl Pts',(2.10320619628386,77.8816487301738,22.2965714738577));
#44711=CARTESIAN_POINT('Ctrl Pts',(2.12290794061138,77.9202366687201,22.4226781994981));
#44712=CARTESIAN_POINT('Ctrl Pts',(2.12363677900081,77.9298111396176,22.4901325035708));
#44713=CARTESIAN_POINT('Ctrl Pts',(2.11676125496322,77.9298111396176,22.5525394843164));
#44714=CARTESIAN_POINT('',(2.06200638105671,77.9298111396176,23.0495323452143));
#44715=CARTESIAN_POINT('',(2.17151612886973,77.9298111396176,22.0555466234185));
#44716=CARTESIAN_POINT('',(2.31264222801171,78.3249353664633,23.5801708210266));
#44717=CARTESIAN_POINT('Ctrl Pts',(2.06200638105672,77.9298111396176,23.0495323452143));
#44718=CARTESIAN_POINT('Ctrl Pts',(2.05513085701913,77.9298111396176,23.11193932596));
#44719=CARTESIAN_POINT('Ctrl Pts',(2.05592754820022,77.9393273581992,23.1794011055345));
#44720=CARTESIAN_POINT('Ctrl Pts',(2.07509523675738,77.9783737890882,23.305448992993));
#44721=CARTESIAN_POINT('Ctrl Pts',(2.09341990517389,78.0079439461362,23.3640297646265));
#44722=CARTESIAN_POINT('Ctrl Pts',(2.13922834115554,78.0770665607413,23.4584639675621));
#44723=CARTESIAN_POINT('Ctrl Pts',(2.16977139876493,78.1212469206825,23.5005628382322));
#44724=CARTESIAN_POINT('Ctrl Pts',(2.23845975544489,78.2194869113329,23.5594293854225));
#44725=CARTESIAN_POINT('Ctrl Pts',(2.27655500713784,78.2735827563092,23.5761950069173));
#44726=CARTESIAN_POINT('Ctrl Pts',(2.31264222801172,78.3249353664633,23.5801708210266));
#44727=CARTESIAN_POINT('',(3.00123722894601,83.3381380528135,23.6560349539252));
#44728=CARTESIAN_POINT('Origin',(-2.15133476424044,81.5,23.0883639630957));
#44729=CARTESIAN_POINT('',(2.78221773331998,83.3381380528135,25.6440063975169));
#44730=CARTESIAN_POINT('',(3.16550185066553,83.3381380528135,22.1650563712315));
#44731=CARTESIAN_POINT('',(2.09362273238568,78.3249353664633,25.5681422646183));
#44732=CARTESIAN_POINT('Origin',(-2.37035425986648,81.5,25.0763354066873));
#44733=CARTESIAN_POINT('',(1.73347713761766,77.9298111396176,26.0314895106017));
#44734=CARTESIAN_POINT('Ctrl Pts',(2.09362273238568,78.3249353664633,25.5681422646183));
#44735=CARTESIAN_POINT('Ctrl Pts',(2.0575355115118,78.2735827563092,25.5641664505089));
#44736=CARTESIAN_POINT('Ctrl Pts',(2.01670405211226,78.2194869113329,25.5722365303698));
#44737=CARTESIAN_POINT('Ctrl Pts',(1.9368477899923,78.1212469206825,25.6147375670833));
#44738=CARTESIAN_POINT('Ctrl Pts',(1.8978722816583,78.0770665607413,25.6491774136268));
#44739=CARTESIAN_POINT('Ctrl Pts',(1.83260401187277,78.0079439461362,25.7313740343017));
#44740=CARTESIAN_POINT('Ctrl Pts',(1.80196569053251,77.9783737890882,25.7845604380456));
#44741=CARTESIAN_POINT('Ctrl Pts',(1.75581682568182,77.9393273581992,25.9034122469942));
#44742=CARTESIAN_POINT('Ctrl Pts',(1.74035266165525,77.9298111396176,25.9690825298561));
#44743=CARTESIAN_POINT('Ctrl Pts',(1.73347713761766,77.9298111396176,26.0314895106017));
#44744=CARTESIAN_POINT('',(1.67872226371115,77.9298111396176,26.5284823714996));
#44745=CARTESIAN_POINT('',(1.62396738980464,77.9298111396176,27.0254752323975));
#44746=CARTESIAN_POINT('',(1.28413688315078,77.5642538212272,26.9880353051765));
#44747=CARTESIAN_POINT('Ctrl Pts',(1.67872226371115,77.9298111396176,26.5284823714996));
#44748=CARTESIAN_POINT('Ctrl Pts',(1.67184673967356,77.9298111396176,26.5908893522453));
#44749=CARTESIAN_POINT('Ctrl Pts',(1.65645042843866,77.9202366687201,26.656567110609));
#44750=CARTESIAN_POINT('Ctrl Pts',(1.6097675078176,77.8816487301738,26.7753600813757));
#44751=CARTESIAN_POINT('Ctrl Pts',(1.57843442304722,77.8526750346387,26.8284699413964));
#44752=CARTESIAN_POINT('Ctrl Pts',(1.50958733196454,77.786624874732,26.9102722749007));
#44753=CARTESIAN_POINT('Ctrl Pts',(1.46746965965018,77.7451420947154,26.9443659418387));
#44754=CARTESIAN_POINT('Ctrl Pts',(1.37713279980561,77.6558998044384,26.9857123064191));
#44755=CARTESIAN_POINT('Ctrl Pts',(1.32886987540445,77.6081839481971,26.9929636442795));
#44756=CARTESIAN_POINT('Ctrl Pts',(1.28413688315077,77.5642538212272,26.9880353051765));
#44757=CARTESIAN_POINT('Origin',(-2.534618881586,81.5,26.567313989381));
#44758=CARTESIAN_POINT('Origin',(-12.171476686886,81.5,114.038057487035));
#44759=CARTESIAN_POINT('',(-17.0908494176979,81.5,108.465825265084));
#44760=CARTESIAN_POINT('',(-17.6383981567629,81.5,113.435753874063));
#44761=CARTESIAN_POINT('',(-17.6383981567629,81.5,113.435753874063));
#44762=CARTESIAN_POINT('',(-7.80517218308414,77.5642538212272,109.488850193851));
#44763=CARTESIAN_POINT('Origin',(-11.6239279478209,81.5,109.068128878056));
#44764=CARTESIAN_POINT('',(-7.52009655033678,77.9298111396176,110.02328298197));
#44765=CARTESIAN_POINT('Ctrl Pts',(-7.80517218308414,77.5642538212272,109.488850193851));
#44766=CARTESIAN_POINT('Ctrl Pts',(-7.76043919083047,77.6081839481971,109.493778532954));
#44767=CARTESIAN_POINT('Ctrl Pts',(-7.7149124741359,77.6558998044383,109.51136289645));
#44768=CARTESIAN_POINT('Ctrl Pts',(-7.63574351973134,77.7451420947154,109.571384115773));
#44769=CARTESIAN_POINT('Ctrl Pts',(-7.60205829814157,77.786624874732,109.613829166049));
#44770=CARTESIAN_POINT('Ctrl Pts',(-7.55267104086277,77.8526750346387,109.708657656155));
#44771=CARTESIAN_POINT('Ctrl Pts',(-7.53365160901614,77.8816487301738,109.767314971512));
#44772=CARTESIAN_POINT('Ctrl Pts',(-7.51394986468862,77.9202366687201,109.893421697152));
#44773=CARTESIAN_POINT('Ctrl Pts',(-7.5132210262992,77.9298111396176,109.960876001225));
#44774=CARTESIAN_POINT('Ctrl Pts',(-7.52009655033678,77.9298111396176,110.02328298197));
#44775=CARTESIAN_POINT('',(-7.57485142424329,77.9298111396176,110.520275842868));
#44776=CARTESIAN_POINT('',(-7.46534167643027,77.9298111396176,109.526290121073));
#44777=CARTESIAN_POINT('',(-7.32421557728829,78.3249353664633,111.050914318681));
#44778=CARTESIAN_POINT('Ctrl Pts',(-7.57485142424328,77.9298111396176,110.520275842868));
#44779=CARTESIAN_POINT('Ctrl Pts',(-7.58172694828087,77.9298111396176,110.582682823614));
#44780=CARTESIAN_POINT('Ctrl Pts',(-7.58093025709977,77.9393273581992,110.650144603188));
#44781=CARTESIAN_POINT('Ctrl Pts',(-7.56176256854262,77.9783737890883,110.776192490647));
#44782=CARTESIAN_POINT('Ctrl Pts',(-7.54343790012612,78.0079439461362,110.834773262281));
#44783=CARTESIAN_POINT('Ctrl Pts',(-7.49762946414447,78.0770665607413,110.929207465216));
#44784=CARTESIAN_POINT('Ctrl Pts',(-7.46708640653507,78.1212469206825,110.971306335886));
#44785=CARTESIAN_POINT('Ctrl Pts',(-7.39839804985511,78.2194869113329,111.030172883077));
#44786=CARTESIAN_POINT('Ctrl Pts',(-7.36030279816216,78.2735827563092,111.046938504571));
#44787=CARTESIAN_POINT('Ctrl Pts',(-7.32421557728828,78.3249353664633,111.050914318681));
#44788=CARTESIAN_POINT('',(-6.63562057635399,83.3381380528135,111.126778451579));
#44789=CARTESIAN_POINT('Origin',(-11.7881925695404,81.5,110.55910746075));
#44790=CARTESIAN_POINT('',(-6.85464007198003,83.3381380528135,113.114749895171));
#44791=CARTESIAN_POINT('',(-6.47135595463447,83.3381380528135,109.635799868886));
#44792=CARTESIAN_POINT('',(-7.54323507291432,78.3249353664633,113.038885762272));
#44793=CARTESIAN_POINT('Origin',(-12.0072120651665,81.5,112.547078904341));
#44794=CARTESIAN_POINT('',(-7.90338066768234,77.9298111396176,113.502233008256));
#44795=CARTESIAN_POINT('Ctrl Pts',(-7.54323507291431,78.3249353664633,113.038885762272));
#44796=CARTESIAN_POINT('Ctrl Pts',(-7.57932229378819,78.2735827563092,113.034909948163));
#44797=CARTESIAN_POINT('Ctrl Pts',(-7.62015375318775,78.2194869113329,113.042980028024));
#44798=CARTESIAN_POINT('Ctrl Pts',(-7.7000100153077,78.1212469206825,113.085481064737));
#44799=CARTESIAN_POINT('Ctrl Pts',(-7.7389855236417,78.0770665607413,113.119920911281));
#44800=CARTESIAN_POINT('Ctrl Pts',(-7.80425379342723,78.0079439461362,113.202117531956));
#44801=CARTESIAN_POINT('Ctrl Pts',(-7.83489211476748,77.9783737890882,113.2553039357));
#44802=CARTESIAN_POINT('Ctrl Pts',(-7.88104097961818,77.9393273581992,113.374155744648));
#44803=CARTESIAN_POINT('Ctrl Pts',(-7.89650514364476,77.9298111396176,113.43982602751));
#44804=CARTESIAN_POINT('Ctrl Pts',(-7.90338066768234,77.9298111396176,113.502233008256));
#44805=CARTESIAN_POINT('',(-7.95813554158885,77.9298111396176,113.999225869154));
#44806=CARTESIAN_POINT('',(-8.01289041549536,77.9298111396176,114.496218730052));
#44807=CARTESIAN_POINT('',(-8.35272092214922,77.5642538212272,114.45877880283));
#44808=CARTESIAN_POINT('Ctrl Pts',(-7.95813554158885,77.9298111396176,113.999225869154));
#44809=CARTESIAN_POINT('Ctrl Pts',(-7.96501106562644,77.9298111396176,114.061632849899));
#44810=CARTESIAN_POINT('Ctrl Pts',(-7.98040737686134,77.9202366687201,114.127310608263));
#44811=CARTESIAN_POINT('Ctrl Pts',(-8.0270902974824,77.8816487301738,114.24610357903));
#44812=CARTESIAN_POINT('Ctrl Pts',(-8.0584233822528,77.8526750346387,114.29921343905));
#44813=CARTESIAN_POINT('Ctrl Pts',(-8.12727047333548,77.786624874732,114.381015772555));
#44814=CARTESIAN_POINT('Ctrl Pts',(-8.16938814564984,77.7451420947154,114.415109439493));
#44815=CARTESIAN_POINT('Ctrl Pts',(-8.25972500549441,77.6558998044383,114.456455804073));
#44816=CARTESIAN_POINT('Ctrl Pts',(-8.30798792989556,77.6081839481971,114.463707141934));
#44817=CARTESIAN_POINT('Ctrl Pts',(-8.35272092214923,77.5642538212272,114.45877880283));
#44818=CARTESIAN_POINT('Origin',(-12.171476686886,81.5,114.038057487035));
#44819=CARTESIAN_POINT('Origin',(-14.7997106497322,77.000000018974,137.893714808445));
#44820=CARTESIAN_POINT('',(-17.0067015889499,77.000000018974,139.662666756411));
#44821=CARTESIAN_POINT('Origin',(-15.0187301453583,77.000000018974,139.881686252037));
#44822=CARTESIAN_POINT('',(-16.7876820933239,77.000000018974,137.674695312819));
#44823=CARTESIAN_POINT('',(-16.7876820933239,77.000000018974,137.674695312819));
#44824=CARTESIAN_POINT('Origin',(-14.7997106497322,77.000000018974,137.893714808445));
#44825=CARTESIAN_POINT('Origin',(-11.2953987197157,81.500000018974,106.086171710979));
#44826=CARTESIAN_POINT('',(-13.7803630242052,81.500000018974,105.812397341447));
#44827=CARTESIAN_POINT('Origin',(-11.2953987197157,81.500000018974,106.086171710979));
#44828=CARTESIAN_POINT('',(-15.0944799979614,81.500000018974,117.740226002996));
#44829=CARTESIAN_POINT('',(-13.7803630242052,81.500000018974,105.812397341447));
#44830=CARTESIAN_POINT('Origin',(-12.6095156934719,81.500000018974,118.014000372529));
#44831=CARTESIAN_POINT('Origin',(-12.5547608195654,81.500000018974,117.517007511631));
#44832=CARTESIAN_POINT('',(-9.55592370657306,81.500000018974,106.277813769652));
#44833=CARTESIAN_POINT('Origin',(-11.2953987197157,81.500000018974,106.086171710979));
#44834=CARTESIAN_POINT('',(-10.8152858064227,81.500000018974,117.708649570304));
#44835=CARTESIAN_POINT('',(-10.8152858064227,81.500000018974,117.708649570304));
#44836=CARTESIAN_POINT('Origin',(-12.5547608195654,81.500000018974,117.517007511631));
#44837=CARTESIAN_POINT('Origin',(-7.01890469369955,83.3381380528135,114.605728477865));
#44838=CARTESIAN_POINT('',(-7.13261343725189,84.204163456598,111.072023577673));
#44839=CARTESIAN_POINT('',(-7.57245184784244,83.0039311341202,111.023565544156));
#44840=CARTESIAN_POINT('Origin',(-6.63562057635399,83.3381380528135,111.126778451579));
#44841=CARTESIAN_POINT('',(-7.79147134346847,83.0039311341202,113.011536987747));
#44842=CARTESIAN_POINT('',(-7.955735965188,83.0039311341202,114.502515570441));
#44843=CARTESIAN_POINT('',(-7.35163293287793,84.204163456598,113.059995021264));
#44844=CARTESIAN_POINT('Origin',(-6.85464007198003,83.3381380528135,113.114749895171));
#44845=CARTESIAN_POINT('',(-7.51589755459745,84.204163456598,114.550973603958));
#44846=CARTESIAN_POINT('Origin',(-7.01890469369955,79.6618619471865,114.605728477865));
#44847=CARTESIAN_POINT('',(-7.37353488244054,78.795836543402,113.258792165624));
#44848=CARTESIAN_POINT('Origin',(-6.87654202154263,79.6618619471865,113.31354703953));
#44849=CARTESIAN_POINT('',(-7.51589755459745,78.795836543402,114.550973603958));
#44850=CARTESIAN_POINT('',(-7.51589755459745,78.795836543402,114.550973603958));
#44851=CARTESIAN_POINT('Origin',(-7.01890469369955,79.6618619471865,114.605728477865));
#44852=CARTESIAN_POINT('Origin',(-7.01890469369955,79.6618619471865,114.605728477865));
#44853=CARTESIAN_POINT('',(-6.96834881553237,78.795836543402,109.581044994979));
#44854=CARTESIAN_POINT('Origin',(-6.47135595463447,79.6618619471865,109.635799868886));
#44855=CARTESIAN_POINT('',(-7.1107114876893,78.795836543402,110.873226433314));
#44856=CARTESIAN_POINT('',(-7.51589755459745,78.795836543402,114.550973603958));
#44857=CARTESIAN_POINT('Origin',(-6.61371862679139,79.6618619471865,110.92798130722));
#44858=CARTESIAN_POINT('Origin',(-12.171476686886,81.5,114.038057487035));
#44859=CARTESIAN_POINT('',(-7.01890469369955,79.6618619471865,114.605728477865));
#44860=CARTESIAN_POINT('Origin',(-12.171476686886,81.5,114.038057487035));
#44861=CARTESIAN_POINT('',(-6.87654202154265,79.6618619471864,113.31354703953));
#44862=CARTESIAN_POINT('',(-6.47135595463447,79.6618619471865,109.635799868886));
#44863=CARTESIAN_POINT('',(-12.0291140147291,87.,112.7458760487));
#44864=CARTESIAN_POINT('Origin',(-12.0291140147291,81.5,112.7458760487));
#44865=CARTESIAN_POINT('',(-11.7662906199778,87.,110.360310316391));
#44866=CARTESIAN_POINT('',(-12.0291140147291,87.,112.7458760487));
#44867=CARTESIAN_POINT('',(-6.61371862679139,79.6618619471865,110.92798130722));
#44868=CARTESIAN_POINT('Origin',(-11.7662906199778,81.5,110.360310316391));
#44869=CARTESIAN_POINT('',(-6.47135595463447,79.6618619471865,109.635799868886));
#44870=CARTESIAN_POINT('',(-6.47135595463447,79.6618619471865,109.635799868886));
#44871=CARTESIAN_POINT('Origin',(-11.6239279478209,81.5,109.068128878056));
#44872=CARTESIAN_POINT('Origin',(2.61795311160045,79.6618619471865,27.1349849802106));
#44873=CARTESIAN_POINT('',(2.26332292285946,78.795836543402,25.7880486679695));
#44874=CARTESIAN_POINT('Origin',(2.76031578375737,79.6618619471865,25.842803541876));
#44875=CARTESIAN_POINT('',(2.12096025070255,78.795836543402,27.0802301063041));
#44876=CARTESIAN_POINT('',(2.12096025070255,78.795836543402,27.0802301063041));
#44877=CARTESIAN_POINT('Origin',(2.61795311160045,79.6618619471865,27.1349849802106));
#44878=CARTESIAN_POINT('Origin',(2.61795311160045,79.6618619471865,27.1349849802106));
#44879=CARTESIAN_POINT('',(2.66850898976763,78.795836543402,22.110301497325));
#44880=CARTESIAN_POINT('Origin',(3.16550185066553,79.6618619471865,22.1650563712315));
#44881=CARTESIAN_POINT('',(2.5261463176107,78.795836543402,23.4024829356596));
#44882=CARTESIAN_POINT('',(2.12096025070255,78.795836543402,27.0802301063041));
#44883=CARTESIAN_POINT('Origin',(3.02313917850861,79.6618619471865,23.4572378095661));
#44884=CARTESIAN_POINT('Origin',(-2.534618881586,81.5,26.567313989381));
#44885=CARTESIAN_POINT('',(2.61795311160045,79.6618619471865,27.1349849802106));
#44886=CARTESIAN_POINT('Origin',(-2.534618881586,81.5,26.567313989381));
#44887=CARTESIAN_POINT('',(2.76031578375735,79.6618619471864,25.842803541876));
#44888=CARTESIAN_POINT('',(3.16550185066553,79.6618619471865,22.1650563712315));
#44889=CARTESIAN_POINT('',(-2.39225620942908,87.,25.2751325510465));
#44890=CARTESIAN_POINT('Origin',(-2.39225620942908,81.5,25.2751325510465));
#44891=CARTESIAN_POINT('',(-2.12943281467784,87.,22.8895668187365));
#44892=CARTESIAN_POINT('',(-2.39225620942908,87.,25.2751325510465));
#44893=CARTESIAN_POINT('',(3.02313917850861,79.6618619471865,23.4572378095661));
#44894=CARTESIAN_POINT('Origin',(-2.12943281467784,81.5,22.8895668187365));
#44895=CARTESIAN_POINT('',(3.16550185066553,79.6618619471865,22.1650563712315));
#44896=CARTESIAN_POINT('',(3.16550185066553,79.6618619471865,22.1650563712315));
#44897=CARTESIAN_POINT('Origin',(-1.98707014252092,81.5,21.597385380402));
#44898=CARTESIAN_POINT('Origin',(2.61795311160045,83.3381380528135,27.1349849802106));
#44899=CARTESIAN_POINT('',(2.50424436804811,84.204163456598,23.6012800800187));
#44900=CARTESIAN_POINT('Origin',(3.00123722894601,83.3381380528135,23.6560349539252));
#44901=CARTESIAN_POINT('',(2.28522487242207,84.204163456598,25.5892515236103));
#44902=CARTESIAN_POINT('Origin',(2.78221773331998,83.3381380528135,25.6440063975169));
#44903=CARTESIAN_POINT('',(2.12096025070255,84.204163456598,27.0802301063041));
#44904=CARTESIAN_POINT('Origin',(-12.6095156787167,81.500000021449,118.014000374155));
#44905=CARTESIAN_POINT('',(1.82040912887033,81.500000021449,18.9987123119195));
#44906=CARTESIAN_POINT('Origin',(-1.658540897415,81.500000021449,18.615428194574));
#44907=CARTESIAN_POINT('',(-9.13056565243138,81.500000021449,118.3972844915));
#44908=CARTESIAN_POINT('',(-9.13056565243138,81.500000021449,118.3972844915));
#44909=CARTESIAN_POINT('Origin',(-12.6095156787167,81.500000021449,118.014000374155));
#44910=CARTESIAN_POINT('Origin',(-12.6095156787167,81.500000021449,118.014000374155));
#44911=CARTESIAN_POINT('Origin',(-12.0072120651665,81.5,112.547078904341));
#44912=CARTESIAN_POINT('Origin',(-11.7881925695404,81.5,110.55910746075));
#44913=CARTESIAN_POINT('',(-11.7662906199778,86.0000000007944,110.36031031639));
#44914=CARTESIAN_POINT('Origin',(-11.7662906199778,81.5,110.360310316391));
#44915=CARTESIAN_POINT('',(-12.0291140147291,86.0000000007944,112.7458760487));
#44916=CARTESIAN_POINT('',(-11.7662906199778,86.,110.360310316391));
#44917=CARTESIAN_POINT('Origin',(-12.0291140147291,81.5,112.7458760487));
#44918=CARTESIAN_POINT('Origin',(-1.658540897415,81.500000021449,18.615428194574));
#44919=CARTESIAN_POINT('Origin',(0.918613714880988,78.570620200579,26.5704957561906));
#44920=CARTESIAN_POINT('',(0.987057307264123,78.570620200579,25.9492546800682));
#44921=CARTESIAN_POINT('',(0.932302433357615,78.570620200579,26.4462475409661));
#44922=CARTESIAN_POINT('Origin',(1.38403014308631,78.570620200579,22.3460564385584));
#44923=CARTESIAN_POINT('',(1.36065466016491,78.5789363869598,22.4692374401316));
#44924=CARTESIAN_POINT('',(1.31558655070317,78.570620200579,22.9672975146808));
#44925=CARTESIAN_POINT('Origin',(4.9436803483069,84.8504809471617,25.3791144897641));
#44926=CARTESIAN_POINT('',(4.51618082872696,85.5,25.8350411952321));
#44927=CARTESIAN_POINT('',(5.00134414567056,85.75,25.3854674461182));
#44928=CARTESIAN_POINT('Origin',(4.57093570263347,85.5,25.3380483343342));
#44929=CARTESIAN_POINT('',(5.01317368962486,84.6339745962156,25.8897960691386));
#44930=CARTESIAN_POINT('',(5.01317368962486,84.6339745962156,25.8897960691386));
#44931=CARTESIAN_POINT('',(5.49833700656846,84.8839745962156,25.4402223200247));
#44932=CARTESIAN_POINT('Origin',(5.06792856353137,84.6339745962156,25.3928032082407));
#44933=CARTESIAN_POINT('',(5.37408879134399,85.1004809471617,25.4265336015481));
#44934=CARTESIAN_POINT('Origin',(5.44358213266196,84.8839745962156,25.9372151809226));
#44935=CARTESIAN_POINT('',(0.812803082748461,79.4245321397111,25.4270313474792));
#44936=CARTESIAN_POINT('',(5.44358213266196,84.8839745962156,25.9372151809226));
#44937=CARTESIAN_POINT('',(2.28522487242207,84.204163456598,25.5892515236103));
#44938=CARTESIAN_POINT('Origin',(2.12096025070255,84.204163456598,27.0802301063041));
#44939=CARTESIAN_POINT('',(5.11085389348358,85.75,24.3914817243224));
#44940=CARTESIAN_POINT('',(4.78232465004453,85.75,27.3734388897098));
#44941=CARTESIAN_POINT('',(4.73520032435299,85.5,23.8470697516405));
#44942=CARTESIAN_POINT('Origin',(4.68044545044649,85.5,24.3440626125384));
#44943=CARTESIAN_POINT('',(2.50424436804811,84.204163456598,23.6012800800187));
#44944=CARTESIAN_POINT('Origin',(0.758048208841953,79.4245321397111,25.9240242083771));
#44945=CARTESIAN_POINT('Origin',(-6.46000589060205,81.5,21.1045915152434));
#44946=CARTESIAN_POINT('',(1.84890551511204,77.5494703669995,22.0200038523508));
#44947=CARTESIAN_POINT('',(5.39645780697042,78.3660254037844,22.4108460428533));
#44948=CARTESIAN_POINT('',(5.82686625000751,78.1160254037844,22.4582651546373));
#44949=CARTESIAN_POINT('',(4.89946494607252,77.5,22.3560911689468));
#44950=CARTESIAN_POINT('',(4.89946494607252,77.5,22.3560911689468));
#44951=CARTESIAN_POINT('',(5.32987338910961,77.25,22.4035102807308));
#44952=CARTESIAN_POINT('Origin',(5.17743831134439,84.6339745962156,24.3988174864449));
#44953=CARTESIAN_POINT('',(5.60784675438148,84.8839745962156,24.4462365982289));
#44954=CARTESIAN_POINT('',(5.11085389348358,85.75,24.3914817243224));
#44955=CARTESIAN_POINT('',(5.2321931852509,84.6339745962156,23.901824625547));
#44956=CARTESIAN_POINT('Origin',(5.17743831134439,84.6339745962156,24.3988174864449));
#44957=CARTESIAN_POINT('',(5.2321931852509,84.6339745962156,23.901824625547));
#44958=CARTESIAN_POINT('Origin',(1.63819716446086,78.9509609731971,23.0028402857485));
#44959=CARTESIAN_POINT('',(1.03182257837449,79.4245321397111,23.4390599038876));
#44960=CARTESIAN_POINT('Origin',(-5.96583445235644,83.8354360064825,25.6862635551102));
#44961=CARTESIAN_POINT('',(-6.02058932626295,83.8354360064825,26.1832564160081));
#44962=CARTESIAN_POINT('Origin',(-8.00154035146294,81.5,25.9650103764094));
#44963=CARTESIAN_POINT('',(4.35191620700744,77.5,27.3260197779258));
#44964=CARTESIAN_POINT('',(4.78232465004453,77.25,27.3734388897098));
#44965=CARTESIAN_POINT('',(4.84890906790534,78.3660254037844,27.3807746518323));
#44966=CARTESIAN_POINT('',(4.84890906790534,78.3660254037844,27.3807746518323));
#44967=CARTESIAN_POINT('',(5.27931751094243,78.1160254037844,27.4281937636163));
#44968=CARTESIAN_POINT('Origin',(3.16550185066553,83.3381380528135,22.1650563712315));
#44969=CARTESIAN_POINT('',(5.66260162828799,84.8839745962156,23.949243737331));
#44970=CARTESIAN_POINT('',(5.82686625000751,84.8839745962156,22.4582651546373));
#44971=CARTESIAN_POINT('Origin',(5.66260162828799,84.8839745962156,23.949243737331));
#44972=CARTESIAN_POINT('Origin',(1.04773081085198,78.1902794279609,22.4347618827151));
#44973=CARTESIAN_POINT('Origin',(5.29195648048422,85.1004809471617,26.172022892895));
#44974=CARTESIAN_POINT('Origin',(-2.19513866336565,86.75,23.485958251814));
#44975=CARTESIAN_POINT('',(-2.39225620942908,86.,25.2751325510465));
#44976=CARTESIAN_POINT('',(-2.12943281467784,87.,22.8895668187365));
#44977=CARTESIAN_POINT('Origin',(4.90366394181185,78.3660254037844,26.8837817909344));
#44978=CARTESIAN_POINT('',(4.83707952395104,77.25,26.8764460288119));
#44979=CARTESIAN_POINT('Origin',(4.40667108091395,77.5,26.8290269170279));
#44980=CARTESIAN_POINT('',(5.33407238484894,78.1160254037844,26.9312009027185));
#44981=CARTESIAN_POINT('',(5.20982416962446,77.8995190528383,26.9175121842418));
#44982=CARTESIAN_POINT('Origin',(4.90366394181185,78.3660254037844,26.8837817909344));
#44983=CARTESIAN_POINT('Origin',(5.29195648048422,77.8995190528383,26.172022892895));
#44984=CARTESIAN_POINT('',(5.2751185152031,77.25,22.9005031416287));
#44985=CARTESIAN_POINT('',(4.78232465004453,77.25,27.3734388897098));
#44986=CARTESIAN_POINT('',(5.772111376101,78.1160254037844,22.9552580155352));
#44987=CARTESIAN_POINT('',(5.64786316087653,77.8995190528383,22.9415692970586));
#44988=CARTESIAN_POINT('',(5.82686625000751,78.1160254037844,22.4582651546373));
#44989=CARTESIAN_POINT('Origin',(5.82686625000751,78.1160254037844,22.4582651546373));
#44990=CARTESIAN_POINT('Origin',(5.34170293306391,78.3660254037844,22.9078389037512));
#44991=CARTESIAN_POINT('',(4.3538213781796,78.8889436754855,23.603842201269));
#44992=CARTESIAN_POINT('',(3.02313917850861,79.6618619471865,23.4572378095661));
#44993=CARTESIAN_POINT('',(4.09099798342836,78.8889436754855,25.9894079335789));
#44994=CARTESIAN_POINT('',(4.09099798342836,78.8889436754855,25.9894079335789));
#44995=CARTESIAN_POINT('',(2.76031578375737,79.6618619471865,25.842803541876));
#44996=CARTESIAN_POINT('Origin',(4.16386731426731,78.6724373245393,24.1865449158698));
#44997=CARTESIAN_POINT('',(3.85682851728169,78.022918271701,23.5490873273625));
#44998=CARTESIAN_POINT('',(4.3538213781796,78.8889436754855,23.603842201269));
#44999=CARTESIAN_POINT('',(3.59400512253045,78.022918271701,25.9346530596724));
#45000=CARTESIAN_POINT('',(3.85682851728169,78.022918271701,23.5490873273625));
#45001=CARTESIAN_POINT('',(3.59400512253045,78.022918271701,25.9346530596724));
#45002=CARTESIAN_POINT('Origin',(-2.12943281467784,87.,22.8895668187365));
#45003=CARTESIAN_POINT('',(2.52614631761071,78.795836543402,23.4024829356596));
#45004=CARTESIAN_POINT('Origin',(4.78232465004453,77.25,27.3734388897098));
#45005=CARTESIAN_POINT('Origin',(4.84471007216601,77.5,22.8530840298447));
#45006=CARTESIAN_POINT('',(2.26332292285947,78.795836543402,25.7880486679695));
#45007=CARTESIAN_POINT('Origin',(-2.39225620942908,86.,25.2751325510465));
#45008=CARTESIAN_POINT('Origin',(4.84471007216601,77.5,22.8530840298447));
#45009=CARTESIAN_POINT('Origin',(-11.8319964686657,86.75,110.956701749468));
#45010=CARTESIAN_POINT('',(-12.0291140147291,86.,112.7458760487));
#45011=CARTESIAN_POINT('',(-11.7662906199778,87.,110.360310316391));
#45012=CARTESIAN_POINT('Origin',(-4.73319386348815,78.3660254037844,114.354525288588));
#45013=CARTESIAN_POINT('',(-4.79977828134896,77.25,114.347189526466));
#45014=CARTESIAN_POINT('',(-5.28494159829256,77.5,114.79676327558));
#45015=CARTESIAN_POINT('Origin',(-5.23018672438606,77.5,114.299770414682));
#45016=CARTESIAN_POINT('',(-4.30278542045106,78.1160254037844,114.401944400372));
#45017=CARTESIAN_POINT('',(-4.42703363567554,77.8995190528383,114.388255681896));
#45018=CARTESIAN_POINT('',(-4.78794873739466,78.3660254037844,114.851518149486));
#45019=CARTESIAN_POINT('Origin',(-4.73319386348815,78.3660254037844,114.354525288588));
#45020=CARTESIAN_POINT('',(-4.78794873739466,78.3660254037844,114.851518149486));
#45021=CARTESIAN_POINT('Origin',(-4.34490132481578,77.8995190528383,113.642766390549));
#45022=CARTESIAN_POINT('',(-4.3617392900969,77.25,110.371246639283));
#45023=CARTESIAN_POINT('',(-4.85453315525547,77.25,114.844182387364));
#45024=CARTESIAN_POINT('',(-3.864746429199,78.1160254037844,110.426001513189));
#45025=CARTESIAN_POINT('',(-3.98899464442347,77.8995190528383,110.412312794713));
#45026=CARTESIAN_POINT('',(-3.80999155529249,78.1160254037844,109.929008652291));
#45027=CARTESIAN_POINT('Origin',(-3.80999155529249,78.1160254037844,109.929008652291));
#45028=CARTESIAN_POINT('',(-4.24039999832958,78.3660254037844,109.881589540507));
#45029=CARTESIAN_POINT('Origin',(-4.29515487223609,78.3660254037844,110.378582401405));
#45030=CARTESIAN_POINT('',(-3.80999155529249,78.1160254037844,109.929008652291));
#45031=CARTESIAN_POINT('',(-5.28303642712041,78.8889436754855,111.074585698923));
#45032=CARTESIAN_POINT('',(-6.61371862679139,79.6618619471865,110.92798130722));
#45033=CARTESIAN_POINT('',(-5.54585982187164,78.8889436754855,113.460151431233));
#45034=CARTESIAN_POINT('',(-5.54585982187164,78.8889436754855,113.460151431233));
#45035=CARTESIAN_POINT('',(-6.87654202154263,79.6618619471865,113.31354703953));
#45036=CARTESIAN_POINT('',(-4.35754029435757,78.1160254037844,114.89893726127));
#45037=CARTESIAN_POINT('Origin',(-5.47299049103269,78.6724373245393,111.657288413524));
#45038=CARTESIAN_POINT('',(-5.78002928801831,78.022918271701,111.019830825016));
#45039=CARTESIAN_POINT('',(-5.28303642712041,78.8889436754855,111.074585698923));
#45040=CARTESIAN_POINT('',(-6.04285268276955,78.022918271701,113.405396557326));
#45041=CARTESIAN_POINT('',(-5.78002928801831,78.022918271701,111.019830825016));
#45042=CARTESIAN_POINT('',(-6.04285268276955,78.022918271701,113.405396557326));
#45043=CARTESIAN_POINT('Origin',(-11.7662906199778,87.,110.360310316391));
#45044=CARTESIAN_POINT('',(-7.11071148768929,78.795836543402,110.873226433314));
#45045=CARTESIAN_POINT('Origin',(-4.85453315525547,77.25,114.844182387364));
#45046=CARTESIAN_POINT('',(-4.73739285922748,77.5,109.826834666601));
#45047=CARTESIAN_POINT('',(-4.30698441619039,77.25,109.874253778385));
#45048=CARTESIAN_POINT('Origin',(-4.79214773313399,77.5,110.323827527499));
#45049=CARTESIAN_POINT('',(-4.85453315525547,77.25,114.844182387364));
#45050=CARTESIAN_POINT('',(-7.37353488244053,78.795836543402,113.258792165624));
#45051=CARTESIAN_POINT('Origin',(-4.30698441619039,77.25,109.874253778385));
#45052=CARTESIAN_POINT('',(-4.73739285922748,77.5,109.826834666601));
#45053=CARTESIAN_POINT('',(-7.78795229018796,77.5494703669995,109.490747350005));
#45054=CARTESIAN_POINT('Origin',(-4.35754029435757,78.1160254037844,114.89893726127));
#45055=CARTESIAN_POINT('',(-15.657447131563,83.8354360064825,113.653999913662));
#45056=CARTESIAN_POINT('Origin',(-12.0291140147291,86.,112.7458760487));
#45057=CARTESIAN_POINT('Origin',(-4.79214773313399,77.5,110.323827527499));
#45058=CARTESIAN_POINT('Origin',(-8.71824409041901,78.570620200579,114.041239253845));
#45059=CARTESIAN_POINT('',(-8.64980049803588,78.570620200579,113.419998177722));
#45060=CARTESIAN_POINT('',(-8.70455537194238,78.570620200579,113.91699103862));
#45061=CARTESIAN_POINT('Origin',(-8.25282766221369,78.570620200579,109.816799936212));
#45062=CARTESIAN_POINT('',(-8.27620314513509,78.5789363869598,109.939980937786));
#45063=CARTESIAN_POINT('',(-8.32127125459683,78.570620200579,110.438041012335));
#45064=CARTESIAN_POINT('Origin',(-4.6931774569931,84.8504809471617,112.849857987418));
#45065=CARTESIAN_POINT('',(-5.12067697657304,85.5,113.305784692886));
#45066=CARTESIAN_POINT('',(-4.63551365962944,85.75,112.856210943772));
#45067=CARTESIAN_POINT('Origin',(-5.06592210266653,85.5,112.808791831988));
#45068=CARTESIAN_POINT('',(-4.62368411567514,84.6339745962156,113.360539566793));
#45069=CARTESIAN_POINT('',(-4.62368411567514,84.6339745962156,113.360539566793));
#45070=CARTESIAN_POINT('',(-4.13852079873154,84.8839745962156,112.910965817679));
#45071=CARTESIAN_POINT('Origin',(-4.56892924176863,84.6339745962156,112.863546705895));
#45072=CARTESIAN_POINT('',(-4.26276901395601,85.1004809471617,112.897277099202));
#45073=CARTESIAN_POINT('Origin',(-4.19327567263805,84.8839745962156,113.407958678577));
#45074=CARTESIAN_POINT('',(-8.82405472255154,79.4245321397111,112.897774845133));
#45075=CARTESIAN_POINT('',(-4.19327567263805,84.8839745962156,113.407958678577));
#45076=CARTESIAN_POINT('',(-7.35163293287793,84.204163456598,113.059995021264));
#45077=CARTESIAN_POINT('Origin',(-7.51589755459745,84.204163456598,114.550973603958));
#45078=CARTESIAN_POINT('',(-4.52600391181642,85.75,111.862225221976));
#45079=CARTESIAN_POINT('',(-4.85453315525547,85.75,114.844182387364));
#45080=CARTESIAN_POINT('',(-4.90165748094701,85.5,111.317813249294));
#45081=CARTESIAN_POINT('Origin',(-4.95641235485351,85.5,111.814806110192));
#45082=CARTESIAN_POINT('',(-7.13261343725189,84.204163456598,111.072023577673));
#45083=CARTESIAN_POINT('Origin',(-8.87880959645805,79.4245321397111,113.394767706031));
#45084=CARTESIAN_POINT('Origin',(-4.45941949395561,84.6339745962156,111.869560984099));
#45085=CARTESIAN_POINT('',(-4.02901105091852,84.8839745962156,111.916980095883));
#45086=CARTESIAN_POINT('',(-4.52600391181642,85.75,111.862225221976));
#45087=CARTESIAN_POINT('',(-4.4046646200491,84.6339745962156,111.372568123201));
#45088=CARTESIAN_POINT('Origin',(-4.45941949395561,84.6339745962156,111.869560984099));
#45089=CARTESIAN_POINT('',(-4.4046646200491,84.6339745962156,111.372568123201));
#45090=CARTESIAN_POINT('Origin',(-7.99866064083914,78.9509609731971,110.473583783403));
#45091=CARTESIAN_POINT('',(-8.60503522692551,79.4245321397111,110.909803401542));
#45092=CARTESIAN_POINT('Origin',(-15.6026922576564,83.8354360064825,113.157007052764));
#45093=CARTESIAN_POINT('Origin',(-6.47135595463447,83.3381380528135,109.635799868886));
#45094=CARTESIAN_POINT('',(-3.97425617701201,84.8839745962156,111.419987234985));
#45095=CARTESIAN_POINT('',(-3.80999155529249,84.8839745962156,109.929008652291));
#45096=CARTESIAN_POINT('Origin',(-3.97425617701201,84.8839745962156,111.419987234985));
#45097=CARTESIAN_POINT('Origin',(-8.58912699444802,78.1902794279609,109.905505380369));
#45098=CARTESIAN_POINT('Origin',(-4.34490132481578,85.1004809471617,113.642766390549));
#45099=CARTESIAN_POINT('Origin',(-12.5547608195654,81.500000018974,117.517007511631));
#45100=CARTESIAN_POINT('Origin',(-11.2953987197157,81.500000018974,106.086171710979));
#45101=CARTESIAN_POINT('Origin',(-12.6095156934719,81.500000018974,118.014000372529));
#45102=CARTESIAN_POINT('Origin',(-14.7997106497322,77.000000018974,137.893714808445));
#45103=CARTESIAN_POINT('Origin',(-4.40913348865652,75.500000018974,118.917455791986));
#45104=CARTESIAN_POINT('',(-4.9566822277216,75.500000018974,123.887384400965));
#45105=CARTESIAN_POINT('',(-21.3574466373524,75.500000018974,122.080473562051));
#45106=CARTESIAN_POINT('',(-4.9566822277216,75.500000018974,123.887384400965));
#45107=CARTESIAN_POINT('',(-20.8098978982873,75.500000018974,117.110544953072));
#45108=CARTESIAN_POINT('',(-20.8098978982873,75.500000018974,117.110544953072));
#45109=CARTESIAN_POINT('',(-4.40913348865652,75.500000018974,118.917455791986));
#45110=CARTESIAN_POINT('',(-4.40913348865652,75.500000018974,118.917455791986));
#45111=CARTESIAN_POINT('',(-4.40913348865652,75.500000018974,118.917455791986));
#45112=CARTESIAN_POINT('Origin',(-20.8098978982873,75.500000018974,117.110544953072));
#45113=CARTESIAN_POINT('',(-21.3574466373524,87.500000018974,122.080473562051));
#45114=CARTESIAN_POINT('',(-21.3574466373524,75.500000018974,122.080473562051));
#45115=CARTESIAN_POINT('',(-20.8098978982873,87.500000018974,117.110544953072));
#45116=CARTESIAN_POINT('',(-20.8098978982873,87.500000018974,117.110544953072));
#45117=CARTESIAN_POINT('',(-20.8098978982873,75.500000018974,117.110544953072));
#45118=CARTESIAN_POINT('Origin',(-6.07285864919602,72.500000018974,140.867273982354));
#45119=CARTESIAN_POINT('',(-4.21119293637475,73.000000018974,123.969516711825));
#45120=CARTESIAN_POINT('',(-4.21119293637475,90.000000018974,123.969516711825));
#45121=CARTESIAN_POINT('',(-4.21119293637475,72.500000018974,123.969516711825));
#45122=CARTESIAN_POINT('',(-6.07285864919602,90.000000018974,140.867273982354));
#45123=CARTESIAN_POINT('',(-6.07285864919602,90.000000018974,140.867273982354));
#45124=CARTESIAN_POINT('',(-6.07285864919602,73.000000018974,140.867273982354));
#45125=CARTESIAN_POINT('',(-6.07285864919602,72.500000018974,140.867273982354));
#45126=CARTESIAN_POINT('',(-6.07285864919602,73.000000018974,140.867273982354));
#45127=CARTESIAN_POINT('Origin',(-6.56985151009392,73.000000018974,140.812519108447));
#45128=CARTESIAN_POINT('',(-6.56985151009392,72.500000018974,140.812519108447));
#45129=CARTESIAN_POINT('Origin',(-6.56985151009392,73.000000018974,140.812519108447));
#45130=CARTESIAN_POINT('',(-4.70818579727265,72.500000018974,123.914761837919));
#45131=CARTESIAN_POINT('',(-6.56985151009392,72.500000018974,140.812519108447));
#45132=CARTESIAN_POINT('Origin',(-4.70818579727265,73.000000018974,123.914761837919));
#45133=CARTESIAN_POINT('Origin',(-23.9646016415205,72.500000018974,138.89609852172));
#45134=CARTESIAN_POINT('',(-23.4676087806226,72.500000018974,138.950853395626));
#45135=CARTESIAN_POINT('',(-23.9646016415205,72.500000018974,138.89609852172));
#45136=CARTESIAN_POINT('',(-21.6059430678014,72.500000018974,122.053096125097));
#45137=CARTESIAN_POINT('',(-23.4676087806226,72.500000018974,138.950853395626));
#45138=CARTESIAN_POINT('',(-22.1029359286993,72.500000018974,121.998341251191));
#45139=CARTESIAN_POINT('Origin',(-23.4676087806226,73.000000018974,138.950853395626));
#45140=CARTESIAN_POINT('',(-23.9646016415205,73.000000018974,138.89609852172));
#45141=CARTESIAN_POINT('Origin',(-23.4676087806226,73.000000018974,138.950853395626));
#45142=CARTESIAN_POINT('',(-22.1029359286993,73.000000018974,121.998341251191));
#45143=CARTESIAN_POINT('',(-23.9646016415205,73.000000018974,138.89609852172));
#45144=CARTESIAN_POINT('Origin',(-21.6059430678014,73.000000018974,122.053096125097));
#45145=CARTESIAN_POINT('Origin',(-23.9646016415205,90.500000018974,138.89609852172));
#45146=CARTESIAN_POINT('',(-22.1029359286993,90.000000018974,121.998341251191));
#45147=CARTESIAN_POINT('',(-22.1029359286993,90.500000018974,121.998341251191));
#45148=CARTESIAN_POINT('',(-23.9646016415205,90.000000018974,138.89609852172));
#45149=CARTESIAN_POINT('',(-23.9646016415205,90.500000018974,138.89609852172));
#45150=CARTESIAN_POINT('',(-23.9646016415205,90.000000018974,138.89609852172));
#45151=CARTESIAN_POINT('Origin',(-15.0187301453583,81.500000018974,139.881686252037));
#45152=CARTESIAN_POINT('',(-6.56985151009392,90.500000018974,140.812519108447));
#45153=CARTESIAN_POINT('Origin',(-6.56985151009392,90.000000018974,140.812519108447));
#45154=CARTESIAN_POINT('',(-23.4676087806226,90.500000018974,138.950853395626));
#45155=CARTESIAN_POINT('',(-6.07285864919602,90.500000018974,140.867273982354));
#45156=CARTESIAN_POINT('Origin',(-23.4676087806226,90.000000018974,138.950853395626));
#45157=CARTESIAN_POINT('Origin',(-23.4676087806226,90.000000018974,138.950853395626));
#45158=CARTESIAN_POINT('',(-21.6059430678014,90.500000018974,122.053096125097));
#45159=CARTESIAN_POINT('',(-23.4676087806226,90.500000018974,138.950853395626));
#45160=CARTESIAN_POINT('Origin',(-21.6059430678014,90.000000018974,122.053096125097));
#45161=CARTESIAN_POINT('Origin',(-13.157064432537,81.500000018974,122.983928981508));
#45162=CARTESIAN_POINT('',(-4.70818579727265,90.500000018974,123.914761837919));
#45163=CARTESIAN_POINT('',(-4.21119293637475,90.500000018974,123.969516711825));
#45164=CARTESIAN_POINT('Origin',(-4.70818579727265,90.000000018974,123.914761837919));
#45165=CARTESIAN_POINT('',(-4.9566822277216,87.500000018974,123.887384400965));
#45166=CARTESIAN_POINT('',(-21.3574466373524,87.500000018974,122.080473562051));
#45167=CARTESIAN_POINT('',(-4.9566822277216,87.500000018974,123.887384400965));
#45168=CARTESIAN_POINT('Origin',(-6.07285864919602,90.500000018974,140.867273982354));
#45169=CARTESIAN_POINT('',(-6.56985151009392,90.500000018974,140.812519108447));
#45170=CARTESIAN_POINT('Origin',(-20.8098978982873,87.500000018974,117.110544953072));
#45171=CARTESIAN_POINT('',(-4.40913348865652,87.500000018974,118.917455791986));
#45172=CARTESIAN_POINT('',(-4.40913348865652,87.500000018974,118.917455791986));
#45173=CARTESIAN_POINT('',(-20.8098978982873,87.500000018974,117.110544953072));
#45174=CARTESIAN_POINT('Origin',(-12.6095156934719,81.500000018974,118.014000372529));
#45175=CARTESIAN_POINT('',(-4.40913348865652,87.500000018974,118.917455791986));
#45176=CARTESIAN_POINT('Origin',(-4.40913348865652,87.500000018974,118.917455791986));
#45177=CARTESIAN_POINT('Origin',(-6.56985151009392,90.000000018974,140.812519108447));
#45178=CARTESIAN_POINT('',(0.,0.,0.));
#45179=CARTESIAN_POINT('Origin',(0.,57.,0.));
#45180=CARTESIAN_POINT('',(-1.67399064887303E-12,79.1849791588191,12.1793954854792));
#45181=CARTESIAN_POINT('',(-3.38396588028469,81.4999870102159,11.4475530231091));
#45182=CARTESIAN_POINT('Ctrl Pts',(-3.38396588028469,81.4999870102159,11.4475530231091));
#45183=CARTESIAN_POINT('Ctrl Pts',(-3.38753348202195,81.1933123994846,11.4799495787905));
#45184=CARTESIAN_POINT('Ctrl Pts',(-3.3334689662572,80.8701382063821,11.5316443917672));
#45185=CARTESIAN_POINT('Ctrl Pts',(-3.10178230244334,80.2584031129966,11.6624034476806));
#45186=CARTESIAN_POINT('Ctrl Pts',(-2.91772638565787,79.9722655814763,11.7421072768728));
#45187=CARTESIAN_POINT('Ctrl Pts',(-2.48590576948198,79.5201548688865,11.8893378356882));
#45188=CARTESIAN_POINT('Ctrl Pts',(-2.20964811254668,79.3236980609575,11.9666092782287));
#45189=CARTESIAN_POINT('Ctrl Pts',(-1.59596577782429,79.063039053013,12.0912896144645));
#45190=CARTESIAN_POINT('Ctrl Pts',(-1.25836538845438,78.998920604423,12.1380077071301));
#45191=CARTESIAN_POINT('Ctrl Pts',(-0.63090568596245,79.0010700955652,12.1862255830573));
#45192=CARTESIAN_POINT('Ctrl Pts',(-0.303396633904576,79.0626096753735,
12.1921956406512));
#45193=CARTESIAN_POINT('Ctrl Pts',(-3.35301231224605E-12,79.1849791588191,
12.1793954854792));
#45194=CARTESIAN_POINT('',(-1.77573785876366E-15,57.,14.5));
#45195=CARTESIAN_POINT('',(-1.77573785876366E-15,57.,14.5));
#45196=CARTESIAN_POINT('Origin',(0.,57.,0.));
#45197=CARTESIAN_POINT('',(-2.93399460262726E-12,83.8360320219375,11.6928836797137));
#45198=CARTESIAN_POINT('Ctrl Pts',(-3.35463239703304E-12,79.1849791588191,
12.1793954854792));
#45199=CARTESIAN_POINT('Ctrl Pts',(0.0128218290929213,79.1901506090859,
12.1788545387986));
#45200=CARTESIAN_POINT('Ctrl Pts',(0.0256027230999332,79.1954256888372,
12.1782825024218));
#45201=CARTESIAN_POINT('Ctrl Pts',(0.352471098452155,79.3334249948847,12.1628182515688));
#45202=CARTESIAN_POINT('Ctrl Pts',(0.638723896983974,79.5314817995799,12.1284822027142));
#45203=CARTESIAN_POINT('Ctrl Pts',(1.09095346963654,79.9850955738011,12.0485761528978));
#45204=CARTESIAN_POINT('Ctrl Pts',(1.28733549422776,80.2716995036191,11.997601589275));
#45205=CARTESIAN_POINT('Ctrl Pts',(1.54631117535722,80.8998779199057,11.9007252849027));
#45206=CARTESIAN_POINT('Ctrl Pts',(1.60872112599741,81.241649843226,11.8556144991127));
#45207=CARTESIAN_POINT('Ctrl Pts',(1.59987230256022,81.8707917182341,11.7904023018295));
#45208=CARTESIAN_POINT('Ctrl Pts',(1.53354425429038,82.1986249422797,11.7653209410141));
#45209=CARTESIAN_POINT('Ctrl Pts',(1.27309593871425,82.8002861327028,11.7330462201679));
#45210=CARTESIAN_POINT('Ctrl Pts',(1.0790616457523,83.0741106544731,11.7250993121732));
#45211=CARTESIAN_POINT('Ctrl Pts',(0.634795438436527,83.5062206065111,11.7122867739736));
#45212=CARTESIAN_POINT('Ctrl Pts',(0.354224746857852,83.6933714014299,11.7064436317575));
#45213=CARTESIAN_POINT('Ctrl Pts',(0.0322540850921523,83.8235665140971,
11.6941541060662));
#45214=CARTESIAN_POINT('Ctrl Pts',(0.0161573344640062,83.829883146393,11.6935268675321));
#45215=CARTESIAN_POINT('Ctrl Pts',(-5.86466963477889E-12,83.8360320219375,
11.6928836797137));
#45216=CARTESIAN_POINT('',(-1.16341445918999E-15,104.8,9.5));
#45217=CARTESIAN_POINT('',(-1.77573785876366E-15,57.,14.5));
#45218=CARTESIAN_POINT('Origin',(7.9959910220806E-15,104.8,-1.0842021724855E-15));
#45219=CARTESIAN_POINT('Ctrl Pts',(-5.86329595986257E-12,83.8360320219375,
11.6928836797137));
#45220=CARTESIAN_POINT('Ctrl Pts',(-0.292206849548209,83.9472349901267,
11.6812515700703));
#45221=CARTESIAN_POINT('Ctrl Pts',(-0.605183114261111,84.0009910985821,
11.6636507998233));
#45222=CARTESIAN_POINT('Ctrl Pts',(-1.20746904872849,83.9989278453149,11.6173674315919));
#45223=CARTESIAN_POINT('Ctrl Pts',(-1.53614415691599,83.9368086460649,11.5848936853051));
#45224=CARTESIAN_POINT('Ctrl Pts',(-2.14059633569514,83.6860882677134,11.5152419644677));
#45225=CARTESIAN_POINT('Ctrl Pts',(-2.41645415653066,83.4974908811631,11.4787528322036));
#45226=CARTESIAN_POINT('Ctrl Pts',(-2.85408198422145,83.0627090933434,11.4247140734898));
#45227=CARTESIAN_POINT('Ctrl Pts',(-3.04540036527166,82.7870995589041,11.4036356546425));
#45228=CARTESIAN_POINT('Ctrl Pts',(-3.30525144654228,82.1828149966382,11.3968748343011));
#45229=CARTESIAN_POINT('Ctrl Pts',(-3.37387872914963,81.8541729218928,11.4119012851098));
#45230=CARTESIAN_POINT('Ctrl Pts',(-3.38301135031416,81.5462246274869,11.4427917170341));
#45231=CARTESIAN_POINT('Ctrl Pts',(-3.38346694495989,81.5308621601771,11.4443327330399));
#45232=CARTESIAN_POINT('Ctrl Pts',(-3.38378589319777,81.5154521527978,11.4459193363202));
#45233=CARTESIAN_POINT('Ctrl Pts',(-3.3839657291394,81.4999999999901,11.4475516509024));
#45234=CARTESIAN_POINT('',(-10.2705269140488,83.083888358195,5.75203415488913));
#45235=CARTESIAN_POINT('',(-3.31946532069801,102.294971773814,9.1803280694632));
#45236=CARTESIAN_POINT('Ctrl Pts',(-10.2705269140489,83.0838883581951,5.75203415488913));
#45237=CARTESIAN_POINT('Ctrl Pts',(-10.4476447349629,83.8697062565521,5.26756237969859));
#45238=CARTESIAN_POINT('Ctrl Pts',(-10.5532091788737,84.7143876905477,4.83155183883129));
#45239=CARTESIAN_POINT('Ctrl Pts',(-10.7479632171024,87.0817516344024,3.72991645237086));
#45240=CARTESIAN_POINT('Ctrl Pts',(-10.7473242520368,88.8776077562035,3.06361757662507));
#45241=CARTESIAN_POINT('Ctrl Pts',(-10.594496436306,92.541382067534,2.05817978394714));
#45242=CARTESIAN_POINT('Ctrl Pts',(-10.447233979957,94.4082846127597,1.71460227208681));
#45243=CARTESIAN_POINT('Ctrl Pts',(-10.2675344540495,96.1491949155499,1.68510994751507));
#45244=CARTESIAN_POINT('Ctrl Pts',(-10.1605929923517,97.1852326653713,1.66755869198092));
#45245=CARTESIAN_POINT('Ctrl Pts',(-10.0298236278627,98.3185303401197,1.76805440954025));
#45246=CARTESIAN_POINT('Ctrl Pts',(-9.75871203778378,99.8566120410559,2.26774767596806));
#45247=CARTESIAN_POINT('Ctrl Pts',(-9.65425306299935,100.343635521796,2.49213503112639));
#45248=CARTESIAN_POINT('Ctrl Pts',(-9.39760803176894,101.219568637648,3.04670383868021));
#45249=CARTESIAN_POINT('Ctrl Pts',(-9.2447343379093,101.608464265196,3.37658893604804));
#45250=CARTESIAN_POINT('Ctrl Pts',(-8.9118265271853,102.19936754128,4.02180967320626));
#45251=CARTESIAN_POINT('Ctrl Pts',(-8.72795377133198,102.447311056827,4.35566740291926));
#45252=CARTESIAN_POINT('Ctrl Pts',(-8.30128569109916,102.851557097895,5.04135184709664));
#45253=CARTESIAN_POINT('Ctrl Pts',(-8.057826724156,103.008611139308,5.39232191797367));
#45254=CARTESIAN_POINT('Ctrl Pts',(-7.62991618465407,103.199656130708,5.94403340287079));
#45255=CARTESIAN_POINT('Ctrl Pts',(-7.41696214474173,103.267989331379,6.19847559769947));
#45256=CARTESIAN_POINT('Ctrl Pts',(-6.96343445333318,103.356321073249,6.69063353410446));
#45257=CARTESIAN_POINT('Ctrl Pts',(-6.72278744373644,103.376431260001,6.92826162463383));
#45258=CARTESIAN_POINT('Ctrl Pts',(-6.26631946043173,103.376431260001,7.34369937925353));
#45259=CARTESIAN_POINT('Ctrl Pts',(-6.00714274392577,103.356321073249,7.56096769783146));
#45260=CARTESIAN_POINT('Ctrl Pts',(-5.47456973400649,103.267989331379,7.96627349639138));
#45261=CARTESIAN_POINT('Ctrl Pts',(-5.20125381536694,103.199656130708,8.15439224145004));
#45262=CARTESIAN_POINT('Ctrl Pts',(-4.6117960944632,103.008611139308,8.52860152467425));
#45263=CARTESIAN_POINT('Ctrl Pts',(-4.23951420613461,102.851557097895,8.73802562753481));
#45264=CARTESIAN_POINT('Ctrl Pts',(-3.68678689137256,102.542395564135,9.01364757314303));
#45265=CARTESIAN_POINT('Ctrl Pts',(-3.49844040074224,102.423050920468,9.10136711957112));
#45266=CARTESIAN_POINT('Ctrl Pts',(-3.31946532089988,102.294971773896,9.1803280694126));
#45267=CARTESIAN_POINT('Ctrl Pts',(-3.31946532089987,102.294971773896,9.1803280694126));
#45268=CARTESIAN_POINT('Ctrl Pts',(-3.16047808560999,102.181196440315,9.25047070112544));
#45269=CARTESIAN_POINT('Ctrl Pts',(-3.00889185896816,102.060551508221,9.31375238255998));
#45270=CARTESIAN_POINT('Ctrl Pts',(-2.49351051375685,101.608464265196,9.52097007344027));
#45271=CARTESIAN_POINT('Ctrl Pts',(-2.15072712555426,101.219568637648,9.64218926545221));
#45272=CARTESIAN_POINT('Ctrl Pts',(-1.57450795246704,100.343635521796,9.84562156115182));
#45273=CARTESIAN_POINT('Ctrl Pts',(-1.34130263815093,99.856612041056,9.92854709366551));
#45274=CARTESIAN_POINT('Ctrl Pts',(-0.818357974109837,98.3185303401197,
10.1515352842484));
#45275=CARTESIAN_POINT('Ctrl Pts',(-0.706026039872255,97.1852326653713,
10.2722893835041));
#45276=CARTESIAN_POINT('Ctrl Pts',(-0.725943775135968,94.4082846127598,
10.5620814434823));
#45277=CARTESIAN_POINT('Ctrl Pts',(-1.05417380953003,92.541382067534,10.7409578875094));
#45278=CARTESIAN_POINT('Ctrl Pts',(-2.04081663585263,88.8776077562036,10.9875292351398));
#45279=CARTESIAN_POINT('Ctrl Pts',(-2.70411103697154,87.0817516344024,11.0507363355381));
#45280=CARTESIAN_POINT('Ctrl Pts',(-4.16467604316353,83.9808413773662,10.9322718155721));
#45281=CARTESIAN_POINT('Ctrl Pts',(-5.15529103297173,82.2348877175806,10.7555894278755));
#45282=CARTESIAN_POINT('Ctrl Pts',(-6.55855196256495,80.8708129924728,10.0572521181665));
#45283=CARTESIAN_POINT('Ctrl Pts',(-6.86925488573727,80.6168547487457,9.88291613982572));
#45284=CARTESIAN_POINT('Ctrl Pts',(-7.50690254096133,80.2600262722913,9.45539631479147));
#45285=CARTESIAN_POINT('Ctrl Pts',(-7.83435236046293,80.1604325456248,9.20023978223745));
#45286=CARTESIAN_POINT('Ctrl Pts',(-8.42387230776362,80.1604325456248,8.66370961546201));
#45287=CARTESIAN_POINT('Ctrl Pts',(-8.70865150525079,80.2600262722913,8.36166814633042));
#45288=CARTESIAN_POINT('Ctrl Pts',(-9.19416243184007,80.6168547487457,7.76698598485886));
#45289=CARTESIAN_POINT('Ctrl Pts',(-9.39690556109689,80.8708129924728,7.47402768859298));
#45290=CARTESIAN_POINT('Ctrl Pts',(-9.87846340427557,81.6650788027622,6.69874090289468));
#45291=CARTESIAN_POINT('Ctrl Pts',(-10.1049688770831,82.349357705135,6.20488636169666));
#45292=CARTESIAN_POINT('Ctrl Pts',(-10.2705269140489,83.0838883581951,5.75203415488912));
#45293=CARTESIAN_POINT('Origin',(-26.2797781582403,69.3521366901578,34.6133035514349));
#45294=CARTESIAN_POINT('',(-26.7739714403084,76.2801240271818,35.1563052606437));
#45295=CARTESIAN_POINT('',(-20.4910969480847,73.0785942424389,35.6813720681732));
#45296=CARTESIAN_POINT('Origin',(-24.1889142881135,73.0785942424389,32.3159379327633));
#45297=CARTESIAN_POINT('',(-28.8648353104351,72.5536664749007,37.4536708793154));
#45298=CARTESIAN_POINT('',(-28.8648353104351,72.5536664749007,37.4536708793154));
#45299=CARTESIAN_POINT('',(-22.5819608182114,69.3521366901579,37.9787376868449));
#45300=CARTESIAN_POINT('Origin',(-26.2797781582403,69.3521366901579,34.6133035514349));
#45301=CARTESIAN_POINT('',(-13.4013316692759,85.7143806963486,27.8913943327985));
#45302=CARTESIAN_POINT('Origin',(3.25260651745652E-16,57.,24.));
#45303=CARTESIAN_POINT('',(-4.19913133791449,61.,27.5520833333334));
#45304=CARTESIAN_POINT('',(4.19913133791449,61.,27.5520833333334));
#45305=CARTESIAN_POINT('Origin',(3.25260651745652E-16,61.,24.));
#45306=CARTESIAN_POINT('',(-4.19913133791449,57.,27.5520833333334));
#45307=CARTESIAN_POINT('',(-4.19913133791449,57.,27.5520833333334));
#45308=CARTESIAN_POINT('',(4.19913133791449,57.,27.5520833333334));
#45309=CARTESIAN_POINT('Origin',(3.25260651745652E-16,57.,24.));
#45310=CARTESIAN_POINT('',(4.19913133791449,57.,27.5520833333334));
#45311=CARTESIAN_POINT('Origin',(-0.549839823016682,81.5,8.55209539435995));
#45312=CARTESIAN_POINT('',(-3.48644671444823,81.5,12.3777394943305));
#45313=CARTESIAN_POINT('',(-3.0348041275062,81.5,8.27832102482741));
#45314=CARTESIAN_POINT('Origin',(-1.00148240995872,81.5,12.651513863863));
#45315=CARTESIAN_POINT('Origin',(3.03576608295941E-15,159.117852690362,
24.));
#45316=CARTESIAN_POINT('',(3.33684549852979E-15,57.,26.4585));
#45317=CARTESIAN_POINT('Origin',(3.03576608295941E-15,57.,24.));
#45318=CARTESIAN_POINT('',(3.33684549852979E-15,61.,26.4585));
#45319=CARTESIAN_POINT('',(3.33684549852979E-15,159.117852690362,26.4585));
#45320=CARTESIAN_POINT('Origin',(3.03576608295941E-15,61.,24.));
#45321=CARTESIAN_POINT('Origin',(-0.853633368077759,103.27860563435,0.937941479018354));
#45322=CARTESIAN_POINT('',(-23.6804219928968,66.0065065859266,31.5522110460941));
#45323=CARTESIAN_POINT('Origin',(-23.6804219928968,62.5953932642765,26.0191914449304));
#45324=CARTESIAN_POINT('',(-0.853633368077761,106.689718956,6.47096108018202));
#45325=CARTESIAN_POINT('Origin',(14.1109635503163,148.485307824806,-15.7093526802252));
#45326=CARTESIAN_POINT('',(-29.8584457467901,70.9711830222491,33.98249436695));
#45327=CARTESIAN_POINT('Origin',(-29.8584457467901,70.1205038384961,32.6026444017984));
#45328=CARTESIAN_POINT('',(-27.7675818766634,74.6976405745302,31.6851287482784));
#45329=CARTESIAN_POINT('',(14.1109635503163,149.335987008559,-14.3295027150735));
#45330=CARTESIAN_POINT('Origin',(-27.7675818766633,73.8469613907772,30.3052787831267));
#45331=CARTESIAN_POINT('Origin',(1.3010426069826E-15,159.117852690362,-24.));
#45332=CARTESIAN_POINT('',(1.60212202255298E-15,57.,-21.5415));
#45333=CARTESIAN_POINT('Origin',(1.3010426069826E-15,57.,-24.));
#45334=CARTESIAN_POINT('',(1.60212202255298E-15,61.,-21.5415));
#45335=CARTESIAN_POINT('',(1.60212202255298E-15,159.117852690362,-21.5415));
#45336=CARTESIAN_POINT('Origin',(1.3010426069826E-15,61.,-24.));
#45337=CARTESIAN_POINT('Origin',(-14.9738587466477,89.2,-14.7235713818163));
#45338=CARTESIAN_POINT('',(-14.9738587466477,104.8,-18.2235713818163));
#45339=CARTESIAN_POINT('Origin',(-14.9738587466477,104.8,-14.7235713818163));
#45340=CARTESIAN_POINT('',(-14.9738587466477,97.,-18.2235713818163));
#45341=CARTESIAN_POINT('',(-14.9738587466477,89.2,-18.2235713818163));
#45342=CARTESIAN_POINT('Origin',(-14.9738587466477,97.,-14.7235713818163));
#45343=CARTESIAN_POINT('Origin',(14.8492424010046,89.2,14.8492423986296));
#45344=CARTESIAN_POINT('',(14.8492424010046,104.8,11.3492423986258));
#45345=CARTESIAN_POINT('Origin',(14.8492424010046,104.8,14.8492423986296));
#45346=CARTESIAN_POINT('',(14.8492424010046,97.,11.3492423986258));
#45347=CARTESIAN_POINT('',(14.8492424010046,89.2,11.3492423986258));
#45348=CARTESIAN_POINT('Origin',(14.8492424010046,97.,14.8492423986296));
#45349=CARTESIAN_POINT('Origin',(-14.9738587466477,104.8,-14.7235713818163));
#45350=CARTESIAN_POINT('',(-13.7983804991702,97.,-21.6241692464732));
#45351=CARTESIAN_POINT('',(-21.8536641357053,97.,-13.4319530911847));
#45352=CARTESIAN_POINT('Origin',(-14.9738587466477,97.,-14.7235713818163));
#45353=CARTESIAN_POINT('',(-21.8536641357053,104.8,-13.4319530911847));
#45354=CARTESIAN_POINT('',(-21.8536641357053,104.8,-13.4319530911847));
#45355=CARTESIAN_POINT('',(-13.7983804991702,104.8,-21.6241692464732));
#45356=CARTESIAN_POINT('Origin',(-14.9738587466477,104.8,-14.7235713818163));
#45357=CARTESIAN_POINT('',(-13.7983804991702,104.8,-21.6241692464732));
#45358=CARTESIAN_POINT('Origin',(-2.9507559210307,81.5,30.3444597118283));
#45359=CARTESIAN_POINT('',(-0.465791616541182,81.5,30.6182340813609));
#45360=CARTESIAN_POINT('Origin',(-2.9507559210307,81.5,30.3444597118283));
#45361=CARTESIAN_POINT('',(-0.686490710462955,81.5,30.7951292761574));
#45362=CARTESIAN_POINT('',(-0.465791616541184,81.5,30.6182340813609));
#45363=CARTESIAN_POINT('Origin',(-2.9726578705933,81.5,30.5432568561875));
#45364=CARTESIAN_POINT('Origin',(-1.6585408968371,81.5,18.6154281946378));
#45365=CARTESIAN_POINT('',(0.588894744914294,81.5,12.8267294603638));
#45366=CARTESIAN_POINT('Origin',(-1.001482409959,81.5,12.651513863863));
#45367=CARTESIAN_POINT('',(-0.0681637419638085,81.5,18.7906437911387));
#45368=CARTESIAN_POINT('',(-0.0681637419638084,81.5,18.7906437911387));
#45369=CARTESIAN_POINT('Origin',(-1.6585408968371,81.5,18.6154281946378));
#45370=CARTESIAN_POINT('Origin',(-2.9726578705933,81.5,30.5432568561875));
#45371=CARTESIAN_POINT('',(0.826423407652414,81.5,18.8892025641704));
#45372=CARTESIAN_POINT('',(-0.487693566103787,81.5,30.8170312257201));
#45373=CARTESIAN_POINT('Origin',(-1.6585408968371,81.5,18.6154281946379));
#45374=CARTESIAN_POINT('Origin',(-1.6585408968371,81.5,18.6154281946378));
#45375=CARTESIAN_POINT('',(-4.71213288373597,81.5,30.3516147975147));
#45376=CARTESIAN_POINT('Origin',(-2.9726578705933,81.5,30.5432568561875));
#45377=CARTESIAN_POINT('',(-3.39801590997976,81.5,18.4237861359651));
#45378=CARTESIAN_POINT('',(-3.39801590997976,81.5,18.4237861359651));
#45379=CARTESIAN_POINT('Origin',(-1.6585408968371,81.5,18.6154281946378));
#45380=CARTESIAN_POINT('Origin',(-2.9726578705933,81.5,30.5432568561875));
#45381=CARTESIAN_POINT('Origin',(-1.6585408968371,81.5,18.6154281946378));
#45382=CARTESIAN_POINT('Origin',(-1.001482409959,81.5,12.651513863863));
#45383=CARTESIAN_POINT('Origin',(-13.7983804991702,104.8,-21.6241692464732));
#45384=CARTESIAN_POINT('',(3.19058381458178,97.,-18.7301942040687));
#45385=CARTESIAN_POINT('',(-13.7983804991702,97.,-21.6241692464732));
#45386=CARTESIAN_POINT('',(3.19058381458178,104.8,-18.7301942040687));
#45387=CARTESIAN_POINT('',(-13.7983804991702,104.8,-21.6241692464732));
#45388=CARTESIAN_POINT('',(3.19058381458178,104.8,-18.7301942040687));
#45389=CARTESIAN_POINT('Origin',(-18.9584411954548,97.,-1.25598862991717));
#45390=CARTESIAN_POINT('',(-18.9584411954548,61.,-1.25598862991717));
#45391=CARTESIAN_POINT('',(-4.34139830399414,61.,-16.347359053955));
#45392=CARTESIAN_POINT('',(-18.9584411954548,61.,-1.25598862991717));
#45393=CARTESIAN_POINT('',(-18.9584411954548,97.,-1.25598862991717));
#45394=CARTESIAN_POINT('',(-18.9584411954548,97.,-1.25598862991717));
#45395=CARTESIAN_POINT('',(-4.34139830399414,97.,-16.347359053955));
#45396=CARTESIAN_POINT('',(-18.9584411954548,97.,-1.25598862991717));
#45397=CARTESIAN_POINT('',(-4.34139830399414,97.,-16.347359053955));
#45398=CARTESIAN_POINT('Origin',(2.55225596709131,97.,-17.5628962976236));
#45399=CARTESIAN_POINT('',(2.55225596709131,61.,-17.5628962976236));
#45400=CARTESIAN_POINT('',(2.55225596709131,61.,-17.5628962976236));
#45401=CARTESIAN_POINT('',(2.55225596709131,97.,-17.5628962976236));
#45402=CARTESIAN_POINT('',(2.55225596709131,97.,-17.5628962976236));
#45403=CARTESIAN_POINT('',(2.55225596709131,97.,-17.5628962976236));
#45404=CARTESIAN_POINT('Origin',(18.9542370742857,97.,-3.8));
#45405=CARTESIAN_POINT('',(18.9542370742857,61.,-3.8));
#45406=CARTESIAN_POINT('',(18.9542370742857,61.,-3.8));
#45407=CARTESIAN_POINT('',(18.542188638435,97.,-4.1457496905495));
#45408=CARTESIAN_POINT('',(18.9542370742857,97.,-3.8));
#45409=CARTESIAN_POINT('',(18.9542370742857,97.,-3.8));
#45410=CARTESIAN_POINT('',(18.9542370742857,97.,-3.8));
#45411=CARTESIAN_POINT('',(18.9542370742857,97.,-3.8));
#45412=CARTESIAN_POINT('Origin',(-21.8536641357053,104.8,-13.4319530911847));
#45413=CARTESIAN_POINT('',(-18.6737574845849,97.,3.50582107457153));
#45414=CARTESIAN_POINT('',(-21.8536641357053,97.,-13.4319530911847));
#45415=CARTESIAN_POINT('',(-18.6737574845849,104.8,3.50582107457153));
#45416=CARTESIAN_POINT('',(-18.6737574845849,104.8,3.50582107457153));
#45417=CARTESIAN_POINT('',(-21.8536641357053,104.8,-13.4319530911847));
#45418=CARTESIAN_POINT('Origin',(4.19913133791449,57.,27.5520833333334));
#45419=CARTESIAN_POINT('',(16.0330469265826,61.,13.5625));
#45420=CARTESIAN_POINT('',(4.19913133791449,61.,27.5520833333334));
#45421=CARTESIAN_POINT('',(16.0330469265826,57.,13.5625));
#45422=CARTESIAN_POINT('',(4.19913133791449,57.,27.5520833333334));
#45423=CARTESIAN_POINT('',(16.0330469265826,57.,13.5625));
#45424=CARTESIAN_POINT('Origin',(3.26019593266391E-16,57.,0.));
#45425=CARTESIAN_POINT('',(16.0330469265826,61.,-13.5625));
#45426=CARTESIAN_POINT('Origin',(3.26019593266391E-16,61.,0.));
#45427=CARTESIAN_POINT('',(16.0330469265826,57.,-13.5625));
#45428=CARTESIAN_POINT('Origin',(3.26019593266391E-16,57.,0.));
#45429=CARTESIAN_POINT('',(16.0330469265826,57.,-13.5625));
#45430=CARTESIAN_POINT('Origin',(4.19913133791449,57.,-27.5520833333334));
#45431=CARTESIAN_POINT('',(4.19913133791449,61.,-27.5520833333334));
#45432=CARTESIAN_POINT('',(4.19913133791449,61.,-27.5520833333334));
#45433=CARTESIAN_POINT('',(4.19913133791449,57.,-27.5520833333334));
#45434=CARTESIAN_POINT('',(4.19913133791449,57.,-27.5520833333334));
#45435=CARTESIAN_POINT('',(4.19913133791449,57.,-27.5520833333334));
#45436=CARTESIAN_POINT('Origin',(3.25260651745652E-16,57.,-24.));
#45437=CARTESIAN_POINT('',(-4.19913133791449,61.,-27.5520833333334));
#45438=CARTESIAN_POINT('Origin',(3.25260651745652E-16,61.,-24.));
#45439=CARTESIAN_POINT('',(-4.19913133791449,57.,-27.5520833333334));
#45440=CARTESIAN_POINT('Origin',(3.25260651745652E-16,57.,-24.));
#45441=CARTESIAN_POINT('',(-4.19913133791449,57.,-27.5520833333334));
#45442=CARTESIAN_POINT('Origin',(-16.0330469265826,57.,-13.5625));
#45443=CARTESIAN_POINT('',(-16.0330469265826,61.,-13.5625));
#45444=CARTESIAN_POINT('',(-16.0330469265826,61.,-13.5625));
#45445=CARTESIAN_POINT('',(-16.0330469265826,57.,-13.5625));
#45446=CARTESIAN_POINT('',(-16.0330469265826,57.,-13.5625));
#45447=CARTESIAN_POINT('',(-16.0330469265826,57.,-13.5625));
#45448=CARTESIAN_POINT('Origin',(3.26019593266391E-16,57.,0.));
#45449=CARTESIAN_POINT('',(-19.4844999727208,61.,7.83289606806087));
#45450=CARTESIAN_POINT('',(-19.4844999727208,57.,7.83289606806088));
#45451=CARTESIAN_POINT('',(-19.4844999727208,57.,7.83289606806088));
#45452=CARTESIAN_POINT('Origin',(3.26019593266391E-16,61.,0.));
#45453=CARTESIAN_POINT('Origin',(3.26019593266391E-16,57.,0.));
#45454=CARTESIAN_POINT('Origin',(-23.0156567533509,85.7143806963486,19.1412655807327));
#45455=CARTESIAN_POINT('',(-34.7813430544813,72.5536664749007,32.0689762626596));
#45456=CARTESIAN_POINT('',(-35.8941032423152,69.3521366901579,25.8631747993693));
#45457=CARTESIAN_POINT('Origin',(-32.1962859022864,69.3521366901579,29.2286089347791));
#45458=CARTESIAN_POINT('',(-32.6904791843545,76.2801240271818,29.771610643988));
#45459=CARTESIAN_POINT('',(-34.7813430544813,72.5536664749007,32.0689762626596));
#45460=CARTESIAN_POINT('',(-33.8032393721885,73.0785942424389,23.5658091806977));
#45461=CARTESIAN_POINT('Origin',(-30.1054220321596,73.0785942424389,26.9312433161075));
#45462=CARTESIAN_POINT('',(-33.8032393721885,73.0785942424389,23.5658091806977));
#45463=CARTESIAN_POINT('Origin',(-4.65835823559196,97.,18.2849312538381));
#45464=CARTESIAN_POINT('',(1.34329598298651,61.,18.9461476330332));
#45465=CARTESIAN_POINT('',(-4.65835823559196,61.,18.2849312538381));
#45466=CARTESIAN_POINT('',(-4.65835823559196,61.,18.2849312538381));
#45467=CARTESIAN_POINT('',(1.34329598298651,97.,18.9461476330332));
#45468=CARTESIAN_POINT('',(1.34329598298651,97.,18.9461476330332));
#45469=CARTESIAN_POINT('',(-4.65835823559196,97.,18.2849312538381));
#45470=CARTESIAN_POINT('',(-4.65835823559196,97.,18.2849312538381));
#45471=CARTESIAN_POINT('',(-4.65835823559196,97.,18.2849312538381));
#45472=CARTESIAN_POINT('Origin',(3.25260651745652E-16,57.,24.));
#45473=CARTESIAN_POINT('',(-25.920440199119,57.,14.9044744769683));
#45474=CARTESIAN_POINT('',(-17.9705006596957,57.,6.16936836636249));
#45475=CARTESIAN_POINT('',(-8.48324341658624,57.,22.4875767898433));
#45476=CARTESIAN_POINT('',(-4.19913133791449,57.,27.5520833333334));
#45477=CARTESIAN_POINT('',(-12.6082977750152,57.,27.0200373644439));
#45478=CARTESIAN_POINT('',(-4.65835823559196,57.,18.2849312538381));
#45479=CARTESIAN_POINT('',(-25.920440199119,57.,14.9044744769683));
#45480=CARTESIAN_POINT('Origin',(-4.19913133791449,57.,27.5520833333334));
#45481=CARTESIAN_POINT('',(-8.48324341658624,61.,22.4875767898433));
#45482=CARTESIAN_POINT('',(-4.19913133791449,61.,27.5520833333334));
#45483=CARTESIAN_POINT('',(-8.48324341658624,57.,22.4875767898433));
#45484=CARTESIAN_POINT('Origin',(-25.920440199119,57.,14.9044744769683));
#45485=CARTESIAN_POINT('',(-12.6082977750152,57.,27.0200373644439));
#45486=CARTESIAN_POINT('',(-38.4791603945101,72.5536664749007,28.7035421272497));
#45487=CARTESIAN_POINT('',(-25.920440199119,57.,14.9044744769683));
#45488=CARTESIAN_POINT('Origin',(6.55415551239188,61.,5.96502657159819));
#45489=CARTESIAN_POINT('',(-19.7919116169754,72.2126703843529,34.9131325076166));
#45490=CARTESIAN_POINT('',(-23.0761541002795,76.2801240271818,38.5217393960537));
#45491=CARTESIAN_POINT('',(-5.392814762146,61.,19.0919255286074));
#45492=CARTESIAN_POINT('',(-4.75813954748794,97.,18.3945673514392));
#45493=CARTESIAN_POINT('',(-4.65835823559196,97.,18.2849312538381));
#45494=CARTESIAN_POINT('',(-6.2344942021657,97.,20.0167324637077));
#45495=CARTESIAN_POINT('',(-4.65835823559196,97.,18.2849312538381));
#45496=CARTESIAN_POINT('',(-19.7919116169754,72.2126703843529,34.9131325076166));
#45497=CARTESIAN_POINT('Origin',(-33.1040540410792,72.2126703843529,22.797569620141));
#45498=CARTESIAN_POINT('',(-12.7886497145576,97.,14.0517058921096));
#45499=CARTESIAN_POINT('',(-19.5466366262695,97.,7.90116957623214));
#45500=CARTESIAN_POINT('',(-19.5466366262695,97.,7.90116957623214));
#45501=CARTESIAN_POINT('',(-19.5466366262695,97.,7.90116957623214));
#45502=CARTESIAN_POINT('',(-33.1040540410792,72.2126703843529,22.797569620141));
#45503=CARTESIAN_POINT('',(-33.1040540410792,72.2126703843529,22.797569620141));
#45504=CARTESIAN_POINT('',(-33.1040540410792,72.2126703843529,22.797569620141));
#45505=CARTESIAN_POINT('Origin',(-17.9705006596957,97.,6.16936836636249));
#45506=CARTESIAN_POINT('Origin',(0.,97.,6.93889390390723E-15));
#45507=CARTESIAN_POINT('Origin',(13.6156503256296,104.8,21.7396887260909));
#45508=CARTESIAN_POINT('',(-3.34832134744457,97.,18.7026400316706));
#45509=CARTESIAN_POINT('',(13.6156503256296,97.,21.7396887260909));
#45510=CARTESIAN_POINT('',(13.6156503256296,97.,21.7396887260909));
#45511=CARTESIAN_POINT('',(13.6156503256296,104.8,21.7396887260909));
#45512=CARTESIAN_POINT('',(13.6156503256296,104.8,21.7396887260909));
#45513=CARTESIAN_POINT('',(-3.34832134744457,104.8,18.7026400316706));
#45514=CARTESIAN_POINT('',(13.6156503256296,104.8,21.7396887260909));
#45515=CARTESIAN_POINT('',(-3.34832134744457,104.8,18.7026400316706));
#45516=CARTESIAN_POINT('Origin',(0.,104.8,6.93889390390723E-15));
#45517=CARTESIAN_POINT('Origin',(0.,104.8,6.93889390390723E-15));
#45518=CARTESIAN_POINT('',(21.7396887282687,104.8,13.6156503221525));
#45519=CARTESIAN_POINT('Origin',(14.8492424010046,104.8,14.8492423986296));
#45520=CARTESIAN_POINT('',(18.7026400311351,104.8,-3.34832135043594));
#45521=CARTESIAN_POINT('',(21.7396887282687,104.8,13.6156503221525));
#45522=CARTESIAN_POINT('Origin',(0.,104.8,6.93889390390723E-15));
#45523=CARTESIAN_POINT('Origin',(0.,104.8,6.93889390390723E-15));
#45524=CARTESIAN_POINT('',(18.7026400311351,97.,-3.34832135043594));
#45525=CARTESIAN_POINT('Origin',(0.,97.,6.93889390390723E-15));
#45526=CARTESIAN_POINT('Origin',(0.,97.,6.93889390390723E-15));
#45527=CARTESIAN_POINT('',(18.7026400311351,104.8,-3.34832135043594));
#45528=CARTESIAN_POINT('Origin',(0.,97.,0.));
#45529=CARTESIAN_POINT('',(18.9542370742857,97.,-1.94298164780184));
#45530=CARTESIAN_POINT('',(21.7396887282687,97.,13.6156503221525));
#45531=CARTESIAN_POINT('',(18.9542370742857,97.,3.8));
#45532=CARTESIAN_POINT('Origin',(3.25260651745652E-16,61.,24.));
#45533=CARTESIAN_POINT('',(-17.9705006596957,61.,6.16936836636249));
#45534=CARTESIAN_POINT('',(-18.7049571862498,61.,6.97636264113177));
#45535=CARTESIAN_POINT('',(-17.9705006596957,61.,6.16936836636249));
#45536=CARTESIAN_POINT('',(18.9542370742857,61.,3.8));
#45537=CARTESIAN_POINT('',(18.9542370742857,61.,3.8));
#45538=CARTESIAN_POINT('',(18.9542370742857,61.,3.8));
#45539=CARTESIAN_POINT('Origin',(18.9542370742857,97.,3.8));
#45540=CARTESIAN_POINT('',(18.9542370742857,97.,3.8));
#45541=CARTESIAN_POINT('',(18.9542370742857,97.,3.8));
#45542=CARTESIAN_POINT('',(18.9542370742857,97.,3.8));
#45543=CARTESIAN_POINT('Origin',(18.9542370742857,97.,3.8));
#45544=CARTESIAN_POINT('',(18.9542370742857,97.,3.8));
#45545=CARTESIAN_POINT('Origin',(0.,97.,6.93889390390723E-15));
#45546=CARTESIAN_POINT('',(21.7396887282687,97.,13.6156503221525));
#45547=CARTESIAN_POINT('',(21.7396887282687,97.,13.6156503221525));
#45548=CARTESIAN_POINT('Origin',(14.8492424010046,97.,14.8492423986296));
#45549=CARTESIAN_POINT('Origin',(0.,97.,6.93889390390723E-15));
#45550=CARTESIAN_POINT('Origin',(21.7396887282687,104.8,13.6156503221525));
#45551=CARTESIAN_POINT('',(21.7396887282687,104.8,13.6156503221525));
#45552=CARTESIAN_POINT('Origin',(14.8492424010046,104.8,14.8492423986296));
#45553=CARTESIAN_POINT('Origin',(-36.3882965243833,76.2801240271818,26.4061765085781));
#45554=CARTESIAN_POINT('',(-36.3882965243834,76.2801240271818,26.4061765085781));
#45555=CARTESIAN_POINT('',(-36.3882965243833,76.2801240271818,26.4061765085781));
#45556=CARTESIAN_POINT('Origin',(-38.4791603945101,72.5536664749007,28.7035421272497));
#45557=CARTESIAN_POINT('Origin',(0.,97.,6.93889390390723E-15));
#45558=CARTESIAN_POINT('',(-17.9705006596957,97.,6.16936836636249));
#45559=CARTESIAN_POINT('',(-17.9705006596957,97.,6.16936836636249));
#45560=CARTESIAN_POINT('Origin',(0.,97.,6.93889390390723E-15));
#45561=CARTESIAN_POINT('Origin',(-17.9705006596957,97.,6.16936836636249));
#45562=CARTESIAN_POINT('',(-17.9705006596957,97.,6.16936836636249));
#45563=CARTESIAN_POINT('Origin',(-6.75798691171192,61.,-6.15053631587742));
#45564=CARTESIAN_POINT('',(-17.9705006596957,97.,6.16936836636249));
#45565=CARTESIAN_POINT('Origin',(-17.9705006596957,97.,6.16936836636249));
#45566=CARTESIAN_POINT('Origin',(0.,97.,6.93889390390723E-15));
#45567=CARTESIAN_POINT('Origin',(0.,104.8,6.93889390390723E-15));
#45568=CARTESIAN_POINT('',(0.,0.,0.));
#45569=CARTESIAN_POINT('Origin',(6.61325378140121E-15,20.,8.67361737988404E-16));
#45570=CARTESIAN_POINT('',(-16.4311231709604,20.4751899333702,3.97184757758869));
#45571=CARTESIAN_POINT('',(-16.2371390735994,19.8911995661135,3.31402377493683));
#45572=CARTESIAN_POINT('Ctrl Pts',(-16.2371391035607,19.8912002375752,3.31402203697616));
#45573=CARTESIAN_POINT('Ctrl Pts',(-16.2259081885633,19.9279846491836,3.32803992581055));
#45574=CARTESIAN_POINT('Ctrl Pts',(-16.21610893629,19.9659892577548,3.35699075210906));
#45575=CARTESIAN_POINT('Ctrl Pts',(-16.2047647575198,20.0287863583858,3.41123974011251));
#45576=CARTESIAN_POINT('Ctrl Pts',(-16.2015113087813,20.0572758839873,3.43881950477961));
#45577=CARTESIAN_POINT('Ctrl Pts',(-16.1982197044851,20.1365633601703,3.5193334688907));
#45578=CARTESIAN_POINT('Ctrl Pts',(-16.2034921724796,20.187761246405,3.5761654848116));
#45579=CARTESIAN_POINT('Ctrl Pts',(-16.2318237402137,20.2873087487659,3.69280893423355));
#45580=CARTESIAN_POINT('Ctrl Pts',(-16.2566681168736,20.3365098327336,3.75433106955588));
#45581=CARTESIAN_POINT('Ctrl Pts',(-16.3283879292358,20.4193612299745,3.86971862334388));
#45582=CARTESIAN_POINT('Ctrl Pts',(-16.374261882323,20.45337712185,3.92346367802565));
#45583=CARTESIAN_POINT('Ctrl Pts',(-16.4311231758819,20.4751899320956,3.97184757096493));
#45584=CARTESIAN_POINT('',(-16.6268429955203,20.5,3.81948640102502));
#45585=CARTESIAN_POINT('Origin',(-16.6034196622342,20.0095539027816,3.82038660784234));
#45586=CARTESIAN_POINT('',(-17.0305720504421,20.5,1.));
#45587=CARTESIAN_POINT('Origin',(6.61325378140121E-15,20.5,8.67361737988404E-16));
#45588=CARTESIAN_POINT('',(-16.5314317768924,20.,0.970691514526271));
#45589=CARTESIAN_POINT('Origin',(-17.0305720504421,20.,1.));
#45590=CARTESIAN_POINT('',(-16.5433923268431,19.8911992509365,0.971393813304911));
#45591=CARTESIAN_POINT('Origin',(-17.0305720504421,20.,1.));
#45592=CARTESIAN_POINT('Origin',(6.61325378140121E-15,19.8911992509365,
8.67361737988404E-16));
#45593=CARTESIAN_POINT('Origin',(0.,12.,0.));
#45594=CARTESIAN_POINT('',(2.38806125833734E-15,8.00000000000001,19.5));
#45595=CARTESIAN_POINT('Origin',(4.8984254152895E-16,8.,1.70652395450943E-16));
#45596=CARTESIAN_POINT('',(2.38806125833734E-15,0.999999999999994,19.5));
#45597=CARTESIAN_POINT('',(2.38806125833734E-15,12.,19.5));
#45598=CARTESIAN_POINT('Origin',(6.12303176911187E-17,1.,3.29879455650267E-15));
#45599=CARTESIAN_POINT('Origin',(-6.,21.,7.));
#45600=CARTESIAN_POINT('',(-16.0233918507227,23.8433850776541,7.00000000000931));
#45601=CARTESIAN_POINT('',(-17.1604382595081,21.8496676031881,4.3051562348531));
#45602=CARTESIAN_POINT('Ctrl Pts',(-16.0233918597094,23.8433856528354,7.00000000001199));
#45603=CARTESIAN_POINT('Ctrl Pts',(-16.0284377251753,23.8433069425452,6.99144636015799));
#45604=CARTESIAN_POINT('Ctrl Pts',(-16.0334726453492,23.843189782176,6.98288622959523));
#45605=CARTESIAN_POINT('Ctrl Pts',(-16.0384965994218,23.843033968243,6.97431959907794));
#45606=CARTESIAN_POINT('Ctrl Pts',(-16.067918697475,23.8421214653128,6.92415030226116));
#45607=CARTESIAN_POINT('Ctrl Pts',(-16.0969646771329,23.8398833271083,6.87375808053725));
#45608=CARTESIAN_POINT('Ctrl Pts',(-16.1256302786017,23.8362782231697,6.82314031829582));
#45609=CARTESIAN_POINT('Ctrl Pts',(-16.1442199635033,23.8339403079396,6.79031462470237));
#45610=CARTESIAN_POINT('Ctrl Pts',(-16.1626496774753,23.8310276912692,6.75739407907483));
#45611=CARTESIAN_POINT('Ctrl Pts',(-16.1809181459987,23.8275229657671,6.72437791675892));
#45612=CARTESIAN_POINT('Ctrl Pts',(-16.2041375205119,23.8230684306814,6.68241410152068));
#45613=CARTESIAN_POINT('Ctrl Pts',(-16.2270964121805,23.8176574074361,6.6402960321563));
#45614=CARTESIAN_POINT('Ctrl Pts',(-16.2497921838513,23.8112536349832,6.59802202944585));
#45615=CARTESIAN_POINT('Ctrl Pts',(-16.2561057824771,23.809472208489,6.58626208185338));
#45616=CARTESIAN_POINT('Ctrl Pts',(-16.2623990192776,23.8076139509515,6.57449005186631));
#45617=CARTESIAN_POINT('Ctrl Pts',(-16.2686718368427,23.8056780738639,6.5627059101453));
#45618=CARTESIAN_POINT('Ctrl Pts',(-16.2736736063734,23.8041344595419,6.55330956466016));
#45619=CARTESIAN_POINT('Ctrl Pts',(-16.2786623917353,23.8025413849404,6.54390551776014));
#45620=CARTESIAN_POINT('Ctrl Pts',(-16.2836381623927,23.8008983485357,6.53449375383592));
#45621=CARTESIAN_POINT('Ctrl Pts',(-16.2901995856383,23.7987317178766,6.52208269817312));
#45622=CARTESIAN_POINT('Ctrl Pts',(-16.2967376415088,23.7964784648201,6.50965962858277));
#45623=CARTESIAN_POINT('Ctrl Pts',(-16.3032535167685,23.7941370090411,6.49722211474457));
#45624=CARTESIAN_POINT('Ctrl Pts',(-16.3078757650997,23.7924760211254,6.48839915922591));
#45625=CARTESIAN_POINT('Ctrl Pts',(-16.3124894944245,23.7907696002991,6.47956383625479));
#45626=CARTESIAN_POINT('Ctrl Pts',(-16.3170869282503,23.7890203161444,6.47073105701516));
#45627=CARTESIAN_POINT('Ctrl Pts',(-16.318180251042,23.7886043161957,6.46863052023255));
#45628=CARTESIAN_POINT('Ctrl Pts',(-16.3192726250444,23.7881859023917,6.46653017992206));
#45629=CARTESIAN_POINT('Ctrl Pts',(-16.320363939594,23.7877651117504,6.46443024841133));
#45630=CARTESIAN_POINT('Ctrl Pts',(-16.3260389472779,23.7855769340861,6.45351027354005));
#45631=CARTESIAN_POINT('Ctrl Pts',(-16.3316845634806,23.7833249057076,6.44260286155155));
#45632=CARTESIAN_POINT('Ctrl Pts',(-16.3373010110403,23.7810090011584,6.43170801330259));
#45633=CARTESIAN_POINT('Ctrl Pts',(-16.3597169306986,23.7717659467615,6.38822535982041));
#45634=CARTESIAN_POINT('Ctrl Pts',(-16.3816683400294,23.7615059125948,6.34494266243544));
#45635=CARTESIAN_POINT('Ctrl Pts',(-16.4031683995334,23.7502232140424,6.30186134796477));
#45636=CARTESIAN_POINT('Ctrl Pts',(-16.4172323732936,23.7428427890555,6.27368028752822));
#45637=CARTESIAN_POINT('Ctrl Pts',(-16.4311033535401,23.7350253864853,6.24558518657362));
#45638=CARTESIAN_POINT('Ctrl Pts',(-16.4447844323403,23.7267668059867,6.21757733753011));
#45639=CARTESIAN_POINT('Ctrl Pts',(-16.4727067748196,23.7099114894986,6.1604148312306));
#45640=CARTESIAN_POINT('Ctrl Pts',(-16.4998355812374,23.6912200670357,6.10362158299839));
#45641=CARTESIAN_POINT('Ctrl Pts',(-16.5261925108193,23.6706610942453,6.04721999865201));
#45642=CARTESIAN_POINT('Ctrl Pts',(-16.5383895772972,23.6611471196732,6.02111931527783));
#45643=CARTESIAN_POINT('Ctrl Pts',(-16.5504213408844,23.6512332657452,5.99510248283814));
#45644=CARTESIAN_POINT('Ctrl Pts',(-16.5622894775869,23.6409135376314,5.96917275294547));
#45645=CARTESIAN_POINT('Ctrl Pts',(-16.5883707008436,23.6182350717835,5.91219000230245));
#45646=CARTESIAN_POINT('Ctrl Pts',(-16.613662202772,23.593596548317,5.85562799479922));
#45647=CARTESIAN_POINT('Ctrl Pts',(-16.6381830439851,23.5669338767108,5.79952074742108));
#45648=CARTESIAN_POINT('Ctrl Pts',(-16.6489320806676,23.5552459402058,5.77492538974222));
#45649=CARTESIAN_POINT('Ctrl Pts',(-16.6595330305966,23.543169167367,5.75041737025986));
#45650=CARTESIAN_POINT('Ctrl Pts',(-16.6699871278393,23.5306950852284,5.72600068773709));
#45651=CARTESIAN_POINT('Ctrl Pts',(-16.687138187239,23.510230025573,5.68594252082273));
#45652=CARTESIAN_POINT('Ctrl Pts',(-16.7038942239911,23.4886956751937,5.64613036475662));
#45653=CARTESIAN_POINT('Ctrl Pts',(-16.7202610350444,23.4660543595333,5.60658198567009));
#45654=CARTESIAN_POINT('Ctrl Pts',(-16.7268161206599,23.4569862666644,5.59074243024164));
#45655=CARTESIAN_POINT('Ctrl Pts',(-16.7333087571338,23.4477405918434,5.57494516833557));
#45656=CARTESIAN_POINT('Ctrl Pts',(-16.7397393243964,23.4383148767634,5.55919131448836));
#45657=CARTESIAN_POINT('Ctrl Pts',(-16.7413367132527,23.4359734764459,5.55527796912543));
#45658=CARTESIAN_POINT('Ctrl Pts',(-16.7429302691987,23.433620942759,5.55136731108168));
#45659=CARTESIAN_POINT('Ctrl Pts',(-16.7445199969512,23.4312572278318,5.54745936122601));
#45660=CARTESIAN_POINT('Ctrl Pts',(-16.7485147239046,23.425317597153,5.53763931965202));
#45661=CARTESIAN_POINT('Ctrl Pts',(-16.7524852872413,23.4193073729298,5.52783639310678));
#45662=CARTESIAN_POINT('Ctrl Pts',(-16.7564317657962,23.4132257989771,5.51805092053644));
#45663=CARTESIAN_POINT('Ctrl Pts',(-16.7588161175821,23.4095514823646,5.51213881214064));
#45664=CARTESIAN_POINT('Ctrl Pts',(-16.7611918475176,23.4058508582643,5.50623265323961));
#45665=CARTESIAN_POINT('Ctrl Pts',(-16.7635588441968,23.4021239495519,5.50033283496077));
#45666=CARTESIAN_POINT('Ctrl Pts',(-16.7651096006317,23.3996822360849,5.49646752275275));
#45667=CARTESIAN_POINT('Ctrl Pts',(-16.7666564028141,23.3972295317442,5.49260543324729));
#45668=CARTESIAN_POINT('Ctrl Pts',(-16.7681985799081,23.3947669372142,5.48874830563239));
#45669=CARTESIAN_POINT('Ctrl Pts',(-16.7705519340973,23.3910090308258,5.48286234904143));
#45670=CARTESIAN_POINT('Ctrl Pts',(-16.7728944619133,23.3872281839827,5.47698808791221));
#45671=CARTESIAN_POINT('Ctrl Pts',(-16.7752239052603,23.3834281185936,5.47113139231683));
#45672=CARTESIAN_POINT('Ctrl Pts',(-16.7790773875821,23.3771418593388,5.46144295195627));
#45673=CARTESIAN_POINT('Ctrl Pts',(-16.7828979733183,23.3707984623358,5.45179534097987));
#45674=CARTESIAN_POINT('Ctrl Pts',(-16.7866861214173,23.3643980243537,5.44218853694711));
#45675=CARTESIAN_POINT('Ctrl Pts',(-16.8018147227821,23.338836807564,5.40382216245424));
#45676=CARTESIAN_POINT('Ctrl Pts',(-16.8164262027409,23.3123662713952,5.36610626913502));
#45677=CARTESIAN_POINT('Ctrl Pts',(-16.8305477690303,23.2849889629749,5.3290423500846));
#45678=CARTESIAN_POINT('Ctrl Pts',(-16.8390627181896,23.2684811348389,5.3066937394637));
#45679=CARTESIAN_POINT('Ctrl Pts',(-16.8473998107328,23.2516441263546,5.28458176432105));
#45680=CARTESIAN_POINT('Ctrl Pts',(-16.8555640341602,23.2344766403772,5.26270826111354));
#45681=CARTESIAN_POINT('Ctrl Pts',(-16.8743784114623,23.1949143278836,5.21230097548252));
#45682=CARTESIAN_POINT('Ctrl Pts',(-16.8922740093455,23.1536002626368,5.16316463641716));
#45683=CARTESIAN_POINT('Ctrl Pts',(-16.9093101088097,23.1105258117712,5.11532790787435));
#45684=CARTESIAN_POINT('Ctrl Pts',(-16.916852396087,23.091455725721,5.09414944799066));
#45685=CARTESIAN_POINT('Ctrl Pts',(-16.9242262045456,23.0720406582638,5.0732256601497));
#45686=CARTESIAN_POINT('Ctrl Pts',(-16.9314355358393,23.0522772513815,5.05256120178904));
#45687=CARTESIAN_POINT('Ctrl Pts',(-16.9474705650594,23.0083193870615,5.00659921445182));
#45688=CARTESIAN_POINT('Ctrl Pts',(-16.9626931835324,22.9626383608009,4.96192034827594));
#45689=CARTESIAN_POINT('Ctrl Pts',(-16.977149247726,22.9151967856811,4.91857454139849));
#45690=CARTESIAN_POINT('Ctrl Pts',(-16.9838731661397,22.8931303866773,4.89841319837217));
#45691=CARTESIAN_POINT('Ctrl Pts',(-16.99043100828,22.8706825154872,4.8785407471639));
#45692=CARTESIAN_POINT('Ctrl Pts',(-16.9968265198859,22.8478469378767,4.85896430688065));
#45693=CARTESIAN_POINT('Ctrl Pts',(-17.0003660793906,22.8352087173936,4.84812983740528));
#45694=CARTESIAN_POINT('Ctrl Pts',(-17.0038557015822,22.8224526137342,4.83738677511585));
#45695=CARTESIAN_POINT('Ctrl Pts',(-17.0072962876948,22.809576737179,4.82673558374586));
#45696=CARTESIAN_POINT('Ctrl Pts',(-17.0121178529662,22.7915327536236,4.81180922738465));
#45697=CARTESIAN_POINT('Ctrl Pts',(-17.0168430837008,22.7732534583247,4.79706337239252));
#45698=CARTESIAN_POINT('Ctrl Pts',(-17.021474163257,22.7547327835074,4.78250002849357));
#45699=CARTESIAN_POINT('Ctrl Pts',(-17.0229427117219,22.748859744998,4.77788188793504));
#45700=CARTESIAN_POINT('Ctrl Pts',(-17.0244024446751,22.7429597062764,4.77328002892413));
#45701=CARTESIAN_POINT('Ctrl Pts',(-17.0258519078165,22.7370387750722,4.76869934923281));
#45702=CARTESIAN_POINT('Ctrl Pts',(-17.0266859568084,22.7336317572868,4.76606353796613));
#45703=CARTESIAN_POINT('Ctrl Pts',(-17.0275165314831,22.7302181246644,4.76343497366233));
#45704=CARTESIAN_POINT('Ctrl Pts',(-17.0283433567152,22.726799039008,4.7608145820925));
#45705=CARTESIAN_POINT('Ctrl Pts',(-17.0306064360811,22.7174407588067,4.75364238431455));
#45706=CARTESIAN_POINT('Ctrl Pts',(-17.0328406947071,22.7080449324597,4.74653378214495));
#45707=CARTESIAN_POINT('Ctrl Pts',(-17.035046758628,22.6986113109312,4.73948821377146));
#45708=CARTESIAN_POINT('Ctrl Pts',(-17.0365196257533,22.6923130024866,4.73478427661965));
#45709=CARTESIAN_POINT('Ctrl Pts',(-17.0379799702854,22.6859978859778,4.73010837023522));
#45710=CARTESIAN_POINT('Ctrl Pts',(-17.039427949088,22.6796658611914,4.72546037207139));
#45711=CARTESIAN_POINT('Ctrl Pts',(-17.043837088838,22.6603846520101,4.71130707547284));
#45712=CARTESIAN_POINT('Ctrl Pts',(-17.0481310680966,22.640947326536,4.69741303542798));
#45713=CARTESIAN_POINT('Ctrl Pts',(-17.0523146503055,22.6213547488622,4.68377752410598));
#45714=CARTESIAN_POINT('Ctrl Pts',(-17.0631983357952,22.570384206709,4.648304427294));
#45715=CARTESIAN_POINT('Ctrl Pts',(-17.0733323397321,22.5183633805738,4.61458142439873));
#45716=CARTESIAN_POINT('Ctrl Pts',(-17.0827819382676,22.4653091749687,4.58259528972156));
#45717=CARTESIAN_POINT('Ctrl Pts',(-17.0878616725955,22.4367893105069,4.56540079561412));
#45718=CARTESIAN_POINT('Ctrl Pts',(-17.0927435475338,22.4079708208665,4.54870821341221));
#45719=CARTESIAN_POINT('Ctrl Pts',(-17.0974346071329,22.3788534273067,4.53252048432898));
#45720=CARTESIAN_POINT('Ctrl Pts',(-17.1058978315018,22.3263222177721,4.50331591330117));
#45721=CARTESIAN_POINT('Ctrl Pts',(-17.1137418031168,22.2728181444527,4.47575463281059));
#45722=CARTESIAN_POINT('Ctrl Pts',(-17.1210087870872,22.2183386823111,4.44985278433895));
#45723=CARTESIAN_POINT('Ctrl Pts',(-17.125262903816,22.1864462229058,4.43468975558594));
#45724=CARTESIAN_POINT('Ctrl Pts',(-17.1293192739918,22.154219575904,4.42009527073905));
#45725=CARTESIAN_POINT('Ctrl Pts',(-17.1331830538353,22.1216546244272,4.40607883828957));
#45726=CARTESIAN_POINT('Ctrl Pts',(-17.1384150443394,22.0775580340953,4.38709901944727));
#45727=CARTESIAN_POINT('Ctrl Pts',(-17.1432952592276,22.0328413580963,4.36917924964466));
#45728=CARTESIAN_POINT('Ctrl Pts',(-17.1478360657817,21.9874939088656,4.35234281173029));
#45729=CARTESIAN_POINT('Ctrl Pts',(-17.1488284826203,21.9775829884882,4.34866312084493));
#45730=CARTESIAN_POINT('Ctrl Pts',(-17.1498047181489,21.9676413186292,4.34503494964224));
#45731=CARTESIAN_POINT('Ctrl Pts',(-17.1507648504972,21.9576696303041,4.34145885652359));
#45732=CARTESIAN_POINT('Ctrl Pts',(-17.1518385084627,21.946518894034,4.3374599277622));
#45733=CARTESIAN_POINT('Ctrl Pts',(-17.1528919489068,21.9353305256573,4.33352628632849));
#45734=CARTESIAN_POINT('Ctrl Pts',(-17.1539252278949,21.924105493081,4.32965880561775));
#45735=CARTESIAN_POINT('Ctrl Pts',(-17.1540818609778,21.9224039086308,4.32907254050056));
#45736=CARTESIAN_POINT('Ctrl Pts',(-17.1542380525564,21.9207012217312,4.32848771335121));
#45737=CARTESIAN_POINT('Ctrl Pts',(-17.1543937822607,21.9189976751517,4.32790440467035));
#45738=CARTESIAN_POINT('Ctrl Pts',(-17.1552641853424,21.9094762277235,4.32464418096637));
#45739=CARTESIAN_POINT('Ctrl Pts',(-17.1561212020475,21.8999164524419,4.32142744214349));
#45740=CARTESIAN_POINT('Ctrl Pts',(-17.1569616836063,21.8903543830217,4.31826660511824));
#45741=CARTESIAN_POINT('Ctrl Pts',(-17.1571359480896,21.8883717945047,4.31761124079123));
#45742=CARTESIAN_POINT('Ctrl Pts',(-17.1573095927471,21.8863881041705,4.31695793879396));
#45743=CARTESIAN_POINT('Ctrl Pts',(-17.1574826225619,21.8844032604135,4.31630668534007));
#45744=CARTESIAN_POINT('Ctrl Pts',(-17.1584901791008,21.8728454701626,4.31251442169526));
#45745=CARTESIAN_POINT('Ctrl Pts',(-17.1594752876153,21.8612669031643,4.30879763630566));
#45746=CARTESIAN_POINT('Ctrl Pts',(-17.1604382596112,21.8496676051728,4.30515622855862));
#45747=CARTESIAN_POINT('',(-28.4921884534998,21.8412135273285,4.48858057664302));
#45748=CARTESIAN_POINT('Ctrl Pts',(-17.1604382594737,21.8496676025262,4.30515623695262));
#45749=CARTESIAN_POINT('Ctrl Pts',(-20.937690036586,21.8469996129353,4.36619867482251));
#45750=CARTESIAN_POINT('Ctrl Pts',(-24.7149401916638,21.8441900251035,4.42733521081778));
#45751=CARTESIAN_POINT('Ctrl Pts',(-28.4921884534998,21.8412135273285,4.48858057664302));
#45752=CARTESIAN_POINT('',(-28.492188453501,20.1587864726715,4.48858057664304));
#45753=CARTESIAN_POINT('Ctrl Pts',(-28.4921884534998,21.8412135273285,4.48858057664302));
#45754=CARTESIAN_POINT('Ctrl Pts',(-28.5227165270159,21.8411894664569,4.48907556589413));
#45755=CARTESIAN_POINT('Ctrl Pts',(-28.5530697764421,21.839992183168,4.4891736621749));
#45756=CARTESIAN_POINT('Ctrl Pts',(-28.5832520807999,21.8376467249157,4.48888855370485));
#45757=CARTESIAN_POINT('Ctrl Pts',(-28.5858424780989,21.8374454258814,4.48886408426071));
#45758=CARTESIAN_POINT('Ctrl Pts',(-28.5884316135345,21.8372356594637,4.48883678885867));
#45759=CARTESIAN_POINT('Ctrl Pts',(-28.5910194901533,21.8370174426294,4.4888066765942));
#45760=CARTESIAN_POINT('Ctrl Pts',(-28.6185845479042,21.8346930815706,4.48848593243537));
#45761=CARTESIAN_POINT('Ctrl Pts',(-28.6460068811572,21.8314097542959,4.48784553144024));
#45762=CARTESIAN_POINT('Ctrl Pts',(-28.6732861919453,21.8271634702414,4.48689681709569));
#45763=CARTESIAN_POINT('Ctrl Pts',(-28.6782462125312,21.8263913958848,4.48672431850452));
#45764=CARTESIAN_POINT('Ctrl Pts',(-28.6832014941128,21.8255874235304,4.48654160704114));
#45765=CARTESIAN_POINT('Ctrl Pts',(-28.6881520409208,21.8247515308658,4.48634875274379));
#45766=CARTESIAN_POINT('Ctrl Pts',(-28.7129848589572,21.8205585454759,4.485381361492));
#45767=CARTESIAN_POINT('Ctrl Pts',(-28.7376985199429,21.8155624946819,4.48415871300685));
#45768=CARTESIAN_POINT('Ctrl Pts',(-28.7622902462614,21.8097419383589,4.48269023678948));
#45769=CARTESIAN_POINT('Ctrl Pts',(-28.7694071606622,21.8080574530739,4.48226525566358));
#45770=CARTESIAN_POINT('Ctrl Pts',(-28.7765112054826,21.8063044074594,4.48181980291049));
#45771=CARTESIAN_POINT('Ctrl Pts',(-28.7836050970554,21.8044816528127,4.48135395516118));
#45772=CARTESIAN_POINT('Ctrl Pts',(-28.7912106045476,21.8025274399551,4.48085451017937));
#45773=CARTESIAN_POINT('Ctrl Pts',(-28.7988145600856,21.8004896679887,4.48033076967421));
#45774=CARTESIAN_POINT('Ctrl Pts',(-28.8063988576059,21.7983729620984,4.4797845327618));
#45775=CARTESIAN_POINT('Ctrl Pts',(-28.8137280605548,21.7963274506966,4.47925666829203));
#45776=CARTESIAN_POINT('Ctrl Pts',(-28.8210440935422,21.794206699072,4.47870739914648));
#45777=CARTESIAN_POINT('Ctrl Pts',(-28.8283192684753,21.7920178352031,4.47813911019099));
#45778=CARTESIAN_POINT('Ctrl Pts',(-28.8290919422524,21.7917853627569,4.47807875398269));
#45779=CARTESIAN_POINT('Ctrl Pts',(-28.829864237367,21.7915520981649,4.47801817707474));
#45780=CARTESIAN_POINT('Ctrl Pts',(-28.8306361287375,21.7913180475491,4.47795738170932));
#45781=CARTESIAN_POINT('Ctrl Pts',(-28.8371320454856,21.7893483749078,4.47744575319842));
#45782=CARTESIAN_POINT('Ctrl Pts',(-28.8436017105944,21.7873228425933,4.47691861764328));
#45783=CARTESIAN_POINT('Ctrl Pts',(-28.8500445700105,21.7852417342137,4.47637649647148));
#45784=CARTESIAN_POINT('Ctrl Pts',(-28.8589452391665,21.782366728573,4.47562756794751));
#45785=CARTESIAN_POINT('Ctrl Pts',(-28.867795030091,21.7793853473532,4.47484994645555));
#45786=CARTESIAN_POINT('Ctrl Pts',(-28.8765942156564,21.7762977216211,4.47404486510076));
#45787=CARTESIAN_POINT('Ctrl Pts',(-28.8963000577746,21.769382960619,4.47224187936397));
#45788=CARTESIAN_POINT('Ctrl Pts',(-28.9157526841421,21.761936297264,4.47030119654534));
#45789=CARTESIAN_POINT('Ctrl Pts',(-28.9349503511768,21.7539513728655,4.46823635605871));
#45790=CARTESIAN_POINT('Ctrl Pts',(-28.9450156597226,21.7497648887661,4.46715376323334));
#45791=CARTESIAN_POINT('Ctrl Pts',(-28.9550106747551,21.7454301254848,4.46603695502191));
#45792=CARTESIAN_POINT('Ctrl Pts',(-28.964935373711,21.740946115794,4.46488795892171));
#45793=CARTESIAN_POINT('Ctrl Pts',(-28.9823926751867,21.7330588529822,4.46286690302823));
#45794=CARTESIAN_POINT('Ctrl Pts',(-28.999632408897,21.7247098510798,4.46074616568145));
#45795=CARTESIAN_POINT('Ctrl Pts',(-29.0166492430745,21.7158853181679,4.45853674003619));
#45796=CARTESIAN_POINT('Ctrl Pts',(-29.0273929158853,21.7103139002811,4.45714180687854));
#45797=CARTESIAN_POINT('Ctrl Pts',(-29.0380469194319,21.7045529828368,4.45571153450151));
#45798=CARTESIAN_POINT('Ctrl Pts',(-29.0486108330097,21.6985982905204,4.45424862705299));
#45799=CARTESIAN_POINT('Ctrl Pts',(-29.0621240238921,21.6909811424507,4.45237729902201));
#45800=CARTESIAN_POINT('Ctrl Pts',(-29.0754894651515,21.6830463951951,4.45045254736087));
#45801=CARTESIAN_POINT('Ctrl Pts',(-29.088703716323,21.6747809730397,4.44848022524981));
#45802=CARTESIAN_POINT('Ctrl Pts',(-29.0908231994901,21.6734552510672,4.44816387712988));
#45803=CARTESIAN_POINT('Ctrl Pts',(-29.0929392811997,21.6721206654223,4.44784622555517));
#45804=CARTESIAN_POINT('Ctrl Pts',(-29.0950506645488,21.6707780193494,4.44752749694437));
#45805=CARTESIAN_POINT('Ctrl Pts',(-29.0994868545906,21.6679570095404,4.44685782192305));
#45806=CARTESIAN_POINT('Ctrl Pts',(-29.1039021069988,21.6651005315295,4.44618341803519));
#45807=CARTESIAN_POINT('Ctrl Pts',(-29.1082854328805,21.6622153371953,4.44550622678895));
#45808=CARTESIAN_POINT('Ctrl Pts',(-29.1102174113624,21.6609436696259,4.44520775048323));
#45809=CARTESIAN_POINT('Ctrl Pts',(-29.1121438952947,21.6596659942202,4.44490862929262));
#45810=CARTESIAN_POINT('Ctrl Pts',(-29.1140649936888,21.6583822331944,4.44460887284627));
#45811=CARTESIAN_POINT('Ctrl Pts',(-29.1185508902551,21.6553845631138,4.44390892097626));
#45812=CARTESIAN_POINT('Ctrl Pts',(-29.1230068386011,21.6523541042434,4.44320559705709));
#45813=CARTESIAN_POINT('Ctrl Pts',(-29.1274327932882,21.6492907567066,4.44249923281721));
#45814=CARTESIAN_POINT('Ctrl Pts',(-29.129202666098,21.6480657700323,4.44221676836596));
#45815=CARTESIAN_POINT('Ctrl Pts',(-29.1309677573007,21.6468355354338,4.44193381959285));
#45816=CARTESIAN_POINT('Ctrl Pts',(-29.1327280554723,21.6456000401895,4.44165040684993));
#45817=CARTESIAN_POINT('Ctrl Pts',(-29.1450526742288,21.6369497966643,4.43966611006221));
#45818=CARTESIAN_POINT('Ctrl Pts',(-29.157142362216,21.6280416455197,4.43765903675389));
#45819=CARTESIAN_POINT('Ctrl Pts',(-29.168996237874,21.6188730413405,4.43563686577132));
#45820=CARTESIAN_POINT('Ctrl Pts',(-29.1793869162976,21.6108361747184,4.43386430386807));
#45821=CARTESIAN_POINT('Ctrl Pts',(-29.1895954231523,21.6025984363405,4.43207994577978));
#45822=CARTESIAN_POINT('Ctrl Pts',(-29.1996207750758,21.5941571047765,4.43028895762304));
#45823=CARTESIAN_POINT('Ctrl Pts',(-29.2124696321858,21.5833383860013,4.42799356180181));
#45824=CARTESIAN_POINT('Ctrl Pts',(-29.2250176217377,21.5721852553999,4.42568718330686));
#45825=CARTESIAN_POINT('Ctrl Pts',(-29.237256114022,21.5606866723982,4.42338074627525));
#45826=CARTESIAN_POINT('Ctrl Pts',(-29.2466554289126,21.5518556170755,4.42160937383559));
#45827=CARTESIAN_POINT('Ctrl Pts',(-29.2558718272431,21.5428205251124,4.41983791271102));
#45828=CARTESIAN_POINT('Ctrl Pts',(-29.264901681043,21.53357566893,4.41807146387376));
#45829=CARTESIAN_POINT('Ctrl Pts',(-29.2768030222565,21.5213909547215,4.41574328549854));
#45830=CARTESIAN_POINT('Ctrl Pts',(-29.2883804475871,21.5088419871408,4.41342370773151));
#45831=CARTESIAN_POINT('Ctrl Pts',(-29.299617742575,21.4959091454236,4.41112518095054));
#45832=CARTESIAN_POINT('Ctrl Pts',(-29.3045585725327,21.4902228150511,4.41011456140285));
#45833=CARTESIAN_POINT('Ctrl Pts',(-29.3094337349238,21.4844622768702,4.40910802533679));
#45834=CARTESIAN_POINT('Ctrl Pts',(-29.3142416822275,21.4786255847451,4.40810663827177));
#45835=CARTESIAN_POINT('Ctrl Pts',(-29.3172794243947,21.4749378642554,4.40747394504097));
#45836=CARTESIAN_POINT('Ctrl Pts',(-29.3202907592376,21.4712191361926,4.40684320370065));
#45837=CARTESIAN_POINT('Ctrl Pts',(-29.3232747701016,21.4674695968391,4.40621481258309));
#45838=CARTESIAN_POINT('Ctrl Pts',(-29.325013664013,21.4652846010567,4.40584862574996));
#45839=CARTESIAN_POINT('Ctrl Pts',(-29.3267406732683,21.4630923936772,4.40548379116715));
#45840=CARTESIAN_POINT('Ctrl Pts',(-29.3284556614909,21.4608931100365,4.4051203821878));
#45841=CARTESIAN_POINT('Ctrl Pts',(-29.3377716134452,21.4489464269854,4.40314631580824));
#45842=CARTESIAN_POINT('Ctrl Pts',(-29.3467234992276,21.4368026456522,4.40121620315188));
#45843=CARTESIAN_POINT('Ctrl Pts',(-29.3553119242716,21.4244611435133,4.39933786704563));
#45844=CARTESIAN_POINT('Ctrl Pts',(-29.3616566833125,21.4153437725315,4.39795023311611));
#45845=CARTESIAN_POINT('Ctrl Pts',(-29.3678027743186,21.4061172031824,4.39659065710816));
#45846=CARTESIAN_POINT('Ctrl Pts',(-29.3737481428319,21.3967828893906,4.39526271743198));
#45847=CARTESIAN_POINT('Ctrl Pts',(-29.3838983743266,21.380846880442,4.39299559217406));
#45848=CARTESIAN_POINT('Ctrl Pts',(-29.3934673651695,21.3645919103031,4.39081973562068));
#45849=CARTESIAN_POINT('Ctrl Pts',(-29.4024399499354,21.3480104267181,4.38875131818053));
#45850=CARTESIAN_POINT('Ctrl Pts',(-29.4069596931346,21.3396578672694,4.38770939816504));
#45851=CARTESIAN_POINT('Ctrl Pts',(-29.4113277352643,21.331222226145,4.38669471346358));
#45852=CARTESIAN_POINT('Ctrl Pts',(-29.4155423013294,21.3227021231074,4.38570936360752));
#45853=CARTESIAN_POINT('Ctrl Pts',(-29.4245951987033,21.3044009226462,4.38359282990357));
#45854=CARTESIAN_POINT('Ctrl Pts',(-29.4329402271217,21.2857101671811,4.3816114641524));
#45855=CARTESIAN_POINT('Ctrl Pts',(-29.4405414932869,21.2666089081952,4.37978733052507));
#45856=CARTESIAN_POINT('Ctrl Pts',(-29.4433583616853,21.2595303857965,4.37911134520135));
#45857=CARTESIAN_POINT('Ctrl Pts',(-29.446072864589,21.2523953721124,4.37845695150955));
#45858=CARTESIAN_POINT('Ctrl Pts',(-29.4486830987638,21.2452026419165,4.3778253136806));
#45859=CARTESIAN_POINT('Ctrl Pts',(-29.4512342841163,21.2381726259518,4.37720796478796));
#45860=CARTESIAN_POINT('Ctrl Pts',(-29.4536856689904,21.2310874002537,4.37661236210478));
#45861=CARTESIAN_POINT('Ctrl Pts',(-29.4560347196898,21.2239455260892,4.37603966694944));
#45862=CARTESIAN_POINT('Ctrl Pts',(-29.45808264445,21.2177191722093,4.37554038586156));
#45863=CARTESIAN_POINT('Ctrl Pts',(-29.4600529077877,21.2114495063001,4.37505849678349));
#45864=CARTESIAN_POINT('Ctrl Pts',(-29.4619435946022,21.2051358286219,4.37459481009537));
#45865=CARTESIAN_POINT('Ctrl Pts',(-29.4622466982348,21.2041236574763,4.37452047461133));
#45866=CARTESIAN_POINT('Ctrl Pts',(-29.462547565049,21.2031109894319,4.37444665410515));
#45867=CARTESIAN_POINT('Ctrl Pts',(-29.4628461926641,21.2020978304696,4.37437335042911));
#45868=CARTESIAN_POINT('Ctrl Pts',(-29.4650075867848,21.1947648320685,4.37384279623265));
#45869=CARTESIAN_POINT('Ctrl Pts',(-29.4670484442119,21.1874164428921,4.37334005434292));
#45870=CARTESIAN_POINT('Ctrl Pts',(-29.4689700849412,21.1800528117656,4.37286547380907));
#45871=CARTESIAN_POINT('Ctrl Pts',(-29.4703195306758,21.1748818032293,4.37253220616575));
#45872=CARTESIAN_POINT('Ctrl Pts',(-29.4716100602321,21.1697029993436,4.37221280780103));
#45873=CARTESIAN_POINT('Ctrl Pts',(-29.4728416797525,21.164517221623,4.37190746254535));
#45874=CARTESIAN_POINT('Ctrl Pts',(-29.478625474554,21.1401643482511,4.37047353406884));
#45875=CARTESIAN_POINT('Ctrl Pts',(-29.4831166515775,21.1156432655594,4.36934845920679));
#45876=CARTESIAN_POINT('Ctrl Pts',(-29.4863141901159,21.0909577508463,4.36854519159516));
#45877=CARTESIAN_POINT('Ctrl Pts',(-29.4866678555618,21.0882273963985,4.36845634575493));
#45878=CARTESIAN_POINT('Ctrl Pts',(-29.4870056852833,21.0854950132696,4.36837143579129));
#45879=CARTESIAN_POINT('Ctrl Pts',(-29.4873276786664,21.0827605984085,4.36829047900386));
#45880=CARTESIAN_POINT('Ctrl Pts',(-29.4905367896416,21.0555083590705,4.36748363225269));
#45881=CARTESIAN_POINT('Ctrl Pts',(-29.4921729809254,21.0280543316155,4.36706935322525));
#45882=CARTESIAN_POINT('Ctrl Pts',(-29.4921883426906,21.0003922828609,4.3670654720775));
#45883=CARTESIAN_POINT('Ctrl Pts',(-29.4921883566808,21.0003670905664,4.36706546854288));
#45884=CARTESIAN_POINT('Ctrl Pts',(-29.4921883693259,21.000341898099,4.36706546534868));
#45885=CARTESIAN_POINT('Ctrl Pts',(-29.4921883806259,21.0003167054589,4.36706546249491));
#45886=CARTESIAN_POINT('Ctrl Pts',(-29.4921917825163,20.9927323980165,4.3670646033626));
#45887=CARTESIAN_POINT('Ctrl Pts',(-29.4920730566502,20.9851324156375,4.3670946013449));
#45888=CARTESIAN_POINT('Ctrl Pts',(-29.4918305391955,20.9775165461871,4.36715584865301));
#45889=CARTESIAN_POINT('Ctrl Pts',(-29.4916325392323,20.9712986767451,4.36720585315584));
#45890=CARTESIAN_POINT('Ctrl Pts',(-29.491351642387,20.9650645241479,4.36727677879092));
#45891=CARTESIAN_POINT('Ctrl Pts',(-29.4909881144146,20.9588345028022,4.36736851454079));
#45892=CARTESIAN_POINT('Ctrl Pts',(-29.4909049012731,20.9574084236909,4.36738951325482));
#45893=CARTESIAN_POINT('Ctrl Pts',(-29.4908173655457,20.955982561579,4.3674116001301));
#45894=CARTESIAN_POINT('Ctrl Pts',(-29.4907255238541,20.9545571623216,4.3674347698338));
#45895=CARTESIAN_POINT('Ctrl Pts',(-29.4903701470481,20.9490416515945,4.36752442383679));
#45896=CARTESIAN_POINT('Ctrl Pts',(-29.4899501892045,20.9435311774064,4.36763032274499));
#45897=CARTESIAN_POINT('Ctrl Pts',(-29.4894659444528,20.938027187658,4.36775233853024));
#45898=CARTESIAN_POINT('Ctrl Pts',(-29.4892783277562,20.9358947115263,4.36779961255538));
#45899=CARTESIAN_POINT('Ctrl Pts',(-29.4890809366929,20.933762242885,4.36784933719275));
#45900=CARTESIAN_POINT('Ctrl Pts',(-29.4888739485811,20.9316311318625,4.36790146339755));
#45901=CARTESIAN_POINT('Ctrl Pts',(-29.488405606424,20.9268091683002,4.36801940688222));
#45902=CARTESIAN_POINT('Ctrl Pts',(-29.4878877219468,20.9219900447715,4.36814974506808));
#45903=CARTESIAN_POINT('Ctrl Pts',(-29.4873219268749,20.9171880702865,4.36829200382837));
#45904=CARTESIAN_POINT('Ctrl Pts',(-29.4869922550241,20.9143901035059,4.36837489374934));
#45905=CARTESIAN_POINT('Ctrl Pts',(-29.4866463833471,20.911597564513,4.36846182241841));
#45906=CARTESIAN_POINT('Ctrl Pts',(-29.4862844141115,20.9088103872103,4.36855274501376));
#45907=CARTESIAN_POINT('Ctrl Pts',(-29.4830395682688,20.8838249470327,4.36936781374468));
#45908=CARTESIAN_POINT('Ctrl Pts',(-29.4785025352126,20.8592571813233,4.37050416053162));
#45909=CARTESIAN_POINT('Ctrl Pts',(-29.4727464080655,20.8350828641766,4.37193103596413));
#45910=CARTESIAN_POINT('Ctrl Pts',(-29.4715260666181,20.8299577304844,4.37223354408915));
#45911=CARTESIAN_POINT('Ctrl Pts',(-29.470250901937,20.8248502902165,4.37254912127071));
#45912=CARTESIAN_POINT('Ctrl Pts',(-29.4689212596439,20.8197603930924,4.37287749430385));
#45913=CARTESIAN_POINT('Ctrl Pts',(-29.4632121945934,20.7979059786151,4.37428742464127));
#45914=CARTESIAN_POINT('Ctrl Pts',(-29.4565005209999,20.7763746296517,4.37593323382873));
#45915=CARTESIAN_POINT('Ctrl Pts',(-29.4488131569132,20.7551568610949,4.37779376198798));
#45916=CARTESIAN_POINT('Ctrl Pts',(-29.4462651977887,20.7481242805658,4.37841042976204));
#45917=CARTESIAN_POINT('Ctrl Pts',(-29.4436100535821,20.7411261537694,4.3790507017421));
#45918=CARTESIAN_POINT('Ctrl Pts',(-29.4408477969706,20.7341623429493,4.37971382159266));
#45919=CARTESIAN_POINT('Ctrl Pts',(-29.4352997116543,20.7201752946803,4.38104572011743));
#45920=CARTESIAN_POINT('Ctrl Pts',(-29.429320357937,20.7063265823598,4.38246980672111));
#45921=CARTESIAN_POINT('Ctrl Pts',(-29.422910812072,20.6926154355498,4.38398004522345));
#45922=CARTESIAN_POINT('Ctrl Pts',(-29.4205280402512,20.6875182672109,4.38454148184031));
#45923=CARTESIAN_POINT('Ctrl Pts',(-29.4180857816454,20.6824403569271,4.38511479576126));
#45924=CARTESIAN_POINT('Ctrl Pts',(-29.4155840016469,20.6773812076774,4.38569973530258));
#45925=CARTESIAN_POINT('Ctrl Pts',(-29.4147209454693,20.6756359183169,4.38590152590167));
#45926=CARTESIAN_POINT('Ctrl Pts',(-29.413850662798,20.6738927337401,4.38610472707077));
#45927=CARTESIAN_POINT('Ctrl Pts',(-29.4129733677328,20.6721520011351,4.38630927694907));
#45928=CARTESIAN_POINT('Ctrl Pts',(-29.4095530177616,20.6653653281535,4.38710676481617));
#45929=CARTESIAN_POINT('Ctrl Pts',(-29.4060207796651,20.65860648416,4.38792593542571));
#45930=CARTESIAN_POINT('Ctrl Pts',(-29.4024066083896,20.6519284466736,4.38875907393075));
#45931=CARTESIAN_POINT('Ctrl Pts',(-29.4001371996232,20.647735176444,4.38928221787797));
#45932=CARTESIAN_POINT('Ctrl Pts',(-29.3978321856955,20.6435672740895,4.38981165055932));
#45933=CARTESIAN_POINT('Ctrl Pts',(-29.3954948265902,20.6394299308394,4.39034642994758));
#45934=CARTESIAN_POINT('Ctrl Pts',(-29.3884220722315,20.6269104970744,4.39196465080228));
#45935=CARTESIAN_POINT('Ctrl Pts',(-29.3810364699,20.6146350685622,4.39363574521622));
#45936=CARTESIAN_POINT('Ctrl Pts',(-29.3733525338789,20.6025957810371,4.39535118824676));
#45937=CARTESIAN_POINT('Ctrl Pts',(-29.3673996050382,20.5932686573166,4.39668018295247));
#45938=CARTESIAN_POINT('Ctrl Pts',(-29.3612679862125,20.5840830647999,4.39803579888286));
#45939=CARTESIAN_POINT('Ctrl Pts',(-29.3549625690452,20.5750364056405,4.39941427356976));
#45940=CARTESIAN_POINT('Ctrl Pts',(-29.3447906773285,20.5604423454973,4.40163802734804));
#45941=CARTESIAN_POINT('Ctrl Pts',(-29.3341654427046,20.5462068647962,4.40392168341668));
#45942=CARTESIAN_POINT('Ctrl Pts',(-29.3231032810787,20.5323157427589,4.40625078658438));
#45943=CARTESIAN_POINT('Ctrl Pts',(-29.3155317896742,20.5228079707103,4.40784494016942));
#45944=CARTESIAN_POINT('Ctrl Pts',(-29.3077555903465,20.5134615445095,4.40946043956847));
#45945=CARTESIAN_POINT('Ctrl Pts',(-29.2997767506546,20.5042737135194,4.41109279276069));
#45946=CARTESIAN_POINT('Ctrl Pts',(-29.2885663431556,20.4913646523768,4.41338627717365));
#45947=CARTESIAN_POINT('Ctrl Pts',(-29.2769568348822,20.4787683533196,4.41571308352564));
#45948=CARTESIAN_POINT('Ctrl Pts',(-29.2649547579802,20.4664781747352,4.41806118409384));
#45949=CARTESIAN_POINT('Ctrl Pts',(-29.2559339982298,20.4572408777904,4.41982601623651));
#45950=CARTESIAN_POINT('Ctrl Pts',(-29.246690765677,20.4481765788377,4.42160290420698));
#45951=CARTESIAN_POINT('Ctrl Pts',(-29.2372257463337,20.4392844579056,4.42338663097564));
#45952=CARTESIAN_POINT('Ctrl Pts',(-29.2357824384442,20.4379285105134,4.42365862903761));
#45953=CARTESIAN_POINT('Ctrl Pts',(-29.2343339292738,20.4365765234704,4.42393079522064));
#45954=CARTESIAN_POINT('Ctrl Pts',(-29.2328802517791,20.4352285214994,4.42420310602461));
#45955=CARTESIAN_POINT('Ctrl Pts',(-29.228779764045,20.4314261199573,4.42497123177162));
#45956=CARTESIAN_POINT('Ctrl Pts',(-29.224649830871,20.4276662781706,4.42573831030471));
#45957=CARTESIAN_POINT('Ctrl Pts',(-29.2204919524299,20.4239491692082,4.4265037708607));
#45958=CARTESIAN_POINT('Ctrl Pts',(-29.2148600507244,20.4189142956299,4.42754059737495));
#45959=CARTESIAN_POINT('Ctrl Pts',(-29.2091763097764,20.4139573124958,4.42857455648857));
#45960=CARTESIAN_POINT('Ctrl Pts',(-29.2034417856259,20.4090764056792,4.42960472148362));
#45961=CARTESIAN_POINT('Ctrl Pts',(-29.2019739526209,20.4078270681698,4.42986840686372));
#45962=CARTESIAN_POINT('Ctrl Pts',(-29.2005027900015,20.4065827309674,4.43013184020828));
#45963=CARTESIAN_POINT('Ctrl Pts',(-29.1990283323788,20.4053433739984,4.43039500427588));
#45964=CARTESIAN_POINT('Ctrl Pts',(-29.1889819796394,20.3968989012052,4.43218809687529));
#45965=CARTESIAN_POINT('Ctrl Pts',(-29.1787816675667,20.3886839680143,4.43396892744536));
#45966=CARTESIAN_POINT('Ctrl Pts',(-29.1684325608492,20.3806911215074,4.4357329453857));
#45967=CARTESIAN_POINT('Ctrl Pts',(-29.154829586387,20.3701852401901,4.43805158907628));
#45968=CARTESIAN_POINT('Ctrl Pts',(-29.1409683057726,20.3600635818434,4.44034101948239));
#45969=CARTESIAN_POINT('Ctrl Pts',(-29.1268573005585,20.3503117232733,4.44259090921445));
#45970=CARTESIAN_POINT('Ctrl Pts',(-29.1163458403702,20.343047444679,4.4442668795644));
#45971=CARTESIAN_POINT('Ctrl Pts',(-29.1056957917177,20.3359883984724,4.44592095804887));
#45972=CARTESIAN_POINT('Ctrl Pts',(-29.0949083371168,20.3291312146284,4.44754895806742));
#45973=CARTESIAN_POINT('Ctrl Pts',(-29.0797948733191,20.3195241475662,4.44982982229845));
#45974=CARTESIAN_POINT('Ctrl Pts',(-29.0644122897058,20.3103127098318,4.45205964031271));
#45975=CARTESIAN_POINT('Ctrl Pts',(-29.0487649387269,20.3014886351646,4.45422727163098));
#45976=CARTESIAN_POINT('Ctrl Pts',(-29.0382506909112,20.2955592923691,4.45568381292568));
#45977=CARTESIAN_POINT('Ctrl Pts',(-29.0276166084402,20.2898051592413,4.45711226285544));
#45978=CARTESIAN_POINT('Ctrl Pts',(-29.016862654098,20.2842252122415,4.45850921188307));
#45979=CARTESIAN_POINT('Ctrl Pts',(-29.0137406770345,20.2826052996034,4.45891475971082));
#45980=CARTESIAN_POINT('Ctrl Pts',(-29.0106091998765,20.2810003697014,4.45931757794315));
#45981=CARTESIAN_POINT('Ctrl Pts',(-29.0074679133908,20.2794102180322,4.45971762954353));
#45982=CARTESIAN_POINT('Ctrl Pts',(-28.9971474318437,20.2741858836601,4.46103197167007));
#45983=CARTESIAN_POINT('Ctrl Pts',(-28.9867108167574,20.2691163199733,4.46231765695496));
#45984=CARTESIAN_POINT('Ctrl Pts',(-28.9761693954237,20.2642067288857,4.46357037351109));
#45985=CARTESIAN_POINT('Ctrl Pts',(-28.9723369419537,20.2624217912759,4.46402581284516));
#45986=CARTESIAN_POINT('Ctrl Pts',(-28.9684910649499,20.2606582186039,4.46447684003569));
#45987=CARTESIAN_POINT('Ctrl Pts',(-28.9646329082511,20.2589165824116,4.46492316881479));
#45988=CARTESIAN_POINT('Ctrl Pts',(-28.961569978256,20.257533924798,4.46527750222113));
#45989=CARTESIAN_POINT('Ctrl Pts',(-28.9585030873642,20.256166717489,4.46562844571048));
#45990=CARTESIAN_POINT('Ctrl Pts',(-28.9554323067952,20.2548148767914,4.46597595326881));
#45991=CARTESIAN_POINT('Ctrl Pts',(-28.9484934807138,20.2517602177952,4.46676119156735));
#45992=CARTESIAN_POINT('Ctrl Pts',(-28.9415314764778,20.2487826803726,4.46752922468682));
#45993=CARTESIAN_POINT('Ctrl Pts',(-28.9345467044577,20.2458807444744,4.46827970500645));
#45994=CARTESIAN_POINT('Ctrl Pts',(-28.9151642248849,20.2378279815343,4.47036225965865));
#45995=CARTESIAN_POINT('Ctrl Pts',(-28.8956059486648,20.2303585263828,4.4723092627131));
#45996=CARTESIAN_POINT('Ctrl Pts',(-28.8758774726147,20.2234510771608,4.47411036362058));
#45997=CARTESIAN_POINT('Ctrl Pts',(-28.8671681201616,20.2204017078292,4.47490547939976));
#45998=CARTESIAN_POINT('Ctrl Pts',(-28.8584255903597,20.2174618973078,4.47567217444019));
#45999=CARTESIAN_POINT('Ctrl Pts',(-28.8496499871138,20.2146308023702,4.47640958818901));
#46000=CARTESIAN_POINT('Ctrl Pts',(-28.8279227455547,20.2076213829761,4.478235327822));
#46001=CARTESIAN_POINT('Ctrl Pts',(-28.8059933800392,20.2012769372787,4.47988199179129));
#46002=CARTESIAN_POINT('Ctrl Pts',(-28.7838646067432,20.1955853468773,4.48133681237158));
#46003=CARTESIAN_POINT('Ctrl Pts',(-28.776809684112,20.1937707984886,4.48180062690387));
#46004=CARTESIAN_POINT('Ctrl Pts',(-28.769734499636,20.1920226012458,4.48224495215947));
#46005=CARTESIAN_POINT('Ctrl Pts',(-28.7626389680079,20.1903408137018,4.4826693708897));
#46006=CARTESIAN_POINT('Ctrl Pts',(-28.7381896799774,20.1845458274732,4.4841318033507));
#46007=CARTESIAN_POINT('Ctrl Pts',(-28.7134995184439,20.1795376786906,4.48535837645559));
#46008=CARTESIAN_POINT('Ctrl Pts',(-28.6885669332602,20.1753183905708,4.48633263463277));
#46009=CARTESIAN_POINT('Ctrl Pts',(-28.6835676332246,20.1744723697073,4.48652798577281));
#46010=CARTESIAN_POINT('Ctrl Pts',(-28.6785585585997,20.1736581381179,4.48671319150791));
#46011=CARTESIAN_POINT('Ctrl Pts',(-28.6735396612379,20.1728758059763,4.4868881172469));
#46012=CARTESIAN_POINT('Ctrl Pts',(-28.6704354517054,20.1723919301931,4.48699630956632));
#46013=CARTESIAN_POINT('Ctrl Pts',(-28.667328116131,20.1719203450063,4.48710055087429));
#46014=CARTESIAN_POINT('Ctrl Pts',(-28.6642171269454,20.1714609861963,4.48720083066601));
#46015=CARTESIAN_POINT('Ctrl Pts',(-28.6597994044565,20.1708086792854,4.4873432317689));
#46016=CARTESIAN_POINT('Ctrl Pts',(-28.6553706485648,20.1701805791297,4.48747773248562));
#46017=CARTESIAN_POINT('Ctrl Pts',(-28.6509366884823,20.1695774849372,4.48760410629557));
#46018=CARTESIAN_POINT('Ctrl Pts',(-28.647181504148,20.169066715823,4.48771113408621));
#46019=CARTESIAN_POINT('Ctrl Pts',(-28.6434213870889,20.1685737240394,4.48781236546092));
#46020=CARTESIAN_POINT('Ctrl Pts',(-28.6396608841676,20.1680991871688,4.48790761646221));
#46021=CARTESIAN_POINT('Ctrl Pts',(-28.6358543008539,20.1676188354257,4.48800403464875));
#46022=CARTESIAN_POINT('Ctrl Pts',(-28.6320482362219,20.1671574287393,4.48809432417053));
#46023=CARTESIAN_POINT('Ctrl Pts',(-28.6282428208247,20.1667148882399,4.48817848501042));
#46024=CARTESIAN_POINT('Ctrl Pts',(-28.6156464496165,20.1652500272923,4.48845706725958));
#46025=CARTESIAN_POINT('Ctrl Pts',(-28.603052964721,20.1639913732817,4.48866859713531));
#46026=CARTESIAN_POINT('Ctrl Pts',(-28.590462340133,20.1629357314628,4.48881310846486));
#46027=CARTESIAN_POINT('Ctrl Pts',(-28.5879303379186,20.1627234395781,4.48884217001013));
#46028=CARTESIAN_POINT('Ctrl Pts',(-28.5853984512941,20.1625193432353,4.4888685206279));
#46029=CARTESIAN_POINT('Ctrl Pts',(-28.5828666801655,20.1623234310325,4.488892161079));
#46030=CARTESIAN_POINT('Ctrl Pts',(-28.5526241869252,20.1599832220774,4.48917455081571));
#46031=CARTESIAN_POINT('Ctrl Pts',(-28.5223981639468,20.1588102781325,4.48907040538594));
#46032=CARTESIAN_POINT('Ctrl Pts',(-28.492188453501,20.1587864726715,4.48858057664305));
#46033=CARTESIAN_POINT('',(-17.2867694013439,20.1504205562397,4.30719763801101));
#46034=CARTESIAN_POINT('Ctrl Pts',(-28.492188453501,20.1587864726715,4.48858057664304));
#46035=CARTESIAN_POINT('Ctrl Pts',(-24.7570506191739,20.1558431582048,4.42801800113474));
#46036=CARTESIAN_POINT('Ctrl Pts',(-21.0219109331918,20.1530630626027,4.36756184755652));
#46037=CARTESIAN_POINT('Ctrl Pts',(-17.2867696586256,20.1504216822361,4.30719785610076));
#46038=CARTESIAN_POINT('',(-17.2461080117266,18.1757197899201,7.));
#46039=CARTESIAN_POINT('Ctrl Pts',(-17.2867699753103,20.1504209513526,4.30719809188305));
#46040=CARTESIAN_POINT('Ctrl Pts',(-17.3208257192627,20.071822958759,4.33255373642374));
#46041=CARTESIAN_POINT('Ctrl Pts',(-17.3535476746569,19.9938851605761,4.36146905604493));
#46042=CARTESIAN_POINT('Ctrl Pts',(-17.4004272525326,19.8779754334467,4.41045157774795));
#46043=CARTESIAN_POINT('Ctrl Pts',(-17.4233147516175,19.8202699530577,4.43634776622695));
#46044=CARTESIAN_POINT('Ctrl Pts',(-17.4453203036792,19.7629423461442,4.46442773366274));
#46045=CARTESIAN_POINT('Ctrl Pts',(-17.4597874908418,19.7248085032196,4.48364358525879));
#46046=CARTESIAN_POINT('Ctrl Pts',(-17.4669273739776,19.7057623714905,4.4935111894555));
#46047=CARTESIAN_POINT('Ctrl Pts',(-17.5019467009911,19.6111618337293,4.54389102196789));
#46048=CARTESIAN_POINT('Ctrl Pts',(-17.5278706528003,19.537295520511,4.58761089528929));
#46049=CARTESIAN_POINT('Ctrl Pts',(-17.5752369806953,19.3931873285045,4.68200405571982));
#46050=CARTESIAN_POINT('Ctrl Pts',(-17.5966805850057,19.3229450588183,4.73267627680039));
#46051=CARTESIAN_POINT('Ctrl Pts',(-17.6346156200307,19.1861771553916,4.84130234246955));
#46052=CARTESIAN_POINT('Ctrl Pts',(-17.6511094474768,19.1196505679119,4.8992538406938));
#46053=CARTESIAN_POINT('Ctrl Pts',(-17.6681966114296,19.0389449588237,4.97660963956145));
#46054=CARTESIAN_POINT('Ctrl Pts',(-17.6714220915483,19.0229959339583,4.99226140241664));
#46055=CARTESIAN_POINT('Ctrl Pts',(-17.6774786818592,18.9915153566521,5.02388879094697));
#46056=CARTESIAN_POINT('Ctrl Pts',(-17.6859756358375,18.9449029840238,5.07183293884616));
#46057=CARTESIAN_POINT('Ctrl Pts',(-17.6926947074833,18.9001035758318,5.12127726254189));
#46058=CARTESIAN_POINT('Ctrl Pts',(-17.703709514897,18.8129042024216,5.22215494584585));
#46059=CARTESIAN_POINT('Ctrl Pts',(-17.7078275163219,18.7579651770337,5.29205430864768));
#46060=CARTESIAN_POINT('Ctrl Pts',(-17.7091952476915,18.6545099125253,5.43719659709591));
#46061=CARTESIAN_POINT('Ctrl Pts',(-17.7064463567172,18.6059930873587,5.51243899701703));
#46062=CARTESIAN_POINT('Ctrl Pts',(-17.6991407639401,18.5551445709081,5.60020358607968));
#46063=CARTESIAN_POINT('Ctrl Pts',(-17.6982694593839,18.5495414765602,5.61000793743428));
#46064=CARTESIAN_POINT('Ctrl Pts',(-17.6964128600498,18.5384679700224,5.62965390264442));
#46065=CARTESIAN_POINT('Ctrl Pts',(-17.6934584932203,18.5220630392232,5.65916663843846));
#46066=CARTESIAN_POINT('Ctrl Pts',(-17.685384085205,18.4852072119293,5.72833147537855));
#46067=CARTESIAN_POINT('Ctrl Pts',(-17.676455706464,18.4560061760419,5.78811746154919));
#46068=CARTESIAN_POINT('Ctrl Pts',(-17.6559536600445,18.4006832919842,5.90832310966332));
#46069=CARTESIAN_POINT('Ctrl Pts',(-17.6387627137838,18.3679005667132,5.98930349659442));
#46070=CARTESIAN_POINT('Ctrl Pts',(-17.5973924447825,18.3101371654525,6.15280666091991));
#46071=CARTESIAN_POINT('Ctrl Pts',(-17.5732126955704,18.2851576196246,6.23532979134612));
#46072=CARTESIAN_POINT('Ctrl Pts',(-17.5385754612136,18.2586835344225,6.33938793190696));
#46073=CARTESIAN_POINT('Ctrl Pts',(-17.5314210668692,18.2536232472437,6.36026115366522));
#46074=CARTESIAN_POINT('Ctrl Pts',(-17.5167222918182,18.2440104157202,6.4019466819254));
#46075=CARTESIAN_POINT('Ctrl Pts',(-17.5091735113904,18.2394538697671,6.42277317881695));
#46076=CARTESIAN_POINT('Ctrl Pts',(-17.4975544336796,18.2329867994005,6.45398810171667));
#46077=CARTESIAN_POINT('Ctrl Pts',(-17.4936310903107,18.2308919767749,6.46439142406025));
#46078=CARTESIAN_POINT('Ctrl Pts',(-17.4857011391769,18.2268311508652,6.48515121686447));
#46079=CARTESIAN_POINT('Ctrl Pts',(-17.4736763159107,18.2209302438205,6.51623424645934));
#46080=CARTESIAN_POINT('Ctrl Pts',(-17.4281734265522,18.20135436499,6.62958911199627));
#46081=CARTESIAN_POINT('Ctrl Pts',(-17.3826445834544,18.1895780498687,6.73081934613577));
#46082=CARTESIAN_POINT('Ctrl Pts',(-17.3127519420792,18.1788281172695,6.87449306774556));
#46083=CARTESIAN_POINT('Ctrl Pts',(-17.2801713026602,18.1762507473026,6.93757304535173));
#46084=CARTESIAN_POINT('Ctrl Pts',(-17.2461080117266,18.1757197899201,7.));
#46085=CARTESIAN_POINT('',(-37.7046869279002,18.4953857332484,7.));
#46086=CARTESIAN_POINT('',(-6.,18.,7.));
#46087=CARTESIAN_POINT('',(-37.7046869279001,23.4998565514917,7.15430439779759));
#46088=CARTESIAN_POINT('Origin',(-37.7046869279001,21.,7.));
#46089=CARTESIAN_POINT('',(-31.4046869279001,23.6003888166982,7.11771364567903));
#46090=CARTESIAN_POINT('Ctrl Pts',(-37.7046869279001,23.4998565514917,7.15430439779759));
#46091=CARTESIAN_POINT('Ctrl Pts',(-36.1624028751846,23.524555494072,7.14531471788049));
#46092=CARTESIAN_POINT('Ctrl Pts',(-34.620117596862,23.5491869331956,7.13634960721236));
#46093=CARTESIAN_POINT('Ctrl Pts',(-33.0778312194337,23.5737573593539,7.12740670344752));
#46094=CARTESIAN_POINT('Ctrl Pts',(-32.6184875763975,23.5810752409274,7.12474321237687));
#46095=CARTESIAN_POINT('Ctrl Pts',(-32.0607728361779,23.5899537087511,7.12151171436315));
#46096=CARTESIAN_POINT('Ctrl Pts',(-31.503057956262,23.5988244202026,7.11828303943805));
#46097=CARTESIAN_POINT('Ctrl Pts',(-31.4046869279001,23.6003888166982,7.11771364567903));
#46098=CARTESIAN_POINT('',(-31.4046869279001,19.0836514699531,8.76167159589278));
#46099=CARTESIAN_POINT('Origin',(-31.4046869279001,21.,7.));
#46100=CARTESIAN_POINT('',(-37.7046869279002,19.1841837351597,8.72508084377422));
#46101=CARTESIAN_POINT('Ctrl Pts',(-31.4046869279001,19.0836514699531,8.76167159589278));
#46102=CARTESIAN_POINT('Ctrl Pts',(-31.503057956262,19.0852158664487,8.76110220213375));
#46103=CARTESIAN_POINT('Ctrl Pts',(-31.601428980305,19.0867805027715,8.76053272108482));
#46104=CARTESIAN_POINT('Ctrl Pts',(-31.6998,19.0883453804229,8.75996315219946));
#46105=CARTESIAN_POINT('Ctrl Pts',(-33.4052019268744,19.1154747663967,8.75008886323108));
#46106=CARTESIAN_POINT('Ctrl Pts',(-35.1106025511401,19.1426765782906,8.74018821338358));
#46107=CARTESIAN_POINT('Ctrl Pts',(-36.8160017078461,19.1699592983337,8.73025811537809));
#46108=CARTESIAN_POINT('Ctrl Pts',(-37.1122301591213,19.1746983166879,8.72853325375751));
#46109=CARTESIAN_POINT('Ctrl Pts',(-37.4084585661232,19.1794397794108,8.72680750245948));
#46110=CARTESIAN_POINT('Ctrl Pts',(-37.7046869279002,19.1841837351597,8.72508084377422));
#46111=CARTESIAN_POINT('Origin',(-37.7046869279001,21.,7.));
#46112=CARTESIAN_POINT('',(-13.9943709817605,20.1406244663727,9.74364801533398));
#46113=CARTESIAN_POINT('Ctrl Pts',(-17.2461080117266,18.1757197899201,7.));
#46114=CARTESIAN_POINT('Ctrl Pts',(-17.2374845700418,18.1755853730772,7.01580396926482));
#46115=CARTESIAN_POINT('Ctrl Pts',(-17.2287661057066,18.1755821101472,7.03156608650189));
#46116=CARTESIAN_POINT('Ctrl Pts',(-17.1763326909695,18.1763288548473,7.12510606643033));
#46117=CARTESIAN_POINT('Ctrl Pts',(-17.130413388618,18.1801068975316,7.20191231344627));
#46118=CARTESIAN_POINT('Ctrl Pts',(-17.0702785978487,18.1885224733183,7.29671107593985));
#46119=CARTESIAN_POINT('Ctrl Pts',(-17.0581024000519,18.1903928724755,7.31562872420576));
#46120=CARTESIAN_POINT('Ctrl Pts',(-17.0335791359912,18.1944811541833,7.35319187234959));
#46121=CARTESIAN_POINT('Ctrl Pts',(-16.9965140945174,18.2011373096274,7.40916741270535));
#46122=CARTESIAN_POINT('Ctrl Pts',(-16.9586325955796,18.2093134720725,7.46406874755071));
#46123=CARTESIAN_POINT('Ctrl Pts',(-16.881837046061,18.2275755679313,7.57251632857413));
#46124=CARTESIAN_POINT('Ctrl Pts',(-16.8292652167036,18.2422918218164,7.64301081819979));
#46125=CARTESIAN_POINT('Ctrl Pts',(-16.7216151897572,18.276322662728,7.78072073500009));
#46126=CARTESIAN_POINT('Ctrl Pts',(-16.6665364004662,18.2956386676755,7.84793529715628));
#46127=CARTESIAN_POINT('Ctrl Pts',(-16.5540588873242,18.3385266250333,7.97932936266556));
#46128=CARTESIAN_POINT('Ctrl Pts',(-16.496659786943,18.362099434901,8.04350832782672));
#46129=CARTESIAN_POINT('Ctrl Pts',(-16.4089303610114,18.4004724064477,8.13763727160809));
#46130=CARTESIAN_POINT('Ctrl Pts',(-16.3794151366119,18.4137664344875,8.16865656743358));
#46131=CARTESIAN_POINT('Ctrl Pts',(-16.33474556304,18.4344457762559,8.21466361265896));
#46132=CARTESIAN_POINT('Ctrl Pts',(-16.3197785925108,18.4414672349154,8.22992330103603));
#46133=CARTESIAN_POINT('Ctrl Pts',(-16.2897774767356,18.4557238173284,8.26020696428227));
#46134=CARTESIAN_POINT('Ctrl Pts',(-16.2146133970836,18.4918961529488,8.33532057783537));
#46135=CARTESIAN_POINT('Ctrl Pts',(-16.0779109948858,18.5616689299404,8.46530633625082));
#46136=CARTESIAN_POINT('Ctrl Pts',(-15.8929500681926,18.6639819795036,8.62836707437087));
#46137=CARTESIAN_POINT('Ctrl Pts',(-15.7055634000057,18.7751395847501,8.78182921325318));
#46138=CARTESIAN_POINT('Ctrl Pts',(-15.5159845124422,18.8948891297535,8.92617004052537));
#46139=CARTESIAN_POINT('Ctrl Pts',(-15.3882781701595,18.9803912140309,9.01653479984028));
#46140=CARTESIAN_POINT('Ctrl Pts',(-15.2920527636081,19.0466610460811,9.08215821710572));
#46141=CARTESIAN_POINT('Ctrl Pts',(-15.2438286045929,19.0803323938859,9.11443187566169));
#46142=CARTESIAN_POINT('Ctrl Pts',(-15.1954462683221,19.1148173577572,9.14590290763911));
#46143=CARTESIAN_POINT('Ctrl Pts',(-15.1631572166934,19.1379895449502,9.16670540807019));
#46144=CARTESIAN_POINT('Ctrl Pts',(-15.1469886722597,19.1496718364991,9.17702188510648));
#46145=CARTESIAN_POINT('Ctrl Pts',(-15.0662279656308,19.2084219980857,9.22805559353009));
#46146=CARTESIAN_POINT('Ctrl Pts',(-14.9373315528598,19.3047303334721,9.30633637519877));
#46147=CARTESIAN_POINT('Ctrl Pts',(-14.745157724316,19.456198658285,9.4139193981442));
#46148=CARTESIAN_POINT('Ctrl Pts',(-14.554399737518,19.6148926439594,9.51177846055287));
#46149=CARTESIAN_POINT('Ctrl Pts',(-14.3653491692332,19.7811828464356,9.59985942251706));
#46150=CARTESIAN_POINT('Ctrl Pts',(-14.2406886289955,19.8974714244525,9.65190302383858));
#46151=CARTESIAN_POINT('Ctrl Pts',(-14.1168602614401,20.0167316186446,9.70045488642478));
#46152=CARTESIAN_POINT('Ctrl Pts',(-14.0553617214042,20.0778465000411,9.72298583483569));
#46153=CARTESIAN_POINT('Ctrl Pts',(-13.9943709817605,20.1406244663727,9.74364801533398));
#46154=CARTESIAN_POINT('',(-13.7129564349448,20.6615335048058,9.85952349485951));
#46155=CARTESIAN_POINT('Ctrl Pts',(-13.9943709817604,20.1406244663728,9.74364801533398));
#46156=CARTESIAN_POINT('Ctrl Pts',(-13.9678155062267,20.1679580970929,9.7526443631144));
#46157=CARTESIAN_POINT('Ctrl Pts',(-13.9423330747277,20.1962188425863,9.76146424305687));
#46158=CARTESIAN_POINT('Ctrl Pts',(-13.9181306824652,20.2255898589142,9.77006745101129));
#46159=CARTESIAN_POINT('Ctrl Pts',(-13.9106257065011,20.2346975855055,9.77273523972456));
#46160=CARTESIAN_POINT('Ctrl Pts',(-13.9032441390017,20.2439122365762,9.77538212412262));
#46161=CARTESIAN_POINT('Ctrl Pts',(-13.8959930675324,20.2532397371734,9.77800670735638));
#46162=CARTESIAN_POINT('Ctrl Pts',(-13.894459989469,20.2552118300721,9.77856161720638));
#46163=CARTESIAN_POINT('Ctrl Pts',(-13.8929328029768,20.2571889081341,9.77911551270585));
#46164=CARTESIAN_POINT('Ctrl Pts',(-13.8914115564317,20.2591710522661,9.77966838704705));
#46165=CARTESIAN_POINT('Ctrl Pts',(-13.8777336839485,20.276992959417,9.78463940555978));
#46166=CARTESIAN_POINT('Ctrl Pts',(-13.8645321513175,20.2952317214795,9.78952955576498));
#46167=CARTESIAN_POINT('Ctrl Pts',(-13.8518728105507,20.3139384256743,9.79432607313674));
#46168=CARTESIAN_POINT('Ctrl Pts',(-13.8500982491222,20.3165606945848,9.79499843948473));
#46169=CARTESIAN_POINT('Ctrl Pts',(-13.848334638917,20.3191917804785,9.79566886174757));
#46170=CARTESIAN_POINT('Ctrl Pts',(-13.846582196565,20.321831792061,9.79633729347187));
#46171=CARTESIAN_POINT('Ctrl Pts',(-13.8413886567631,20.3296557328692,9.79831825835845));
#46172=CARTESIAN_POINT('Ctrl Pts',(-13.8363073992497,20.3375366388824,9.80027632033235));
#46173=CARTESIAN_POINT('Ctrl Pts',(-13.8313424796597,20.3454770830741,9.80221067100469));
#46174=CARTESIAN_POINT('Ctrl Pts',(-13.8229125974778,20.3589590756412,9.8054949836649));
#46175=CARTESIAN_POINT('Ctrl Pts',(-13.8148176348778,20.372613333958,9.80871112397037));
#46176=CARTESIAN_POINT('Ctrl Pts',(-13.8070804182788,20.3864513682538,9.81185433149902));
#46177=CARTESIAN_POINT('Ctrl Pts',(-13.7965338154804,20.4053139979037,9.81613883884006));
#46178=CARTESIAN_POINT('Ctrl Pts',(-13.7866491922786,20.4245175913989,9.82028832080854));
#46179=CARTESIAN_POINT('Ctrl Pts',(-13.7774996931455,20.4440988084439,9.82428825257612));
#46180=CARTESIAN_POINT('Ctrl Pts',(-13.7669251796949,20.466729756872,9.82891116489764));
#46181=CARTESIAN_POINT('Ctrl Pts',(-13.7573319687151,20.4898647835373,9.83333444164274));
#46182=CARTESIAN_POINT('Ctrl Pts',(-13.7488489882647,20.5135706416344,9.83753261467546));
#46183=CARTESIAN_POINT('Ctrl Pts',(-13.7480286665604,20.5158630470016,9.83793858666573));
#46184=CARTESIAN_POINT('Ctrl Pts',(-13.7472187561872,20.5181608018945,9.8383424508099));
#46185=CARTESIAN_POINT('Ctrl Pts',(-13.7464193789805,20.520463975649,9.83874418260543));
#46186=CARTESIAN_POINT('Ctrl Pts',(-13.7430855599168,20.530069409111,9.84041961331223));
#46187=CARTESIAN_POINT('Ctrl Pts',(-13.7399346038681,20.5397690428386,9.84205802015337));
#46188=CARTESIAN_POINT('Ctrl Pts',(-13.7369778918466,20.5495685335625,9.84365718794162));
#46189=CARTESIAN_POINT('Ctrl Pts',(-13.7346205393843,20.5573815547226,9.84493218601245));
#46190=CARTESIAN_POINT('Ctrl Pts',(-13.7323843611739,20.5652681120244,9.84618372560941));
#46191=CARTESIAN_POINT('Ctrl Pts',(-13.7302881581844,20.5731813035807,9.8474030924272));
#46192=CARTESIAN_POINT('Ctrl Pts',(-13.7291247796699,20.5775730714983,9.84807983278311));
#46193=CARTESIAN_POINT('Ctrl Pts',(-13.7280038555256,20.58197485668,9.8487469873088));
#46194=CARTESIAN_POINT('Ctrl Pts',(-13.726925950927,20.5863867852498,9.84940444264791));
#46195=CARTESIAN_POINT('Ctrl Pts',(-13.7208857536075,20.6111096773842,9.85308859056077));
#46196=CARTESIAN_POINT('Ctrl Pts',(-13.7161966218325,20.6361508131826,9.85646810013119));
#46197=CARTESIAN_POINT('Ctrl Pts',(-13.7129564349448,20.6615335048058,9.8595234948595));
#46198=CARTESIAN_POINT('Ctrl Pts',(-13.7129564349448,20.6615335048058,9.85952349485952));
#46199=CARTESIAN_POINT('Ctrl Pts',(-13.7036527253464,20.7344160883897,9.86829660154869));
#46200=CARTESIAN_POINT('Ctrl Pts',(-13.6973734530137,20.8072675266628,9.87419602162833));
#46201=CARTESIAN_POINT('Ctrl Pts',(-13.6940900143325,20.8800864282419,9.87728216942434));
#46202=CARTESIAN_POINT('Ctrl Pts',(-13.6930332737108,20.9035224350612,9.87827541402463));
#46203=CARTESIAN_POINT('Ctrl Pts',(-13.6922868437377,20.9269551735342,9.87897686532106));
#46204=CARTESIAN_POINT('Ctrl Pts',(-13.691849770872,20.9503848193212,9.87938741553639));
#46205=CARTESIAN_POINT('Ctrl Pts',(-13.6904743566214,21.0241150168119,9.88067936628678));
#46206=CARTESIAN_POINT('Ctrl Pts',(-13.6921624494699,21.0978128650641,9.87909442673253));
#46207=CARTESIAN_POINT('Ctrl Pts',(-13.6969164901419,21.1714789657059,9.87462563650867));
#46208=CARTESIAN_POINT('Ctrl Pts',(-13.6983671737571,21.1939579919851,9.87326199635393));
#46209=CARTESIAN_POINT('Ctrl Pts',(-13.7001033430898,21.2164340423875,9.87162946024555));
#46210=CARTESIAN_POINT('Ctrl Pts',(-13.7021250674901,21.2389070262678,9.86972686788085));
#46211=CARTESIAN_POINT('Ctrl Pts',(-13.7042868487285,21.2629368470063,9.86769247166067));
#46212=CARTESIAN_POINT('Ctrl Pts',(-13.7067754665188,21.2869632334582,9.865349303113));
#46213=CARTESIAN_POINT('Ctrl Pts',(-13.7095917140698,21.3109861711179,9.86269533148285));
#46214=CARTESIAN_POINT('Ctrl Pts',(-13.7109998378453,21.3229976399478,9.86136834566778));
#46215=CARTESIAN_POINT('Ctrl Pts',(-13.712489868911,21.3350082454893,9.85996364954342));
#46216=CARTESIAN_POINT('Ctrl Pts',(-13.7140619415434,21.3470179869437,9.85848092966431));
#46217=CARTESIAN_POINT('Ctrl Pts',(-13.7156340141758,21.3590277283981,9.8569982097852));
#46218=CARTESIAN_POINT('Ctrl Pts',(-13.717289175782,21.3710435001363,9.85543647401904));
#46219=CARTESIAN_POINT('Ctrl Pts',(-13.7190227227906,21.3830328711285,9.85379994855188));
#46220=CARTESIAN_POINT('Ctrl Pts',(-13.7207562697992,21.3950222421207,9.85216342308471));
#46221=CARTESIAN_POINT('Ctrl Pts',(-13.7225685411701,21.406988586054,9.85045178901428));
#46222=CARTESIAN_POINT('Ctrl Pts',(-13.7244588222449,21.4189320780816,9.84866549501998));
#46223=CARTESIAN_POINT('Ctrl Pts',(-13.7263491033196,21.4308755701092,9.84687920102567));
#46224=CARTESIAN_POINT('Ctrl Pts',(-13.7283185206183,21.4428026752592,9.84501718116659));
#46225=CARTESIAN_POINT('Ctrl Pts',(-13.7303624422929,21.4546908792916,9.84308357311477));
#46226=CARTESIAN_POINT('Ctrl Pts',(-13.734450285642,21.4784672873565,9.83921635701112));
#46227=CARTESIAN_POINT('Ctrl Pts',(-13.7388319210099,21.5020663604287,9.83506680074837));
#46228=CARTESIAN_POINT('Ctrl Pts',(-13.7434962067534,21.5254941628828,9.83064342694144));
#46229=CARTESIAN_POINT('Ctrl Pts',(-13.7561476228294,21.5890397715551,9.81864546078576));
#46230=CARTESIAN_POINT('Ctrl Pts',(-13.7708718347572,21.6513304844594,9.80463565324319));
#46231=CARTESIAN_POINT('Ctrl Pts',(-13.7874862060043,21.7124593155382,9.78875075720091));
#46232=CARTESIAN_POINT('Ctrl Pts',(-13.7953731789483,21.7414776533159,9.7812100718846));
#46233=CARTESIAN_POINT('Ctrl Pts',(-13.8036860947034,21.7702343158064,9.77324607590147));
#46234=CARTESIAN_POINT('Ctrl Pts',(-13.8124054158604,21.7987397797719,9.764869356201));
#46235=CARTESIAN_POINT('Ctrl Pts',(-13.8322758179319,21.8637006890019,9.74577970627396));
#46236=CARTESIAN_POINT('Ctrl Pts',(-13.8542587234846,21.9273544229971,9.72455068576793));
#46237=CARTESIAN_POINT('Ctrl Pts',(-13.878183283974,21.989781098824,9.70127867312322));
#46238=CARTESIAN_POINT('Ctrl Pts',(-13.8868723841143,22.0124536840915,9.69282657017131));
#46239=CARTESIAN_POINT('Ctrl Pts',(-13.8958175984909,22.0349644128231,9.68410448289681));
#46240=CARTESIAN_POINT('Ctrl Pts',(-13.9050107423846,22.0573170274346,9.67511534283697));
#46241=CARTESIAN_POINT('Ctrl Pts',(-13.9136371268844,22.0782915983152,9.66668038528867));
#46242=CARTESIAN_POINT('Ctrl Pts',(-13.9224824295412,22.099126578146,9.65801041030057));
#46243=CARTESIAN_POINT('Ctrl Pts',(-13.931541052428,22.1198243299877,9.64910743888102));
#46244=CARTESIAN_POINT('Ctrl Pts',(-13.9405996753149,22.1405220818294,9.64020446746147));
#46245=CARTESIAN_POINT('Ctrl Pts',(-13.9498749785272,22.1610898312997,9.63106517933433));
#46246=CARTESIAN_POINT('Ctrl Pts',(-13.9593514650354,22.181507469896,9.6217012642152));
#46247=CARTESIAN_POINT('Ctrl Pts',(-13.9783044380518,22.2223427470887,9.60297343397693));
#46248=CARTESIAN_POINT('Ctrl Pts',(-13.9979239435683,22.2622844146239,9.58348365750646));
#46249=CARTESIAN_POINT('Ctrl Pts',(-14.0181458571129,22.301397033398,9.56327145460671));
#46250=CARTESIAN_POINT('Ctrl Pts',(-14.047012829478,22.3572306656996,9.53441834427864));
#46251=CARTESIAN_POINT('Ctrl Pts',(-14.077103469815,22.4113789550291,9.50409285299139));
#46252=CARTESIAN_POINT('Ctrl Pts',(-14.1082729868791,22.4639803192505,9.4723797919722));
#46253=CARTESIAN_POINT('Ctrl Pts',(-14.1207732576489,22.4850756507655,9.4596615375038));
#46254=CARTESIAN_POINT('Ctrl Pts',(-14.1334470488101,22.5059220937757,9.44671952479236));
#46255=CARTESIAN_POINT('Ctrl Pts',(-14.1462850211486,22.5265281049559,9.4335569387938));
#46256=CARTESIAN_POINT('Ctrl Pts',(-14.1808678364504,22.582036393957,9.39809968211153));
#46257=CARTESIAN_POINT('Ctrl Pts',(-14.2166436653731,22.6357989151547,9.3610466312961));
#46258=CARTESIAN_POINT('Ctrl Pts',(-14.2534796534065,22.6879277922558,9.3224484691866));
#46259=CARTESIAN_POINT('Ctrl Pts',(-14.26441529704,22.7034034955946,9.31098968205277));
#46260=CARTESIAN_POINT('Ctrl Pts',(-14.2754443768594,22.7187351039292,9.29939438604579));
#46261=CARTESIAN_POINT('Ctrl Pts',(-14.2865634167636,22.7339252276024,9.28766309180211));
#46262=CARTESIAN_POINT('Ctrl Pts',(-14.2987066132822,22.75051448877,9.27485124719641));
#46263=CARTESIAN_POINT('Ctrl Pts',(-14.3109575323814,22.7669347099736,9.26187741306074));
#46264=CARTESIAN_POINT('Ctrl Pts',(-14.323312446271,22.7831885697824,9.24874219114853));
#46265=CARTESIAN_POINT('Ctrl Pts',(-14.3356673601605,22.7994424295911,9.23560696923631));
#46266=CARTESIAN_POINT('Ctrl Pts',(-14.3481294639689,22.8155339721094,9.22230693586296));
#46267=CARTESIAN_POINT('Ctrl Pts',(-14.3606854713469,22.8314530437744,9.20885290917389));
#46268=CARTESIAN_POINT('Ctrl Pts',(-14.385797486103,22.8632911871044,9.18194485579574));
#46269=CARTESIAN_POINT('Ctrl Pts',(-14.4111704750995,22.8942958355665,9.15454372686061));
#46270=CARTESIAN_POINT('Ctrl Pts',(-14.4367746827933,22.9245107320554,9.12666136044781));
#46271=CARTESIAN_POINT('Ctrl Pts',(-14.4773471154067,22.9723892630523,9.08247895707439));
#46272=CARTESIAN_POINT('Ctrl Pts',(-14.5184980614865,23.0182881012217,9.03708818117602));
#46273=CARTESIAN_POINT('Ctrl Pts',(-14.5601330700439,23.0623326230404,8.99051784601957));
#46274=CARTESIAN_POINT('Ctrl Pts',(-14.5710476049953,23.0738788071163,8.9783095249846));
#46275=CARTESIAN_POINT('Ctrl Pts',(-14.5819954054864,23.0852974233284,8.96601989905037));
#46276=CARTESIAN_POINT('Ctrl Pts',(-14.5929747699614,23.0965904242636,8.95364898597441));
#46277=CARTESIAN_POINT('Ctrl Pts',(-14.6373231856493,23.1422056965305,8.90367975535227));
#46278=CARTESIAN_POINT('Ctrl Pts',(-14.6821873492953,23.185772764633,8.85238878137541));
#46279=CARTESIAN_POINT('Ctrl Pts',(-14.7274828084958,23.2273755535218,8.79977569903656));
#46280=CARTESIAN_POINT('Ctrl Pts',(-14.7361778644479,23.2353617530998,8.78967592959335));
#46281=CARTESIAN_POINT('Ctrl Pts',(-14.7448888135656,23.2432754682488,8.77952732413173));
#46282=CARTESIAN_POINT('Ctrl Pts',(-14.7536150584491,23.2511171438068,8.76932972001199));
#46283=CARTESIAN_POINT('Ctrl Pts',(-14.8003253341024,23.2930924529792,8.71474347979135));
#46284=CARTESIAN_POINT('Ctrl Pts',(-14.8474743525417,23.3330060160619,8.65875697852264));
#46285=CARTESIAN_POINT('Ctrl Pts',(-14.8949923923289,23.3708917389166,8.60133801834855));
#46286=CARTESIAN_POINT('Ctrl Pts',(-14.9025955410729,23.376953663765,8.59215066767327));
#46287=CARTESIAN_POINT('Ctrl Pts',(-14.9102081374154,23.3829635840753,8.58292658058977));
#46288=CARTESIAN_POINT('Ctrl Pts',(-14.9178298957478,23.38892153554,8.57366555667347));
#46289=CARTESIAN_POINT('Ctrl Pts',(-14.9247369087521,23.394320768427,8.56527300342887));
#46290=CARTESIAN_POINT('Ctrl Pts',(-14.9316514833144,23.3996773155833,8.55685012467997));
#46291=CARTESIAN_POINT('Ctrl Pts',(-14.9385734378949,23.4049911793944,8.54839676378748));
#46292=CARTESIAN_POINT('Ctrl Pts',(-14.9454953924754,23.4103050432056,8.539943402895));
#46293=CARTESIAN_POINT('Ctrl Pts',(-14.9524262363533,23.4155773244076,8.53145769055019));
#46294=CARTESIAN_POINT('Ctrl Pts',(-14.959353285948,23.4207986878509,8.5229548624532));
#46295=CARTESIAN_POINT('Ctrl Pts',(-14.9732073851374,23.4312414147376,8.50594920625923));
#46296=CARTESIAN_POINT('Ctrl Pts',(-14.9870564533274,23.4414883605791,8.48886276682353));
#46297=CARTESIAN_POINT('Ctrl Pts',(-15.0008990793685,23.4515418985906,8.47169540755511));
#46298=CARTESIAN_POINT('Ctrl Pts',(-15.0285843314506,23.4716489746137,8.43736068901826));
#46299=CARTESIAN_POINT('Ctrl Pts',(-15.056243820486,23.4909827221071,8.40270247677271));
#46300=CARTESIAN_POINT('Ctrl Pts',(-15.0838673340348,23.5095574077922,8.36771880146978));
#46301=CARTESIAN_POINT('Ctrl Pts',(-15.1327946316088,23.5424572477151,8.30575504408032));
#46302=CARTESIAN_POINT('Ctrl Pts',(-15.1816083488692,23.5729787208378,8.24277073945841));
#46303=CARTESIAN_POINT('Ctrl Pts',(-15.2302598345825,23.6011583270334,8.17874455125467));
#46304=CARTESIAN_POINT('Ctrl Pts',(-15.236543938669,23.6047981661021,8.17047456268122));
#46305=CARTESIAN_POINT('Ctrl Pts',(-15.2428253361195,23.6083988711168,8.16218715798696));
#46306=CARTESIAN_POINT('Ctrl Pts',(-15.2491039220922,23.6119604639728,8.15388226311987));
#46307=CARTESIAN_POINT('Ctrl Pts',(-15.2980136097019,23.6397049903268,8.08918778965834));
#46308=CARTESIAN_POINT('Ctrl Pts',(-15.3467526858593,23.6650797342656,8.02343413429301));
#46309=CARTESIAN_POINT('Ctrl Pts',(-15.3952795899614,23.688065012956,7.95658226498493));
#46310=CARTESIAN_POINT('Ctrl Pts',(-15.4012104696617,23.6908742365261,7.94841173768804));
#46311=CARTESIAN_POINT('Ctrl Pts',(-15.4071381800772,23.6936477058343,7.94022479030037));
#46312=CARTESIAN_POINT('Ctrl Pts',(-15.4130626453345,23.6963853325483,7.93202133999328));
#46313=CARTESIAN_POINT('Ctrl Pts',(-15.4603402908521,23.7182317844597,7.86655723499836));
#46314=CARTESIAN_POINT('Ctrl Pts',(-15.5074112844545,23.7377996181745,7.80004345203389));
#46315=CARTESIAN_POINT('Ctrl Pts',(-15.5542428903708,23.7550185268095,7.73242656333141));
#46316=CARTESIAN_POINT('Ctrl Pts',(-15.5612969456177,23.7576121413231,7.7222417050674));
#46317=CARTESIAN_POINT('Ctrl Pts',(-15.5683455695944,23.7601523666281,7.71203181680802));
#46318=CARTESIAN_POINT('Ctrl Pts',(-15.5753886504285,23.762638858942,7.70179671648233));
#46319=CARTESIAN_POINT('Ctrl Pts',(-15.602289564448,23.7721359693005,7.66270394439485));
#46320=CARTESIAN_POINT('Ctrl Pts',(-15.6291097206323,23.780849799148,7.6232429531147));
#46321=CARTESIAN_POINT('Ctrl Pts',(-15.6558435641724,23.7887579153097,7.58340079166616));
#46322=CARTESIAN_POINT('Ctrl Pts',(-15.6625270250574,23.7907349443502,7.57344025130403));
#46323=CARTESIAN_POINT('Ctrl Pts',(-15.6692027203841,23.7926608334869,7.56345938084566));
#46324=CARTESIAN_POINT('Ctrl Pts',(-15.6758600778727,23.794532483472,7.55347386171613));
#46325=CARTESIAN_POINT('Ctrl Pts',(-15.6825174353613,23.7964041334571,7.54348834258661));
#46326=CARTESIAN_POINT('Ctrl Pts',(-15.689159444701,23.798222436163,7.53349372486578));
#46327=CARTESIAN_POINT('Ctrl Pts',(-15.6957860766278,23.7999874133985,7.52348999736768));
#46328=CARTESIAN_POINT('Ctrl Pts',(-15.7090393404816,23.8035173678694,7.50348254237147));
#46329=CARTESIAN_POINT('Ctrl Pts',(-15.7222310949942,23.8068340407154,7.48343864760626));
#46330=CARTESIAN_POINT('Ctrl Pts',(-15.7353611064557,23.8099373932428,7.4633580913403));
#46331=CARTESIAN_POINT('Ctrl Pts',(-15.7827318779681,23.8211337432174,7.39091097691843));
#46332=CARTESIAN_POINT('Ctrl Pts',(-15.829299054463,23.8295572844193,7.31798752817788));
#46333=CARTESIAN_POINT('Ctrl Pts',(-15.8750507541838,23.8351723271489,7.24458053382367));
#46334=CARTESIAN_POINT('Ctrl Pts',(-15.8800240329711,23.8357826907652,7.23660108278487));
#46335=CARTESIAN_POINT('Ctrl Pts',(-15.8849876760702,23.8363598183367,7.22861591935028));
#46336=CARTESIAN_POINT('Ctrl Pts',(-15.8899416682199,23.8369036267558,7.22062503629825));
#46337=CARTESIAN_POINT('Ctrl Pts',(-15.935236133316,23.8418756797414,7.14756420726362));
#46338=CARTESIAN_POINT('Ctrl Pts',(-15.979723815376,23.8440668153845,7.07402507537809));
#46339=CARTESIAN_POINT('Ctrl Pts',(-16.0233918417347,23.8433845024729,7.00000000000883));
#46340=CARTESIAN_POINT('Origin',(-37.7,21.,7.));
#46341=CARTESIAN_POINT('',(-38.,23.1883393165246,7.26768739878651));
#46342=CARTESIAN_POINT('',(-38.,19.4957009701268,8.6116978427853));
#46343=CARTESIAN_POINT('Origin',(-38.,21.,7.));
#46344=CARTESIAN_POINT('Ctrl Pts',(-37.7046869279001,23.4998565514917,7.15430439779761));
#46345=CARTESIAN_POINT('Ctrl Pts',(-37.7395316670408,23.4992985296346,7.15450750114366));
#46346=CARTESIAN_POINT('Ctrl Pts',(-37.7794800415659,23.4909398979206,7.15754979428675));
#46347=CARTESIAN_POINT('Ctrl Pts',(-37.8454177694196,23.4639858105548,7.16736027977971));
#46348=CARTESIAN_POINT('Ctrl Pts',(-37.8821059412057,23.4393962497117,7.17631014800026));
#46349=CARTESIAN_POINT('Ctrl Pts',(-37.9354044401321,23.3865174575227,7.19555645438101));
#46350=CARTESIAN_POINT('Ctrl Pts',(-37.9607107815143,23.3482518128805,7.20948401002579));
#46351=CARTESIAN_POINT('Ctrl Pts',(-37.9908311196217,23.2758954359896,7.23581957747343));
#46352=CARTESIAN_POINT('Ctrl Pts',(-38.,23.2284905615032,7.25307354074558));
#46353=CARTESIAN_POINT('Ctrl Pts',(-38.,23.1883393165246,7.26768739878653));
#46354=CARTESIAN_POINT('Ctrl Pts',(-38.,19.4957009701268,8.61169784278532));
#46355=CARTESIAN_POINT('Ctrl Pts',(-38.,19.4555497251481,8.62631170082627));
#46356=CARTESIAN_POINT('Ctrl Pts',(-37.9908311196217,19.4081448506618,8.64356566409842));
#46357=CARTESIAN_POINT('Ctrl Pts',(-37.9607107815143,19.3357884737709,8.66990123154606));
#46358=CARTESIAN_POINT('Ctrl Pts',(-37.9354044401321,19.2975228291287,8.68382878719084));
#46359=CARTESIAN_POINT('Ctrl Pts',(-37.8821059412057,19.2446440369396,8.70307509357159));
#46360=CARTESIAN_POINT('Ctrl Pts',(-37.8454177694196,19.2200544760966,8.71202496179214));
#46361=CARTESIAN_POINT('Ctrl Pts',(-37.7794800415659,19.1931003887308,8.7218354472851));
#46362=CARTESIAN_POINT('Ctrl Pts',(-37.7395316670409,19.1847417570168,8.72487774042819));
#46363=CARTESIAN_POINT('Ctrl Pts',(-37.7046869279002,19.1841837351597,8.72508084377424));
#46364=CARTESIAN_POINT('Origin',(6.61287431064084E-15,12.,8.67361737988404E-16));
#46365=CARTESIAN_POINT('',(4.24820533297024E-15,12.5093665794476,19.3089875327072));
#46366=CARTESIAN_POINT('Origin',(3.30643715532042E-15,12.5093665794476,
4.33680868994202E-16));
#46367=CARTESIAN_POINT('',(4.568814811381E-15,19.4906334205533,16.6910124672925));
#46368=CARTESIAN_POINT('',(4.2248130523035E-15,12.,19.5));
#46369=CARTESIAN_POINT('',(-13.2658111744658,19.4906334205523,10.1295681579593));
#46370=CARTESIAN_POINT('Origin',(6.61325378140121E-15,19.4906334205523,
8.67361737988404E-16));
#46371=CARTESIAN_POINT('',(-16.3856910571095,19.4906334689658,3.17789711507297));
#46372=CARTESIAN_POINT('Ctrl Pts',(-13.2658111744658,19.4906334205523,10.1295681579593));
#46373=CARTESIAN_POINT('Ctrl Pts',(-13.3267563717861,19.4032674929026,10.1037375593391));
#46374=CARTESIAN_POINT('Ctrl Pts',(-13.3884259101566,19.3179204250404,10.075220655976));
#46375=CARTESIAN_POINT('Ctrl Pts',(-13.4507036432112,19.2344246756853,10.0441518788645));
#46376=CARTESIAN_POINT('Ctrl Pts',(-13.4570523134828,19.2259130142016,10.0409846887317));
#46377=CARTESIAN_POINT('Ctrl Pts',(-13.4634073117058,19.2174206253153,10.0377909469459));
#46378=CARTESIAN_POINT('Ctrl Pts',(-13.469768514267,19.2089473264459,10.0345707988203));
#46379=CARTESIAN_POINT('Ctrl Pts',(-13.5258079811479,19.1343011967558,10.0062026746325));
#46380=CARTESIAN_POINT('Ctrl Pts',(-13.5823298738816,19.0611374216604,9.97578381795668));
#46381=CARTESIAN_POINT('Ctrl Pts',(-13.6392670213906,18.9893727845524,9.94336645117775));
#46382=CARTESIAN_POINT('Ctrl Pts',(-13.6519731092965,18.9733577956124,9.93613219498486));
#46383=CARTESIAN_POINT('Ctrl Pts',(-13.6646999196863,18.9574126170077,9.9287982659174));
#46384=CARTESIAN_POINT('Ctrl Pts',(-13.6774467134566,18.9415362896475,9.92136524837809));
#46385=CARTESIAN_POINT('Ctrl Pts',(-13.7283032803252,18.8781936547406,9.89170933957969));
#46386=CARTESIAN_POINT('Ctrl Pts',(-13.7794782156711,18.8159476034485,9.86047564177073));
#46387=CARTESIAN_POINT('Ctrl Pts',(-13.8309330026652,18.7547608624783,9.82767434435942));
#46388=CARTESIAN_POINT('Ctrl Pts',(-13.8499593369977,18.732135962864,9.81554547380052));
#46389=CARTESIAN_POINT('Ctrl Pts',(-13.8690240359903,18.7096562047432,9.80320192369851));
#46390=CARTESIAN_POINT('Ctrl Pts',(-13.8881251733158,18.6873196376304,9.79064419604015));
#46391=CARTESIAN_POINT('Ctrl Pts',(-13.9336285571146,18.6341087021369,9.76072874694729));
#46392=CARTESIAN_POINT('Ctrl Pts',(-13.9793388662965,18.5817106162214,9.72959770180917));
#46393=CARTESIAN_POINT('Ctrl Pts',(-14.0252343603869,18.5301127159014,9.69724126768515));
#46394=CARTESIAN_POINT('Ctrl Pts',(-14.0505071373545,18.5016998563687,9.67942389891539));
#46395=CARTESIAN_POINT('Ctrl Pts',(-14.0758362191046,18.4735300880598,9.66123443518788));
#46396=CARTESIAN_POINT('Ctrl Pts',(-14.1012180543646,18.4456012371598,9.64267109998932));
#46397=CARTESIAN_POINT('Ctrl Pts',(-14.1412786350688,18.4015206585098,9.61337227347639));
#46398=CARTESIAN_POINT('Ctrl Pts',(-14.1814707003173,18.3580402718792,9.58314214870423));
#46399=CARTESIAN_POINT('Ctrl Pts',(-14.2217824291453,18.3151599459258,9.55196286685991));
#46400=CARTESIAN_POINT('Ctrl Pts',(-14.2531968841308,18.2817438134852,9.52766522013385));
#46401=CARTESIAN_POINT('Ctrl Pts',(-14.2846839504599,18.2486918389125,9.50279141917903));
#46402=CARTESIAN_POINT('Ctrl Pts',(-14.3162385566473,18.2160051198467,9.47733130486547));
#46403=CARTESIAN_POINT('Ctrl Pts',(-14.3177571907933,18.2144320003028,9.47610598141418));
#46404=CARTESIAN_POINT('Ctrl Pts',(-14.3192759817155,18.2128597284681,9.47487929772981));
#46405=CARTESIAN_POINT('Ctrl Pts',(-14.3207949288989,18.2112883047585,9.47365125229762));
#46406=CARTESIAN_POINT('Ctrl Pts',(-14.3372603013804,18.1942540872504,9.46033925192903));
#46407=CARTESIAN_POINT('Ctrl Pts',(-14.3537439534659,18.1773193481409,9.44686748678888));
#46408=CARTESIAN_POINT('Ctrl Pts',(-14.3702452789957,18.160484438606,9.43323407054952));
#46409=CARTESIAN_POINT('Ctrl Pts',(-14.3703200984053,18.160408106678,9.43317225465766));
#46410=CARTESIAN_POINT('Ctrl Pts',(-14.3703949181347,18.1603317768519,9.43311043547205));
#46411=CARTESIAN_POINT('Ctrl Pts',(-14.3704697381797,18.1602554491316,9.433048612996));
#46412=CARTESIAN_POINT('Ctrl Pts',(-14.3787578810354,18.1518002945171,9.42620026757015));
#46413=CARTESIAN_POINT('Ctrl Pts',(-14.3870535870957,18.1433672280733,9.41930847928004));
#46414=CARTESIAN_POINT('Ctrl Pts',(-14.3953439616599,18.1349691748069,9.41238384586159));
#46415=CARTESIAN_POINT('Ctrl Pts',(-14.4036343362241,18.1265711215405,9.40545921244314));
#46416=CARTESIAN_POINT('Ctrl Pts',(-14.4119193906067,18.1182081087496,9.39850171532258));
#46417=CARTESIAN_POINT('Ctrl Pts',(-14.4201990643658,18.1098799082598,9.39151134982619));
#46418=CARTESIAN_POINT('Ctrl Pts',(-14.421558271936,18.1085127344458,9.39036379764265));
#46419=CARTESIAN_POINT('Ctrl Pts',(-14.422917280404,18.1071465552667,9.38921540373944));
#46420=CARTESIAN_POINT('Ctrl Pts',(-14.4242760645572,18.1057813955388,9.38806618855738));
#46421=CARTESIAN_POINT('Ctrl Pts',(-14.4602193317155,18.0696694783551,9.35766654913436));
#46422=CARTESIAN_POINT('Ctrl Pts',(-14.4960648528319,18.0342100318951,9.32664377669584));
#46423=CARTESIAN_POINT('Ctrl Pts',(-14.5318017642789,17.9993986191631,9.29499961802803));
#46424=CARTESIAN_POINT('Ctrl Pts',(-14.5605504652558,17.9713944393194,9.26954334835129));
#46425=CARTESIAN_POINT('Ctrl Pts',(-14.5892289079274,17.943809019562,9.24368540990711));
#46426=CARTESIAN_POINT('Ctrl Pts',(-14.6178313776236,17.9166428216246,9.21742470121035));
#46427=CARTESIAN_POINT('Ctrl Pts',(-14.6602094841027,17.8763927298999,9.17851620410542));
#46428=CARTESIAN_POINT('Ctrl Pts',(-14.7024236203372,17.8370594141368,9.13872159295134));
#46429=CARTESIAN_POINT('Ctrl Pts',(-14.7444610537933,17.798639696996,9.09803104691099));
#46430=CARTESIAN_POINT('Ctrl Pts',(-14.7673987745469,17.7776759827358,9.07582825512162));
#46431=CARTESIAN_POINT('Ctrl Pts',(-14.7902838993704,17.7569842878885,9.05335872280684));
#46432=CARTESIAN_POINT('Ctrl Pts',(-14.8131141999115,17.7365661645866,9.03061927808011));
#46433=CARTESIAN_POINT('Ctrl Pts',(-14.8601963365352,17.6944585773839,8.98372451024983));
#46434=CARTESIAN_POINT('Ctrl Pts',(-14.9070453477554,17.6535123161777,8.93568335712758));
#46435=CARTESIAN_POINT('Ctrl Pts',(-14.9536422378279,17.6137407654663,8.88646686737394));
#46436=CARTESIAN_POINT('Ctrl Pts',(-14.9710496924444,17.5988830901374,8.86808079460306));
#46437=CARTESIAN_POINT('Ctrl Pts',(-14.9884219698747,17.5841893412295,8.84953071609024));
#46438=CARTESIAN_POINT('Ctrl Pts',(-15.005757957724,17.5696612078881,8.83081432981604));
#46439=CARTESIAN_POINT('Ctrl Pts',(-15.0571595476816,17.526584969063,8.77531982779415));
#46440=CARTESIAN_POINT('Ctrl Pts',(-15.1082422038154,17.4849616812795,8.71836542626731));
#46441=CARTESIAN_POINT('Ctrl Pts',(-15.1589777195974,17.4448351333286,8.65988924371568));
#46442=CARTESIAN_POINT('Ctrl Pts',(-15.1711577983194,17.4352019502349,8.64585086259621));
#46443=CARTESIAN_POINT('Ctrl Pts',(-15.1833178750539,17.4256550106342,8.63172479735828));
#46444=CARTESIAN_POINT('Ctrl Pts',(-15.1954574932711,17.416195331879,8.6175098489441));
#46445=CARTESIAN_POINT('Ctrl Pts',(-15.2507634646902,17.373098694612,8.55274903714184));
#46446=CARTESIAN_POINT('Ctrl Pts',(-15.3056449788749,17.3318093226852,8.48614625302313));
#46447=CARTESIAN_POINT('Ctrl Pts',(-15.3600600510067,17.2924229689497,8.4175851121417));
#46448=CARTESIAN_POINT('Ctrl Pts',(-15.3673414639574,17.2871525853053,8.40841077937746));
#46449=CARTESIAN_POINT('Ctrl Pts',(-15.3746145140432,17.281916335781,8.39920133086733));
#46450=CARTESIAN_POINT('Ctrl Pts',(-15.3818790846534,17.276714535136,8.38995641468225));
#46451=CARTESIAN_POINT('Ctrl Pts',(-15.4076486781805,17.2582622004526,8.35716194614907));
#46452=CARTESIAN_POINT('Ctrl Pts',(-15.433311892242,17.2402426999691,8.3239211011398));
#46453=CARTESIAN_POINT('Ctrl Pts',(-15.458862852334,17.2226705080983,8.29021899737143));
#46454=CARTESIAN_POINT('Ctrl Pts',(-15.4638276648221,17.2192560517597,8.28367033442248));
#46455=CARTESIAN_POINT('Ctrl Pts',(-15.4687883226332,17.2158584353545,8.27710413388084));
#46456=CARTESIAN_POINT('Ctrl Pts',(-15.4737447016702,17.2124778330333,8.27052037800331));
#46457=CARTESIAN_POINT('Ctrl Pts',(-15.4813606859533,17.2072831911478,8.26040376244317));
#46458=CARTESIAN_POINT('Ctrl Pts',(-15.4889666118216,17.2021286574388,8.25024566530342));
#46459=CARTESIAN_POINT('Ctrl Pts',(-15.4965623340349,17.1970147003122,8.24004557550053));
#46460=CARTESIAN_POINT('Ctrl Pts',(-15.500311300197,17.1944906411533,8.23501119029698));
#46461=CARTESIAN_POINT('Ctrl Pts',(-15.5040577922121,17.1919764550271,8.22996656269615));
#46462=CARTESIAN_POINT('Ctrl Pts',(-15.5078015824525,17.1894723340246,8.2249119185801));
#46463=CARTESIAN_POINT('Ctrl Pts',(-15.5116430275708,17.1869028942903,8.21972542662477));
#46464=CARTESIAN_POINT('Ctrl Pts',(-15.5154790323891,17.184345787301,8.21453189406302));
#46465=CARTESIAN_POINT('Ctrl Pts',(-15.5193093970066,17.1818011536978,8.20933156444055));
#46466=CARTESIAN_POINT('Ctrl Pts',(-15.5316884204386,17.1735773728976,8.1925250698434));
#46467=CARTESIAN_POINT('Ctrl Pts',(-15.5440097288867,17.1654831610244,8.17564589662492));
#46468=CARTESIAN_POINT('Ctrl Pts',(-15.5562729465418,17.1575189151244,8.15869371101957));
#46469=CARTESIAN_POINT('Ctrl Pts',(-15.5589949305578,17.1557511449805,8.1549309482968));
#46470=CARTESIAN_POINT('Ctrl Pts',(-15.5617140559427,17.1539897665543,8.15116459316442));
#46471=CARTESIAN_POINT('Ctrl Pts',(-15.5644303175793,17.1522347879277,8.14739464025237));
#46472=CARTESIAN_POINT('Ctrl Pts',(-15.6242451117547,17.1135884057392,8.06437651179032));
#46473=CARTESIAN_POINT('Ctrl Pts',(-15.6826710263357,17.0780463286275,7.97961348456311));
#46474=CARTESIAN_POINT('Ctrl Pts',(-15.739650238122,17.045710385027,7.89304092775047));
#46475=CARTESIAN_POINT('Ctrl Pts',(-15.7410835124827,17.0448969957674,7.89086325238204));
#46476=CARTESIAN_POINT('Ctrl Pts',(-15.7425158711234,17.0440856365664,7.88868443145153));
#46477=CARTESIAN_POINT('Ctrl Pts',(-15.7439473131389,17.0432763090081,7.88650446391694));
#46478=CARTESIAN_POINT('Ctrl Pts',(-15.7994222388065,17.0119111641728,7.80202075054952));
#46479=CARTESIAN_POINT('Ctrl Pts',(-15.8535208498676,16.9835963942817,7.71581549314315));
#46480=CARTESIAN_POINT('Ctrl Pts',(-15.9061702459269,16.9584917518482,7.62779804765074));
#46481=CARTESIAN_POINT('Ctrl Pts',(-15.9112471153019,16.956070964529,7.61931071243075));
#46482=CARTESIAN_POINT('Ctrl Pts',(-15.9163104996267,16.9536800690656,7.61080650848719));
#46483=CARTESIAN_POINT('Ctrl Pts',(-15.9213603339769,16.9513192076422,7.60228535346611));
#46484=CARTESIAN_POINT('Ctrl Pts',(-15.970030829791,16.9285651353192,7.52015813680427));
#46485=CARTESIAN_POINT('Ctrl Pts',(-16.017443148426,16.908599481043,7.43645711852202));
#46486=CARTESIAN_POINT('Ctrl Pts',(-16.0635184121896,16.891616430166,7.35107816654769));
#46487=CARTESIAN_POINT('Ctrl Pts',(-16.0717041578125,16.88859921609,7.33590971551069));
#46488=CARTESIAN_POINT('Ctrl Pts',(-16.0798476086457,16.8856763078134,7.32068835327566));
#46489=CARTESIAN_POINT('Ctrl Pts',(-16.0879483499438,16.88284880545,7.30541341996439));
#46490=CARTESIAN_POINT('Ctrl Pts',(-16.1147581040427,16.873491063944,7.25486036674568));
#46491=CARTESIAN_POINT('Ctrl Pts',(-16.1410995143865,16.8651800504117,7.20371978428443));
#46492=CARTESIAN_POINT('Ctrl Pts',(-16.16695329123,16.8579688556867,7.15196177803975));
#46493=CARTESIAN_POINT('Ctrl Pts',(-16.1798695718559,16.854366217075,7.12610401120998));
#46494=CARTESIAN_POINT('Ctrl Pts',(-16.1926640919658,16.8510382409624,7.10009206849362));
#46495=CARTESIAN_POINT('Ctrl Pts',(-16.2053341041957,16.8479925917601,7.07392174227086));
#46496=CARTESIAN_POINT('Ctrl Pts',(-16.207248100535,16.847532500537,7.06996831999477));
#46497=CARTESIAN_POINT('Ctrl Pts',(-16.2091593148357,16.8470788585248,7.06601112699843));
#46498=CARTESIAN_POINT('Ctrl Pts',(-16.2110675167977,16.8466317303188,7.06205063036694));
#46499=CARTESIAN_POINT('Ctrl Pts',(-16.217000474151,16.8452415249684,7.04973670444064));
#46500=CARTESIAN_POINT('Ctrl Pts',(-16.2229080555058,16.8439135616734,7.0373828841659));
#46501=CARTESIAN_POINT('Ctrl Pts',(-16.2287732539462,16.8426519143645,7.02502447530824));
#46502=CARTESIAN_POINT('Ctrl Pts',(-16.2335040116055,16.8416342936086,7.0150564174576));
#46503=CARTESIAN_POINT('Ctrl Pts',(-16.2382100622439,16.8406591492381,7.00507941805309));
#46504=CARTESIAN_POINT('Ctrl Pts',(-16.2428892811382,16.8397271892998,6.99509766222573));
#46505=CARTESIAN_POINT('Ctrl Pts',(-16.2440113628681,16.839503704303,6.99270402642913));
#46506=CARTESIAN_POINT('Ctrl Pts',(-16.24513203341,16.8392826651952,6.9903098519872));
#46507=CARTESIAN_POINT('Ctrl Pts',(-16.2462513124443,16.8390640709198,6.98791509430535));
#46508=CARTESIAN_POINT('Ctrl Pts',(-16.2578249331307,16.8368037523125,6.96315271048787));
#46509=CARTESIAN_POINT('Ctrl Pts',(-16.2692417829089,16.8348066794356,6.93834479185663));
#46510=CARTESIAN_POINT('Ctrl Pts',(-16.2805015918988,16.8330742819549,6.91349131223052));
#46511=CARTESIAN_POINT('Ctrl Pts',(-16.3030212098786,16.8296094869936,6.86378435297832));
#46512=CARTESIAN_POINT('Ctrl Pts',(-16.3249126668437,16.8272033934617,6.81389514748906));
#46513=CARTESIAN_POINT('Ctrl Pts',(-16.3461718488325,16.8258727062833,6.76382298919644));
#46514=CARTESIAN_POINT('Ctrl Pts',(-16.3585128827858,16.8251002374433,6.73475591568759));
#46515=CARTESIAN_POINT('Ctrl Pts',(-16.3706406252239,16.8246907899988,6.70562711760921));
#46516=CARTESIAN_POINT('Ctrl Pts',(-16.3825543362793,16.8246474124682,6.67643650814875));
#46517=CARTESIAN_POINT('Ctrl Pts',(-16.4116867405569,16.8245413420967,6.60505718461495));
#46518=CARTESIAN_POINT('Ctrl Pts',(-16.4395395922015,16.8266234509508,6.53330838124095));
#46519=CARTESIAN_POINT('Ctrl Pts',(-16.4660876043868,16.830974861643,6.46118444796423));
#46520=CARTESIAN_POINT('Ctrl Pts',(-16.4793737111767,16.8331525503806,6.42508960692901));
#46521=CARTESIAN_POINT('Ctrl Pts',(-16.4923325381101,16.835899902222,6.38890068074229));
#46522=CARTESIAN_POINT('Ctrl Pts',(-16.5049608875163,16.8392270469745,6.35261705451585));
#46523=CARTESIAN_POINT('Ctrl Pts',(-16.5278855658781,16.8452669276318,6.28675013602257));
#46524=CARTESIAN_POINT('Ctrl Pts',(-16.5497215555428,16.8532163974352,6.22057127274915));
#46525=CARTESIAN_POINT('Ctrl Pts',(-16.5704362939606,16.8631707652677,6.15407282388274));
#46526=CARTESIAN_POINT('Ctrl Pts',(-16.5839479628594,16.8696637327162,6.11069766725516));
#46527=CARTESIAN_POINT('Ctrl Pts',(-16.5969825403869,16.8770097708918,6.06718658073939));
#46528=CARTESIAN_POINT('Ctrl Pts',(-16.6095299784033,16.885238026301,6.0235372341579));
#46529=CARTESIAN_POINT('Ctrl Pts',(-16.6118991067048,16.8867916337176,6.01529563916504));
#46530=CARTESIAN_POINT('Ctrl Pts',(-16.614250835039,16.8883767774259,6.00704910784024));
#46531=CARTESIAN_POINT('Ctrl Pts',(-16.6165850775924,16.8899936994925,5.99879762134841));
#46532=CARTESIAN_POINT('Ctrl Pts',(-16.6181662314661,16.8910889595311,5.99320828368015));
#46533=CARTESIAN_POINT('Ctrl Pts',(-16.6197392455601,16.8921986796151,5.98761712958495));
#46534=CARTESIAN_POINT('Ctrl Pts',(-16.6213041889455,16.8933229998439,5.98202381843932));
#46535=CARTESIAN_POINT('Ctrl Pts',(-16.6233758056449,16.894811335194,5.97461959098788));
#46536=CARTESIAN_POINT('Ctrl Pts',(-16.6254340295377,16.8963258504435,5.96720881741333));
#46537=CARTESIAN_POINT('Ctrl Pts',(-16.6274776180581,16.897865794274,5.95979582904516));
#46538=CARTESIAN_POINT('Ctrl Pts',(-16.6292570586422,16.8992066897243,5.95334102064287));
#46539=CARTESIAN_POINT('Ctrl Pts',(-16.631025572609,16.9005669866222,5.94688392154869));
#46540=CARTESIAN_POINT('Ctrl Pts',(-16.6327818099178,16.9019457784013,5.94042932478974));
#46541=CARTESIAN_POINT('Ctrl Pts',(-16.6345661535421,16.9033466359665,5.93387143052549));
#46542=CARTESIAN_POINT('Ctrl Pts',(-16.6363372586855,16.9047660921804,5.92731827230297));
#46543=CARTESIAN_POINT('Ctrl Pts',(-16.6380947701799,16.9062037955367,5.92077133421867));
#46544=CARTESIAN_POINT('Ctrl Pts',(-16.6437740492813,16.9108496363473,5.89961534817929));
#46545=CARTESIAN_POINT('Ctrl Pts',(-16.6493146604464,16.9156889677414,5.87851181846174));
#46546=CARTESIAN_POINT('Ctrl Pts',(-16.6547182018872,16.9207206527441,5.85746057140922));
#46547=CARTESIAN_POINT('Ctrl Pts',(-16.6559507078088,16.9218683410943,5.85265894511777));
#46548=CARTESIAN_POINT('Ctrl Pts',(-16.6571760846858,16.9230260331474,5.8478600378164));
#46549=CARTESIAN_POINT('Ctrl Pts',(-16.6583943491292,16.9241937195169,5.8430638481694));
#46550=CARTESIAN_POINT('Ctrl Pts',(-16.6711840856364,16.9364524709472,5.79271188874387));
#46551=CARTESIAN_POINT('Ctrl Pts',(-16.6831889826383,16.949814692948,5.74265997630306));
#46552=CARTESIAN_POINT('Ctrl Pts',(-16.6944254022008,16.9642745561676,5.69290880673133));
#46553=CARTESIAN_POINT('Ctrl Pts',(-16.7062399084323,16.979478344453,5.64059805955267));
#46554=CARTESIAN_POINT('Ctrl Pts',(-16.7172058453786,16.9958937260294,5.58861931331693));
#46555=CARTESIAN_POINT('Ctrl Pts',(-16.7273360612814,17.013524763337,5.53697595623463));
#46556=CARTESIAN_POINT('Ctrl Pts',(-16.7383690919225,17.0327270959147,5.48073009271422));
#46557=CARTESIAN_POINT('Ctrl Pts',(-16.7484107574535,17.0533714712242,5.42488213752166));
#46558=CARTESIAN_POINT('Ctrl Pts',(-16.7574767467459,17.0754640501639,5.36943744760249));
#46559=CARTESIAN_POINT('Ctrl Pts',(-16.7646517241534,17.0929484911502,5.32555758135657));
#46560=CARTESIAN_POINT('Ctrl Pts',(-16.7712156377876,17.1113397698573,5.28193022356205));
#46561=CARTESIAN_POINT('Ctrl Pts',(-16.7771711177175,17.1306506982287,5.23856061432427));
#46562=CARTESIAN_POINT('Ctrl Pts',(-16.7857032969204,17.1583166971708,5.17642670029277));
#46563=CARTESIAN_POINT('Ctrl Pts',(-16.7929878087474,17.1878678868144,5.11482118509071));
#46564=CARTESIAN_POINT('Ctrl Pts',(-16.7990319439269,17.2193417178198,5.05376028262675));
#46565=CARTESIAN_POINT('Ctrl Pts',(-16.8025373454865,17.2375955147675,5.0183469478207));
#46566=CARTESIAN_POINT('Ctrl Pts',(-16.8056249923219,17.2564970784941,4.9831170877998));
#46567=CARTESIAN_POINT('Ctrl Pts',(-16.8082939481964,17.2760584841819,4.94807520570957));
#46568=CARTESIAN_POINT('Ctrl Pts',(-16.8095429904173,17.2852130085553,4.93167598733007));
#46569=CARTESIAN_POINT('Ctrl Pts',(-16.8107003335015,17.2945118620255,4.91531818116869));
#46570=CARTESIAN_POINT('Ctrl Pts',(-16.8117658798418,17.3039556942957,4.89900304955538));
#46571=CARTESIAN_POINT('Ctrl Pts',(-16.8122510098167,17.3082553534842,4.89157497337359));
#46572=CARTESIAN_POINT('Ctrl Pts',(-16.8127172005031,17.3125869477479,4.88415283348946));
#46573=CARTESIAN_POINT('Ctrl Pts',(-16.8131642431758,17.3169475780613,4.87674150730954));
#46574=CARTESIAN_POINT('Ctrl Pts',(-16.8138787099376,17.3239167682738,4.86489667338347));
#46575=CARTESIAN_POINT('Ctrl Pts',(-16.8145449498413,17.3309677138809,4.85306683516652));
#46576=CARTESIAN_POINT('Ctrl Pts',(-16.8151607441959,17.3380741191068,4.84129616134881));
#46577=CARTESIAN_POINT('Ctrl Pts',(-16.8154888696785,17.3418607609082,4.83502416811295));
#46578=CARTESIAN_POINT('Ctrl Pts',(-16.815802859543,17.345665122089,4.82876566522662));
#46579=CARTESIAN_POINT('Ctrl Pts',(-16.8161026019274,17.3494855415575,4.82252343039461));
#46580=CARTESIAN_POINT('Ctrl Pts',(-16.8163653872281,17.3528349179926,4.8170508391198));
#46581=CARTESIAN_POINT('Ctrl Pts',(-16.8166173448659,17.3561974209022,4.81158930335026));
#46582=CARTESIAN_POINT('Ctrl Pts',(-16.8168585431549,17.3595730738688,4.80613867917317));
#46583=CARTESIAN_POINT('Ctrl Pts',(-16.8177333839499,17.3718167715219,4.78636893533259));
#46584=CARTESIAN_POINT('Ctrl Pts',(-16.8184664384501,17.3842314930117,4.76674627660528));
#46585=CARTESIAN_POINT('Ctrl Pts',(-16.8190606453201,17.3968154028595,4.74726906352365));
#46586=CARTESIAN_POINT('Ctrl Pts',(-16.8198692059289,17.4139388228674,4.72076565526566));
#46587=CARTESIAN_POINT('Ctrl Pts',(-16.82042126738,17.4313747980671,4.69453101225618));
#46588=CARTESIAN_POINT('Ctrl Pts',(-16.8207228409782,17.4491203250095,4.66856224559516));
#46589=CARTESIAN_POINT('Ctrl Pts',(-16.8215560496239,17.4981489089408,4.59681391938496));
#46590=CARTESIAN_POINT('Ctrl Pts',(-16.820480330705,17.5495354930376,4.52709118335943));
#46591=CARTESIAN_POINT('Ctrl Pts',(-16.8176176508208,17.6032206644751,4.45933945087101));
#46592=CARTESIAN_POINT('Ctrl Pts',(-16.8168851937344,17.6169567739388,4.44200421305957));
#46593=CARTESIAN_POINT('Ctrl Pts',(-16.8160356997886,17.6308433811587,4.42479803834067));
#46594=CARTESIAN_POINT('Ctrl Pts',(-16.8150705444703,17.6448803145444,4.4077206653306));
#46595=CARTESIAN_POINT('Ctrl Pts',(-16.8108707290189,17.7059611878581,4.3334095014392));
#46596=CARTESIAN_POINT('Ctrl Pts',(-16.804484970729,17.7698819222335,4.26153195563804));
#46597=CARTESIAN_POINT('Ctrl Pts',(-16.7960260709805,17.836624529602,4.19206773199594));
#46598=CARTESIAN_POINT('Ctrl Pts',(-16.7949435260831,17.845166050508,4.18317790671273));
#46599=CARTESIAN_POINT('Ctrl Pts',(-16.7938269626664,17.8537538688681,4.1743276718339));
#46600=CARTESIAN_POINT('Ctrl Pts',(-16.7926765400346,17.8623880506822,4.16551706644754));
#46601=CARTESIAN_POINT('Ctrl Pts',(-16.7882774357282,17.8954043225738,4.13182616796633));
#46602=CARTESIAN_POINT('Ctrl Pts',(-16.7833836442642,17.9290978128492,4.09871424594278));
#46603=CARTESIAN_POINT('Ctrl Pts',(-16.7780042088693,17.9634716718842,4.06618342561398));
#46604=CARTESIAN_POINT('Ctrl Pts',(-16.7771839813685,17.9687128138295,4.06122330034071));
#46605=CARTESIAN_POINT('Ctrl Pts',(-16.7763524570089,17.9739697823373,4.05627669175243));
#46606=CARTESIAN_POINT('Ctrl Pts',(-16.7755096616605,17.9792425973972,4.05134361419153));
#46607=CARTESIAN_POINT('Ctrl Pts',(-16.774606322161,17.9848941973095,4.04605615760648));
#46608=CARTESIAN_POINT('Ctrl Pts',(-16.7736900416366,17.9905639652448,4.04078427420014));
#46609=CARTESIAN_POINT('Ctrl Pts',(-16.772760844743,17.9962519732155,4.03552793535613));
#46610=CARTESIAN_POINT('Ctrl Pts',(-16.7709635554923,18.0072539423928,4.02536091761548));
#46611=CARTESIAN_POINT('Ctrl Pts',(-16.7691170692686,18.0183290120654,4.0152478267625));
#46612=CARTESIAN_POINT('Ctrl Pts',(-16.7672278724432,18.0294413032003,4.00522090599292));
#46613=CARTESIAN_POINT('Ctrl Pts',(-16.7666499510457,18.0328406476918,4.00215358553933));
#46614=CARTESIAN_POINT('Ctrl Pts',(-16.7660679300489,18.0362441268367,3.99909371537179));
#46615=CARTESIAN_POINT('Ctrl Pts',(-16.7654818289922,18.0396517394221,3.99604126463338));
#46616=CARTESIAN_POINT('Ctrl Pts',(-16.7622326330158,18.0585426814793,3.97911925000119));
#46617=CARTESIAN_POINT('Ctrl Pts',(-16.758857941205,18.0775606054575,3.96242577932828));
#46618=CARTESIAN_POINT('Ctrl Pts',(-16.7553616195243,18.0967033857874,3.94595641211867));
#46619=CARTESIAN_POINT('Ctrl Pts',(-16.7550997309887,18.0981372569145,3.94472279037113));
#46620=CARTESIAN_POINT('Ctrl Pts',(-16.7548371621615,18.0995718268212,3.94349042298232));
#46621=CARTESIAN_POINT('Ctrl Pts',(-16.7545739143653,18.1010070948678,3.94225930848775));
#46622=CARTESIAN_POINT('Ctrl Pts',(-16.7394630496698,18.1833938862189,3.87159127318213));
#46623=CARTESIAN_POINT('Ctrl Pts',(-16.7221122255081,18.2680851147759,3.80505793177941));
#46624=CARTESIAN_POINT('Ctrl Pts',(-16.7027490566819,18.3549810994009,3.74243609542314));
#46625=CARTESIAN_POINT('Ctrl Pts',(-16.7011252984973,18.3622680299395,3.73718474838229));
#46626=CARTESIAN_POINT('Ctrl Pts',(-16.6994873679414,18.3695704916422,3.73196094643881));
#46627=CARTESIAN_POINT('Ctrl Pts',(-16.6978353988412,18.3768884221525,3.72676456101778));
#46628=CARTESIAN_POINT('Ctrl Pts',(-16.6797877865089,18.4568361481147,3.66999452240542));
#46629=CARTESIAN_POINT('Ctrl Pts',(-16.660063932005,18.5386304234911,3.61649763813193));
#46630=CARTESIAN_POINT('Ctrl Pts',(-16.6387816406185,18.6222388096108,3.56618605682596));
#46631=CARTESIAN_POINT('Ctrl Pts',(-16.6343665117779,18.6395838308854,3.55574864153051));
#46632=CARTESIAN_POINT('Ctrl Pts',(-16.6298845307761,18.6570058438323,3.54544919702397));
#46633=CARTESIAN_POINT('Ctrl Pts',(-16.6253365723563,18.6745052073658,3.53528656580386));
#46634=CARTESIAN_POINT('Ctrl Pts',(-16.6120568488463,18.725602136554,3.50561238669301));
#46635=CARTESIAN_POINT('Ctrl Pts',(-16.5982133624414,18.7773596411757,3.47710648804274));
#46636=CARTESIAN_POINT('Ctrl Pts',(-16.5838189315666,18.8297952185675,3.4497540158));
#46637=CARTESIAN_POINT('Ctrl Pts',(-16.5772052155726,18.8538874539513,3.43718655240246));
#46638=CARTESIAN_POINT('Ctrl Pts',(-16.5704722809959,18.8781329439034,3.42485779907269));
#46639=CARTESIAN_POINT('Ctrl Pts',(-16.5636289474838,18.9025052790382,3.4127811710977));
#46640=CARTESIAN_POINT('Ctrl Pts',(-16.5630150703628,18.9046915847181,3.41169784444109));
#46641=CARTESIAN_POINT('Ctrl Pts',(-16.562400271962,18.9068790266346,3.41061649162404));
#46642=CARTESIAN_POINT('Ctrl Pts',(-16.5617845583766,18.9090675860316,3.40953712293799));
#46643=CARTESIAN_POINT('Ctrl Pts',(-16.5543053966033,18.9356523328526,3.39642587574771));
#46644=CARTESIAN_POINT('Ctrl Pts',(-16.5467123462032,18.9623271295586,3.3836439251165));
#46645=CARTESIAN_POINT('Ctrl Pts',(-16.5390081804392,18.9890932965675,3.37118496984572));
#46646=CARTESIAN_POINT('Ctrl Pts',(-16.5196180850813,19.0564592576034,3.33982786536966));
#46647=CARTESIAN_POINT('Ctrl Pts',(-16.4995268262444,19.1244028255936,3.31051116810786));
#46648=CARTESIAN_POINT('Ctrl Pts',(-16.4787633867405,19.1929521614537,3.28316660603189));
#46649=CARTESIAN_POINT('Ctrl Pts',(-16.4665990140822,19.2331121583907,3.26714664733446));
#46650=CARTESIAN_POINT('Ctrl Pts',(-16.4542052664158,19.2734744522462,3.25180765814332));
#46651=CARTESIAN_POINT('Ctrl Pts',(-16.4415901717203,19.3140374655582,3.23713906453767));
#46652=CARTESIAN_POINT('Ctrl Pts',(-16.4234126569237,19.372486077516,3.21600259400401));
#46653=CARTESIAN_POINT('Ctrl Pts',(-16.4047752775749,19.4313515251799,3.19625859049243));
#46654=CARTESIAN_POINT('Ctrl Pts',(-16.3856913105911,19.4906335657926,3.17789716423366));
#46655=CARTESIAN_POINT('',(2.06506260776231,19.4906334205523,-16.5627719180504));
#46656=CARTESIAN_POINT('Origin',(6.61325378140121E-15,19.4906334205523,
8.67361737988404E-16));
#46657=CARTESIAN_POINT('',(6.78574855947105,19.4906334205522,-15.2493774847033));
#46658=CARTESIAN_POINT('Ctrl Pts',(2.06506260776273,19.4906334205533,-16.5627719180497));
#46659=CARTESIAN_POINT('Ctrl Pts',(2.41742332821393,19.349939283335,-16.5720080472377));
#46660=CARTESIAN_POINT('Ctrl Pts',(2.76269377024947,19.2344262533423,-16.5621715122885));
#46661=CARTESIAN_POINT('Ctrl Pts',(3.44112953030319,19.0724697614237,-16.495689659873));
#46662=CARTESIAN_POINT('Ctrl Pts',(3.75758071471907,19.0223948272706,-16.4459328577175));
#46663=CARTESIAN_POINT('Ctrl Pts',(4.22465776181844,18.9889208004819,-16.3426280057139));
#46664=CARTESIAN_POINT('Ctrl Pts',(4.37312530932789,18.984322683773,-16.3053159474107));
#46665=CARTESIAN_POINT('Ctrl Pts',(4.59196989806894,18.9864292907932,-16.2436668872455));
#46666=CARTESIAN_POINT('Ctrl Pts',(4.66297798251051,18.9885240740547,-16.2226078396245));
#46667=CARTESIAN_POINT('Ctrl Pts',(4.76322511787825,18.9934497272694,-16.1913920375261));
#46668=CARTESIAN_POINT('Ctrl Pts',(4.7927075198343,18.9951414505049,-16.1820279768777));
#46669=CARTESIAN_POINT('Ctrl Pts',(4.83538292817332,18.9979409897723,-16.1682080344538));
#46670=CARTESIAN_POINT('Ctrl Pts',(4.84862882894517,18.9988591807016,-16.1638812207154));
#46671=CARTESIAN_POINT('Ctrl Pts',(4.91979031300025,19.0040561695104,-16.1404359378585));
#46672=CARTESIAN_POINT('Ctrl Pts',(4.97741481102364,19.0092070140339,-16.1207366039373));
#46673=CARTESIAN_POINT('Ctrl Pts',(5.11930956255435,19.0241842792193,-16.0704800244993));
#46674=CARTESIAN_POINT('Ctrl Pts',(5.2031675870547,19.0350630426818,-16.0392332038417));
#46675=CARTESIAN_POINT('Ctrl Pts',(5.46110025027662,19.074570039631,-15.9384495833863));
#46676=CARTESIAN_POINT('Ctrl Pts',(5.63207967254321,19.1095004500619,-15.8648985157062));
#46677=CARTESIAN_POINT('Ctrl Pts',(6.14663187861032,19.2388854970279,-15.6241814045855));
#46678=CARTESIAN_POINT('Ctrl Pts',(6.46898077889003,19.3543537790241,-15.44627066688));
#46679=CARTESIAN_POINT('Ctrl Pts',(6.78574855947051,19.4906334205529,-15.2493774847029));
#46680=CARTESIAN_POINT('',(16.6906704142672,19.4906334305655,0.10686064282603));
#46681=CARTESIAN_POINT('Origin',(6.61325378140121E-15,19.4906334205523,
8.67361737988404E-16));
#46682=CARTESIAN_POINT('',(12.3247145833779,19.4906334205523,11.2557233273388));
#46683=CARTESIAN_POINT('Ctrl Pts',(16.6906704676692,19.4906334505918,0.106860643167889));
#46684=CARTESIAN_POINT('Ctrl Pts',(16.7554332564921,19.3173865856866,0.139157039459681));
#46685=CARTESIAN_POINT('Ctrl Pts',(16.8193252940415,19.1461031307759,0.178612921117866));
#46686=CARTESIAN_POINT('Ctrl Pts',(16.8822218893148,18.9767355755773,0.225223411409203));
#46687=CARTESIAN_POINT('Ctrl Pts',(16.8826470664552,18.9755906612543,0.225538495475169));
#46688=CARTESIAN_POINT('Ctrl Pts',(16.8830721981114,18.9744458344816,0.225853906539962));
#46689=CARTESIAN_POINT('Ctrl Pts',(16.8834972842449,18.9733010952449,0.226169644596096));
#46690=CARTESIAN_POINT('Ctrl Pts',(16.9459553307026,18.8051041798494,0.272561141813467));
#46691=CARTESIAN_POINT('Ctrl Pts',(17.007431128011,18.6387971651158,0.32601057224118));
#46692=CARTESIAN_POINT('Ctrl Pts',(17.0677324304234,18.474366967947,0.386698765732942));
#46693=CARTESIAN_POINT('Ctrl Pts',(17.0738247090014,18.4577544815209,0.392830132160528));
#46694=CARTESIAN_POINT('Ctrl Pts',(17.0799049883242,18.4411611794587,0.3990355131978));
#46695=CARTESIAN_POINT('Ctrl Pts',(17.0859730702553,18.424587051854,0.405315079357435));
#46696=CARTESIAN_POINT('Ctrl Pts',(17.110140279184,18.3585776589057,0.430324561609761));
#46697=CARTESIAN_POINT('Ctrl Pts',(17.134113158127,18.2928728040555,0.456513147980813));
#46698=CARTESIAN_POINT('Ctrl Pts',(17.1578750798263,18.2274735574929,0.483903109577319));
#46699=CARTESIAN_POINT('Ctrl Pts',(17.1666728977386,18.2032595789208,0.494044204131883));
#46700=CARTESIAN_POINT('Ctrl Pts',(17.1754417870569,18.1790875151221,0.504350093439007));
#46701=CARTESIAN_POINT('Ctrl Pts',(17.1841808989709,18.1549574369282,0.514821961053957));
#46702=CARTESIAN_POINT('Ctrl Pts',(17.1902067224447,18.1383191797416,0.522042560390655));
#46703=CARTESIAN_POINT('Ctrl Pts',(17.1962183712914,18.1217008914811,0.529342119502282));
#46704=CARTESIAN_POINT('Ctrl Pts',(17.2022155260639,18.1051026122299,0.536721137196537));
#46705=CARTESIAN_POINT('Ctrl Pts',(17.209562870631,18.0847674230431,0.545761455084535));
#46706=CARTESIAN_POINT('Ctrl Pts',(17.2168884661567,18.0644622546451,0.554920988090242));
#46707=CARTESIAN_POINT('Ctrl Pts',(17.2241917200914,18.0441871936411,0.564200691556757));
#46708=CARTESIAN_POINT('Ctrl Pts',(17.2269375825861,18.0365642176241,0.567689655508839));
#46709=CARTESIAN_POINT('Ctrl Pts',(17.229680508348,18.0289448827969,0.571195887923344));
#46710=CARTESIAN_POINT('Ctrl Pts',(17.2324204715755,18.0213291760418,0.574719454032397));
#46711=CARTESIAN_POINT('Ctrl Pts',(17.2369680718224,18.0086891560694,0.580567623798449));
#46712=CARTESIAN_POINT('Ctrl Pts',(17.2415029342496,17.9960718361261,0.586457709712012));
#46713=CARTESIAN_POINT('Ctrl Pts',(17.2460245379011,17.9834783465572,0.592389106278812));
#46714=CARTESIAN_POINT('Ctrl Pts',(17.2573836593269,17.9518411248512,0.60728989348185));
#46715=CARTESIAN_POINT('Ctrl Pts',(17.2686612397977,17.9203483203527,0.622454523538607));
#46716=CARTESIAN_POINT('Ctrl Pts',(17.2798485678208,17.8890190033201,0.637873157575821));
#46717=CARTESIAN_POINT('Ctrl Pts',(17.3257517832463,17.7604703109143,0.701138029966847));
#46718=CARTESIAN_POINT('Ctrl Pts',(17.3701969574651,17.6345118072375,0.768739601039109));
#46719=CARTESIAN_POINT('Ctrl Pts',(17.4130560019887,17.5110962940719,0.840715969915629));
#46720=CARTESIAN_POINT('Ctrl Pts',(17.4284574345146,17.4667468289871,0.866580736641848));
#46721=CARTESIAN_POINT('Ctrl Pts',(17.4436530655792,17.4227281768419,0.893011286951045));
#46722=CARTESIAN_POINT('Ctrl Pts',(17.4586365955835,17.3790389121479,0.920008840824794));
#46723=CARTESIAN_POINT('Ctrl Pts',(17.4955111628831,17.271519340273,0.986450001016147));
#46724=CARTESIAN_POINT('Ctrl Pts',(17.5311020607058,17.1659947086958,1.05632454162672));
#46725=CARTESIAN_POINT('Ctrl Pts',(17.5652760758296,17.0624873851863,1.12972562705538));
#46726=CARTESIAN_POINT('Ctrl Pts',(17.5834046144217,17.0075791017433,1.168663235208));
#46727=CARTESIAN_POINT('Ctrl Pts',(17.6011335450642,16.953240328626,1.20859594981807));
#46728=CARTESIAN_POINT('Ctrl Pts',(17.618442770531,16.8994741998413,1.24953825060211));
#46729=CARTESIAN_POINT('Ctrl Pts',(17.6470216890427,16.810702012075,1.31713727056023));
#46730=CARTESIAN_POINT('Ctrl Pts',(17.6744578871136,16.7234901850469,1.38748683629434));
#46731=CARTESIAN_POINT('Ctrl Pts',(17.7006253081176,16.637886306578,1.46071191763152));
#46732=CARTESIAN_POINT('Ctrl Pts',(17.7199827879829,16.5745604116187,1.51488053583065));
#46733=CARTESIAN_POINT('Ctrl Pts',(17.738646309133,16.5121137043897,1.5706217131087));
#46734=CARTESIAN_POINT('Ctrl Pts',(17.7565615957351,16.4505703505189,1.62799550309415));
#46735=CARTESIAN_POINT('Ctrl Pts',(17.7580891880836,16.4453227003659,1.63288762480768));
#46736=CARTESIAN_POINT('Ctrl Pts',(17.7596113167566,16.4400816395194,1.63779165267672));
#46737=CARTESIAN_POINT('Ctrl Pts',(17.7611279404093,16.4348471898327,1.64270763524448));
#46738=CARTESIAN_POINT('Ctrl Pts',(17.770039202122,16.4040910091567,1.67159259108592));
#46739=CARTESIAN_POINT('Ctrl Pts',(17.7787607516293,16.3735624005947,1.70088932840607));
#46740=CARTESIAN_POINT('Ctrl Pts',(17.7872844554273,16.3432652299643,1.73060714320661));
#46741=CARTESIAN_POINT('Ctrl Pts',(17.7879926300817,16.340748050948,1.73307618761802));
#46742=CARTESIAN_POINT('Ctrl Pts',(17.7886994386785,16.3382324698041,1.73554813918163));
#46743=CARTESIAN_POINT('Ctrl Pts',(17.7894048762293,16.335718489019,1.73802300370958));
#46744=CARTESIAN_POINT('Ctrl Pts',(17.7936629409595,16.3205439453602,1.75296143921885));
#46745=CARTESIAN_POINT('Ctrl Pts',(17.7978713134397,16.3054267654372,1.7680069588093));
#46746=CARTESIAN_POINT('Ctrl Pts',(17.8020281525554,16.2903702106543,1.78315803810895));
#46747=CARTESIAN_POINT('Ctrl Pts',(17.8023601028744,16.2891678479878,1.78436794916567));
#46748=CARTESIAN_POINT('Ctrl Pts',(17.8026917396659,16.2879658150709,1.78557859340076));
#46749=CARTESIAN_POINT('Ctrl Pts',(17.8030230558681,16.2867641364131,1.7867899461418));
#46750=CARTESIAN_POINT('Ctrl Pts',(17.8075032704746,16.2705144684552,1.80317043163647));
#46751=CARTESIAN_POINT('Ctrl Pts',(17.8119262462366,16.2543245055393,1.81968570898484));
#46752=CARTESIAN_POINT('Ctrl Pts',(17.8162742104404,16.2382558357076,1.83627399178503));
#46753=CARTESIAN_POINT('Ctrl Pts',(17.8162953962977,16.238177539629,1.8363548197259));
#46754=CARTESIAN_POINT('Ctrl Pts',(17.816316580384,16.2380992463939,1.83643564943822));
#46755=CARTESIAN_POINT('Ctrl Pts',(17.8163377626971,16.2380209560091,1.8365164809153));
#46756=CARTESIAN_POINT('Ctrl Pts',(17.8350686489185,16.168791109381,1.90799333949187));
#46757=CARTESIAN_POINT('Ctrl Pts',(17.8524671078719,16.1015998621785,1.98103401675485));
#46758=CARTESIAN_POINT('Ctrl Pts',(17.8684852965537,16.0364294729093,2.05563176347801));
#46759=CARTESIAN_POINT('Ctrl Pts',(17.8821901849448,15.9806708019961,2.11945632025969));
#46760=CARTESIAN_POINT('Ctrl Pts',(17.8948867344368,15.9263883328354,2.18441855727403));
#46761=CARTESIAN_POINT('Ctrl Pts',(17.9065346466881,15.8735871519442,2.25052542310617));
#46762=CARTESIAN_POINT('Ctrl Pts',(17.9220146524199,15.8034146982716,2.33838105250214));
#46763=CARTESIAN_POINT('Ctrl Pts',(17.9356436345352,15.735856243357,2.42825707097301));
#46764=CARTESIAN_POINT('Ctrl Pts',(17.9473244533597,15.6709250091733,2.52017572255856));
#46765=CARTESIAN_POINT('Ctrl Pts',(17.9547172544272,15.6298299708379,2.57835112239702));
#46766=CARTESIAN_POINT('Ctrl Pts',(17.9613282438511,15.5897895312754,2.6373462328043));
#46767=CARTESIAN_POINT('Ctrl Pts',(17.9671255285473,15.5508170878235,2.69717341994217));
#46768=CARTESIAN_POINT('Ctrl Pts',(17.9693245013501,15.5360344184021,2.71986651925895));
#46769=CARTESIAN_POINT('Ctrl Pts',(17.9714064145044,15.5214053613257,2.74267934384877));
#46770=CARTESIAN_POINT('Ctrl Pts',(17.9733695519132,15.5069305580775,2.7656125562293));
#46771=CARTESIAN_POINT('Ctrl Pts',(17.9780829256348,15.4721774343545,2.82067380670434));
#46772=CARTESIAN_POINT('Ctrl Pts',(17.9821116985938,15.4383134582655,2.87642898490496));
#46773=CARTESIAN_POINT('Ctrl Pts',(17.9854278507014,15.4053528371821,2.93289108280594));
#46774=CARTESIAN_POINT('Ctrl Pts',(17.9871214137631,15.3885198064447,2.96172634737995));
#46775=CARTESIAN_POINT('Ctrl Pts',(17.9886290074013,15.3719225948283,2.99074613159763));
#46776=CARTESIAN_POINT('Ctrl Pts',(17.9899468566142,15.3555631122618,3.01995223286669));
#46777=CARTESIAN_POINT('Ctrl Pts',(17.9922842524111,15.3265472086113,3.07175346906009));
#46778=CARTESIAN_POINT('Ctrl Pts',(17.9940248324192,15.2982790927692,3.12414077166325));
#46779=CARTESIAN_POINT('Ctrl Pts',(17.9951437711287,15.2707738254319,3.17712733298565));
#46780=CARTESIAN_POINT('Ctrl Pts',(17.9958860934773,15.2525263785625,3.21227948950411));
#46781=CARTESIAN_POINT('Ctrl Pts',(17.9963548145827,15.2346143329278,3.24769611805471));
#46782=CARTESIAN_POINT('Ctrl Pts',(17.9965424157188,15.217043464621,3.28337941396034));
#46783=CARTESIAN_POINT('Ctrl Pts',(17.9965759220781,15.2139052329469,3.28975260209714));
#46784=CARTESIAN_POINT('Ctrl Pts',(17.9966004535718,15.2107778316002,3.29613443020691));
#46785=CARTESIAN_POINT('Ctrl Pts',(17.996615963183,15.2076613246323,3.30252485909978));
#46786=CARTESIAN_POINT('Ctrl Pts',(17.9966671369206,15.1973784549953,3.32360998674614));
#46787=CARTESIAN_POINT('Ctrl Pts',(17.9966201386314,15.1872142054475,3.34478847787987));
#46788=CARTESIAN_POINT('Ctrl Pts',(17.996473262686,15.1771697287181,3.36606132847237));
#46789=CARTESIAN_POINT('Ctrl Pts',(17.9963998247132,15.1721474903534,3.37669775376862));
#46790=CARTESIAN_POINT('Ctrl Pts',(17.996301417629,15.1671551934491,3.38735776816199));
#46791=CARTESIAN_POINT('Ctrl Pts',(17.9961778220592,15.1621929880374,3.39804150044135));
#46792=CARTESIAN_POINT('Ctrl Pts',(17.9960987266352,15.1590174070552,3.404878592869));
#46793=CARTESIAN_POINT('Ctrl Pts',(17.9960093131326,15.1558540955849,3.41172551884406));
#46794=CARTESIAN_POINT('Ctrl Pts',(17.9959095368297,15.1527034975434,3.41858143252991));
#46795=CARTESIAN_POINT('Ctrl Pts',(17.9958534013443,15.1509309288511,3.42243866147377));
#46796=CARTESIAN_POINT('Ctrl Pts',(17.9957940138343,15.1491632483792,3.42629685157856));
#46797=CARTESIAN_POINT('Ctrl Pts',(17.9957313769541,15.1474005156812,3.43015585664521));
#46798=CARTESIAN_POINT('Ctrl Pts',(17.9950561047956,15.1283969460774,3.47175880159095));
#46799=CARTESIAN_POINT('Ctrl Pts',(17.9940028406359,15.1099587858533,3.51347756260468));
#46800=CARTESIAN_POINT('Ctrl Pts',(17.9925715579667,15.0920785076305,3.55530998373131));
#46801=CARTESIAN_POINT('Ctrl Pts',(17.9910529348596,15.0731071302408,3.59969512351652));
#46802=CARTESIAN_POINT('Ctrl Pts',(17.9891089067087,15.0547634660304,3.64420815159584));
#46803=CARTESIAN_POINT('Ctrl Pts',(17.9867385000125,15.0370405505643,3.68884690964006));
#46804=CARTESIAN_POINT('Ctrl Pts',(17.9842315841771,15.0182969917055,3.73605636512686));
#46805=CARTESIAN_POINT('Ctrl Pts',(17.98124774844,15.0002478006414,3.78340641977283));
#46806=CARTESIAN_POINT('Ctrl Pts',(17.9777857836728,14.9828847689785,3.83089464581435));
#46807=CARTESIAN_POINT('Ctrl Pts',(17.9710601427838,14.9491531964285,3.92315114646949));
#46808=CARTESIAN_POINT('Ctrl Pts',(17.9625299443818,14.9180114764903,4.01592917751899));
#46809=CARTESIAN_POINT('Ctrl Pts',(17.9521757527204,14.8894208769911,4.10921510859279));
#46810=CARTESIAN_POINT('Ctrl Pts',(17.9482813090824,14.8786673114816,4.14430203885945));
#46811=CARTESIAN_POINT('Ctrl Pts',(17.9441288257152,14.8682746592604,4.1794608228901));
#46812=CARTESIAN_POINT('Ctrl Pts',(17.939716716368,14.8582419102149,4.21469093389021));
#46813=CARTESIAN_POINT('Ctrl Pts',(17.9324154880939,14.8416395585428,4.27299027832925));
#46814=CARTESIAN_POINT('Ctrl Pts',(17.9244033804411,14.8260225892159,4.33148490202253));
#46815=CARTESIAN_POINT('Ctrl Pts',(17.9156731062911,14.8113863758173,4.39017270789179));
#46816=CARTESIAN_POINT('Ctrl Pts',(17.9016880401047,14.7879405584717,4.48418497317845));
#46817=CARTESIAN_POINT('Ctrl Pts',(17.8858601407598,14.7670114814837,4.57869298264017));
#46818=CARTESIAN_POINT('Ctrl Pts',(17.8681487343997,14.7485990793917,4.67369153702113));
#46819=CARTESIAN_POINT('Ctrl Pts',(17.8633275572532,14.7435870859692,4.69955085332978));
#46820=CARTESIAN_POINT('Ctrl Pts',(17.8583668179424,14.738761572283,4.72544651760255));
#46821=CARTESIAN_POINT('Ctrl Pts',(17.8532654706195,14.7341229139912,4.7513784911553));
#46822=CARTESIAN_POINT('Ctrl Pts',(17.8443802227101,14.7260435525441,4.79654538515573));
#46823=CARTESIAN_POINT('Ctrl Pts',(17.8350684710653,14.718530907793,4.8418224347108));
#46824=CARTESIAN_POINT('Ctrl Pts',(17.8253246718829,14.71158690184,4.88720951203339));
#46825=CARTESIAN_POINT('Ctrl Pts',(17.8204527722917,14.7081148988635,4.90990305069469));
#46826=CARTESIAN_POINT('Ctrl Pts',(17.8154728604565,14.704785055436,4.93262409639065));
#46827=CARTESIAN_POINT('Ctrl Pts',(17.8103841833282,14.7015977386771,4.95537266126419));
#46828=CARTESIAN_POINT('Ctrl Pts',(17.8100602652887,14.7013948510955,4.95682071354793));
#46829=CARTESIAN_POINT('Ctrl Pts',(17.8097359181445,14.7011925479494,4.95826882593874));
#46830=CARTESIAN_POINT('Ctrl Pts',(17.8094111397357,14.7009908278893,4.95971700764907));
#46831=CARTESIAN_POINT('Ctrl Pts',(17.8071848214802,14.6996080603154,4.96964412500633));
#46832=CARTESIAN_POINT('Ctrl Pts',(17.8049374293926,14.6982522836604,4.97957790799021));
#46833=CARTESIAN_POINT('Ctrl Pts',(17.8026694530977,14.6969237531007,4.98951614577323));
#46834=CARTESIAN_POINT('Ctrl Pts',(17.8000706212612,14.6954014146521,5.00090418752978));
#46835=CARTESIAN_POINT('Ctrl Pts',(17.7974433294583,14.6939141022485,5.01230419126638));
#46836=CARTESIAN_POINT('Ctrl Pts',(17.7947921859334,14.6924644235442,5.02369591713228));
#46837=CARTESIAN_POINT('Ctrl Pts',(17.7941791730066,14.6921292203472,5.02632997867901));
#46838=CARTESIAN_POINT('Ctrl Pts',(17.7935648422523,14.6917960048101,5.02896378380818));
#46839=CARTESIAN_POINT('Ctrl Pts',(17.7929492152684,14.6914647890424,5.03159723664596));
#46840=CARTESIAN_POINT('Ctrl Pts',(17.7873483284016,14.6884514350272,5.05555601655535));
#46841=CARTESIAN_POINT('Ctrl Pts',(17.7816424538296,14.6856043845632,5.07947678558384));
#46842=CARTESIAN_POINT('Ctrl Pts',(17.7758323461943,14.6829213594339,5.1033604314301));
#46843=CARTESIAN_POINT('Ctrl Pts',(17.7642105485492,14.6775545784573,5.15113422779961));
#46844=CARTESIAN_POINT('Ctrl Pts',(17.7521717712571,14.6728439394171,5.19875951427955));
#46845=CARTESIAN_POINT('Ctrl Pts',(17.7397212214228,14.6687729664596,5.24624310344624));
#46846=CARTESIAN_POINT('Ctrl Pts',(17.7354095133055,14.6673631614807,5.26268698581072));
#46847=CARTESIAN_POINT('Ctrl Pts',(17.7310484383225,14.6660300309743,5.27911388004275));
#46848=CARTESIAN_POINT('Ctrl Pts',(17.7266381601075,14.6647730057,5.29552405089601));
#46849=CARTESIAN_POINT('Ctrl Pts',(17.7055762871139,14.658769913517,5.37389301481793));
#46850=CARTESIAN_POINT('Ctrl Pts',(17.6833946055873,14.6545023082244,5.45187298840078));
#46851=CARTESIAN_POINT('Ctrl Pts',(17.6601166503744,14.6519096363622,5.52947233599578));
#46852=CARTESIAN_POINT('Ctrl Pts',(17.6566350859603,14.6515218637245,5.54107847256024));
#46853=CARTESIAN_POINT('Ctrl Pts',(17.6531289967112,14.6511715627669,5.55267609381828));
#46854=CARTESIAN_POINT('Ctrl Pts',(17.6495984426794,14.650858573625,5.56426522108234));
#46855=CARTESIAN_POINT('Ctrl Pts',(17.6245782873355,14.6486404976851,5.64639447383985));
#46856=CARTESIAN_POINT('Ctrl Pts',(17.5983297977291,14.6482953236228,5.72809730835287));
#46857=CARTESIAN_POINT('Ctrl Pts',(17.570874188347,14.6497664199344,5.80938132211805));
#46858=CARTESIAN_POINT('Ctrl Pts',(17.5685523256427,14.6498908274321,5.81625533891355));
#46859=CARTESIAN_POINT('Ctrl Pts',(17.5662218403192,14.650028201591,5.82312636385389));
#46860=CARTESIAN_POINT('Ctrl Pts',(17.5638827400639,14.6501785196801,5.82999439969799));
#46861=CARTESIAN_POINT('Ctrl Pts',(17.5038856589009,14.6540341246598,6.00615705156473));
#46862=CARTESIAN_POINT('Ctrl Pts',(17.4382229946775,14.6663995345244,6.18035414179747));
#46863=CARTESIAN_POINT('Ctrl Pts',(17.3670255340948,14.686885583319,6.35263285243815));
#46864=CARTESIAN_POINT('Ctrl Pts',(17.3660868151046,14.6871556862536,6.35490429998657));
#46865=CARTESIAN_POINT('Ctrl Pts',(17.3651471338108,14.6874272011641,6.35717541405588));
#46866=CARTESIAN_POINT('Ctrl Pts',(17.3642064905221,14.6877001271357,6.35944619474937));
#46867=CARTESIAN_POINT('Ctrl Pts',(17.3473112813971,14.6926022419129,6.40023244725639));
#46868=CARTESIAN_POINT('Ctrl Pts',(17.3301052356159,14.6979606564321,6.44091098042997));
#46869=CARTESIAN_POINT('Ctrl Pts',(17.3125892792668,14.7037719520379,6.4814821016378));
#46870=CARTESIAN_POINT('Ctrl Pts',(17.3106500215433,14.7044153425364,6.48597388379275));
#46871=CARTESIAN_POINT('Ctrl Pts',(17.3087068447073,14.7050643246938,6.49046462743921));
#46872=CARTESIAN_POINT('Ctrl Pts',(17.3067598265897,14.7057188695631,6.49495415327635));
#46873=CARTESIAN_POINT('Ctrl Pts',(17.2994242664377,14.7081849243048,6.51186883246479));
#46874=CARTESIAN_POINT('Ctrl Pts',(17.2920351878217,14.7107297252115,6.52876361629531));
#46875=CARTESIAN_POINT('Ctrl Pts',(17.2846071230498,14.7133476118522,6.54560651341641));
#46876=CARTESIAN_POINT('Ctrl Pts',(17.2821447655724,14.7142154250636,6.55118982952103));
#46877=CARTESIAN_POINT('Ctrl Pts',(17.2796776634466,14.7150914327112,6.55676849028774));
#46878=CARTESIAN_POINT('Ctrl Pts',(17.2772062480082,14.7159754625462,6.56234155089384));
#46879=CARTESIAN_POINT('Ctrl Pts',(17.2702434505644,14.7184660679616,6.57804271207401));
#46880=CARTESIAN_POINT('Ctrl Pts',(17.2632433558177,14.7210213662988,6.59370650751666));
#46881=CARTESIAN_POINT('Ctrl Pts',(17.2562075816311,14.7236401478524,6.60933047448542));
#46882=CARTESIAN_POINT('Ctrl Pts',(17.2532097516256,14.724755968473,6.61598759504413));
#46883=CARTESIAN_POINT('Ctrl Pts',(17.2502053634654,14.725883353374,6.62263765588774));
#46884=CARTESIAN_POINT('Ctrl Pts',(17.2471944427328,14.7270222483695,6.62928068697227));
#46885=CARTESIAN_POINT('Ctrl Pts',(17.2119064798966,14.7403700870687,6.7071369491747));
#46886=CARTESIAN_POINT('Ctrl Pts',(17.1757218111607,14.7552975107985,6.78402829646679));
#46887=CARTESIAN_POINT('Ctrl Pts',(17.1386772777326,14.7717276730342,6.85999798429434));
#46888=CARTESIAN_POINT('Ctrl Pts',(17.1333754037566,14.7740791846209,6.87087088978365));
#46889=CARTESIAN_POINT('Ctrl Pts',(17.1280559071385,14.7764615087316,6.8817249071209));
#46890=CARTESIAN_POINT('Ctrl Pts',(17.1227188965086,14.7788744200072,6.8925601603357));
#46891=CARTESIAN_POINT('Ctrl Pts',(17.0471123438152,14.8130568333759,7.04605735191772));
#46892=CARTESIAN_POINT('Ctrl Pts',(16.9679967584232,14.8533638693528,7.19579527946855));
#46893=CARTESIAN_POINT('Ctrl Pts',(16.8856109571811,14.8993231905961,7.342046713768));
#46894=CARTESIAN_POINT('Ctrl Pts',(16.8749530043552,14.9052687815881,7.36096673231486));
#46895=CARTESIAN_POINT('Ctrl Pts',(16.8642402649882,14.9113091728742,7.37982832651959));
#46896=CARTESIAN_POINT('Ctrl Pts',(16.8534732588058,14.9174433438549,7.3986320679054));
#46897=CARTESIAN_POINT('Ctrl Pts',(16.7751364249307,14.9620733482351,7.53544127375318));
#46898=CARTESIAN_POINT('Ctrl Pts',(16.6939260422893,15.0116699463912,7.66918665661123));
#46899=CARTESIAN_POINT('Ctrl Pts',(16.6099844685074,15.0659826559846,7.80002155565286));
#46900=CARTESIAN_POINT('Ctrl Pts',(16.5930199143405,15.0769592300746,7.82646322968525));
#46901=CARTESIAN_POINT('Ctrl Pts',(16.5759431813926,15.0881292937242,7.85278656828423));
#46902=CARTESIAN_POINT('Ctrl Pts',(16.558756936468,15.099489782043,7.87899055063023));
#46903=CARTESIAN_POINT('Ctrl Pts',(16.5517615237535,15.1041139046932,7.88965650308689));
#46904=CARTESIAN_POINT('Ctrl Pts',(16.5447473800273,15.1087700325058,7.90030346917402));
#46905=CARTESIAN_POINT('Ctrl Pts',(16.5377151519886,15.1134576667111,7.91093065893069));
#46906=CARTESIAN_POINT('Ctrl Pts',(16.5255606917866,15.1215597451814,7.92929862911696));
#46907=CARTESIAN_POINT('Ctrl Pts',(16.5133516708353,15.1297562440715,7.94760839472119));
#46908=CARTESIAN_POINT('Ctrl Pts',(16.5010884079715,15.1380466877915,7.96586027627348));
#46909=CARTESIAN_POINT('Ctrl Pts',(16.4944989617198,15.1425014103154,7.97566760029621));
#46910=CARTESIAN_POINT('Ctrl Pts',(16.4878941994145,15.1469830271346,7.98545769044203));
#46911=CARTESIAN_POINT('Ctrl Pts',(16.4812751499307,15.1514907998686,7.99522914710671));
#46912=CARTESIAN_POINT('Ctrl Pts',(16.4755758435728,15.1553721997383,8.00364282118959));
#46913=CARTESIAN_POINT('Ctrl Pts',(16.4698677621575,15.1592717459216,8.01204001683089));
#46914=CARTESIAN_POINT('Ctrl Pts',(16.4641513393775,15.1631890857729,8.02042025617386));
#46915=CARTESIAN_POINT('Ctrl Pts',(16.4437117286727,15.177195905184,8.05038459512734));
#46916=CARTESIAN_POINT('Ctrl Pts',(16.4231596967393,15.1914341799859,8.08014062779508));
#46917=CARTESIAN_POINT('Ctrl Pts',(16.4024974398753,15.2058999341082,8.10969210477789));
#46918=CARTESIAN_POINT('Ctrl Pts',(16.3731999518779,15.2264112587209,8.1515938218994));
#46919=CARTESIAN_POINT('Ctrl Pts',(16.3436809381474,15.2473796884686,8.19308445418479));
#46920=CARTESIAN_POINT('Ctrl Pts',(16.3139460336245,15.2687956713135,8.23417339797329));
#46921=CARTESIAN_POINT('Ctrl Pts',(16.2899592323926,15.2860716952971,8.26731937046929));
#46922=CARTESIAN_POINT('Ctrl Pts',(16.2658319325667,15.3036390269857,8.30020390682567));
#46923=CARTESIAN_POINT('Ctrl Pts',(16.2415670965676,15.3214927217308,8.33283183165488));
#46924=CARTESIAN_POINT('Ctrl Pts',(16.2145385429846,15.3413799175515,8.36917601360532));
#46925=CARTESIAN_POINT('Ctrl Pts',(16.1873393276794,15.361622446644,8.40520178115493));
#46926=CARTESIAN_POINT('Ctrl Pts',(16.159973040911,15.3822149926241,8.44091470888462));
#46927=CARTESIAN_POINT('Ctrl Pts',(16.1340058798433,15.4017547264134,8.47480178148602));
#46928=CARTESIAN_POINT('Ctrl Pts',(16.1078883340152,15.4216092771505,8.50840736974749));
#46929=CARTESIAN_POINT('Ctrl Pts',(16.0816234182085,15.4417746145561,8.54173588342655));
#46930=CARTESIAN_POINT('Ctrl Pts',(16.0798486235869,15.4431372434193,8.54398798532766));
#46931=CARTESIAN_POINT('Ctrl Pts',(16.0780731561048,15.4445012909336,8.54623882233379));
#46932=CARTESIAN_POINT('Ctrl Pts',(16.0762970167215,15.4458667556287,8.54848839592704));
#46933=CARTESIAN_POINT('Ctrl Pts',(16.0649307477388,15.454604943159,8.56288437115155));
#46934=CARTESIAN_POINT('Ctrl Pts',(16.0535369512196,15.4634012045553,8.57722858040296));
#46935=CARTESIAN_POINT('Ctrl Pts',(16.0421158599722,15.472255213642,8.59152137068278));
#46936=CARTESIAN_POINT('Ctrl Pts',(16.0395193741824,15.4742680956231,8.59477071227845));
#46937=CARTESIAN_POINT('Ctrl Pts',(16.0369214123754,15.4762840129575,8.59801747797031));
#46938=CARTESIAN_POINT('Ctrl Pts',(16.0343220133108,15.478302934371,8.60126162608156));
#46939=CARTESIAN_POINT('Ctrl Pts',(16.0237007979998,15.4865523022038,8.61451730354146));
#46940=CARTESIAN_POINT('Ctrl Pts',(16.0130541971412,15.4948529430825,8.62773092316722));
#46941=CARTESIAN_POINT('Ctrl Pts',(16.0023948674495,15.5031947937513,8.64088751525607));
#46942=CARTESIAN_POINT('Ctrl Pts',(15.998966260682,15.5058779761355,8.645119374292));
#46943=CARTESIAN_POINT('Ctrl Pts',(15.9955361555857,15.5085655671632,8.649345555432));
#46944=CARTESIAN_POINT('Ctrl Pts',(15.9921048908792,15.5112572959462,8.65356566263564));
#46945=CARTESIAN_POINT('Ctrl Pts',(15.963891155855,15.5333901621449,8.68826569210053));
#46946=CARTESIAN_POINT('Ctrl Pts',(15.9355795517899,15.5558177771029,8.72257963369553));
#46947=CARTESIAN_POINT('Ctrl Pts',(15.9071741212286,15.5785326177975,8.75651763111319));
#46948=CARTESIAN_POINT('Ctrl Pts',(15.8320856427827,15.6385782778068,8.84623120127341));
#46949=CARTESIAN_POINT('Ctrl Pts',(15.7563428898215,15.7006252473126,8.93332397978106));
#46950=CARTESIAN_POINT('Ctrl Pts',(15.6800121405069,15.7645675407892,9.01794758228341));
#46951=CARTESIAN_POINT('Ctrl Pts',(15.6406445808878,15.7975457582603,9.06159217828978));
#46952=CARTESIAN_POINT('Ctrl Pts',(15.6011197257036,15.8310304240877,9.10457977539739));
#46953=CARTESIAN_POINT('Ctrl Pts',(15.5614458176104,15.8650078553951,9.1469317593497));
#46954=CARTESIAN_POINT('Ctrl Pts',(15.4915558576705,15.9248628439017,9.22153944495621));
#46955=CARTESIAN_POINT('Ctrl Pts',(15.4212030312285,15.9862476883049,9.29417371478342));
#46956=CARTESIAN_POINT('Ctrl Pts',(15.3504255247275,16.0491202511077,9.36491710445505));
#46957=CARTESIAN_POINT('Ctrl Pts',(15.3028155108123,16.0914128344143,9.41250416895029));
#46958=CARTESIAN_POINT('Ctrl Pts',(15.2550134038353,16.1343797974888,9.45923461112119));
#46959=CARTESIAN_POINT('Ctrl Pts',(15.2070311136134,16.1780085379062,9.50513258392003));
#46960=CARTESIAN_POINT('Ctrl Pts',(15.1431905716113,16.2360566723789,9.56619993703555));
#46961=CARTESIAN_POINT('Ctrl Pts',(15.0790308535853,16.2952765226413,9.62579322207588));
#46962=CARTESIAN_POINT('Ctrl Pts',(15.0145773289901,16.35565810712,9.6839498613404));
#46963=CARTESIAN_POINT('Ctrl Pts',(14.9582797762188,16.4083989845189,9.73474733888037));
#46964=CARTESIAN_POINT('Ctrl Pts',(14.9017581147026,16.4620266993466,9.78444830855335));
#46965=CARTESIAN_POINT('Ctrl Pts',(14.8450296295046,16.51653473843,9.83307664083576));
#46966=CARTESIAN_POINT('Ctrl Pts',(14.7879974125538,16.5713346207062,9.88196533558943));
#46967=CARTESIAN_POINT('Ctrl Pts',(14.7307560003233,16.6270242276471,9.92976976812893));
#46968=CARTESIAN_POINT('Ctrl Pts',(14.673322350996,16.6836096033916,9.97650269153596));
#46969=CARTESIAN_POINT('Ctrl Pts',(14.6079377474624,16.7480285007138,10.0297051905017));
#46970=CARTESIAN_POINT('Ctrl Pts',(14.542303948576,16.8136074931285,10.0815196120906));
#46971=CARTESIAN_POINT('Ctrl Pts',(14.4764465245309,16.8803555924736,10.1319634598115));
#46972=CARTESIAN_POINT('Ctrl Pts',(14.4269140830284,16.930557925379,10.1699030994592));
#46973=CARTESIAN_POINT('Ctrl Pts',(14.3772551335397,16.9814228338856,10.2070663578355));
#46974=CARTESIAN_POINT('Ctrl Pts',(14.3274807199144,17.0329603662361,10.2434554339001));
#46975=CARTESIAN_POINT('Ctrl Pts',(14.314990397583,17.0458931231355,10.2525868581859));
#46976=CARTESIAN_POINT('Ctrl Pts',(14.3024946467154,17.05886631397,10.2616681973105));
#46977=CARTESIAN_POINT('Ctrl Pts',(14.2899914513039,17.07188234669,10.2707011041516));
#46978=CARTESIAN_POINT('Ctrl Pts',(14.2734763801558,17.0890748082458,10.2826323820567));
#46979=CARTESIAN_POINT('Ctrl Pts',(14.2569416682199,17.1063491334474,10.2944837091251));
#46980=CARTESIAN_POINT('Ctrl Pts',(14.2404003000471,17.1236924326205,10.3062463900494));
#46981=CARTESIAN_POINT('Ctrl Pts',(14.2257017395037,17.1391035842408,10.3166986377662));
#46982=CARTESIAN_POINT('Ctrl Pts',(14.2110064088285,17.1545603076558,10.3270748478657));
#46983=CARTESIAN_POINT('Ctrl Pts',(14.1963246412405,17.170052197827,10.3373681732381));
#46984=CARTESIAN_POINT('Ctrl Pts',(14.181975142211,17.1851934852533,10.3474285465246));
#46985=CARTESIAN_POINT('Ctrl Pts',(14.1676354439626,17.2003715773109,10.3574121351433));
#46986=CARTESIAN_POINT('Ctrl Pts',(14.1533036570002,17.2155887738345,10.3673208975942));
#46987=CARTESIAN_POINT('Ctrl Pts',(14.1364434248707,17.2334906214145,10.3789777855647));
#46988=CARTESIAN_POINT('Ctrl Pts',(14.1195959115965,17.2514448030669,10.3905298278396));
#46989=CARTESIAN_POINT('Ctrl Pts',(14.102761535583,17.2694513331259,10.4019778023782));
#46990=CARTESIAN_POINT('Ctrl Pts',(14.0616939791491,17.3133783660484,10.4299052016498));
#46991=CARTESIAN_POINT('Ctrl Pts',(14.0207043099312,17.357616068478,10.4572145106538));
#46992=CARTESIAN_POINT('Ctrl Pts',(13.9797992920512,17.4021669272979,10.4839136631712));
#46993=CARTESIAN_POINT('Ctrl Pts',(13.8963730378755,17.4930289159798,10.5383668916413));
#46994=CARTESIAN_POINT('Ctrl Pts',(13.8132979186715,17.5851917329795,10.5902846035054));
#46995=CARTESIAN_POINT('Ctrl Pts',(13.7306345084654,17.6786798143199,10.6397262633505));
#46996=CARTESIAN_POINT('Ctrl Pts',(13.6990070978718,17.7144487951397,10.658642875579));
#46997=CARTESIAN_POINT('Ctrl Pts',(13.6674398860713,17.7504117000158,10.6771970283303));
#46998=CARTESIAN_POINT('Ctrl Pts',(13.6359369836638,17.7865716688882,10.6953896284376));
#46999=CARTESIAN_POINT('Ctrl Pts',(13.5443304572451,17.8917203660138,10.7482914493811));
#47000=CARTESIAN_POINT('Ctrl Pts',(13.4532652978713,17.9985304127055,10.7981423054322));
#47001=CARTESIAN_POINT('Ctrl Pts',(13.362843952931,18.1070757677516,10.8449629340514));
#47002=CARTESIAN_POINT('Ctrl Pts',(13.3408972516745,18.133421455062,10.8563270466912));
#47003=CARTESIAN_POINT('Ctrl Pts',(13.3189884250314,18.1598692890699,10.8675126974676));
#47004=CARTESIAN_POINT('Ctrl Pts',(13.2971192937982,18.1864210638634,10.8785192895612));
#47005=CARTESIAN_POINT('Ctrl Pts',(13.1974886473656,18.3073847390275,10.9286627485591));
#47006=CARTESIAN_POINT('Ctrl Pts',(13.0986789283229,18.4304994909325,10.9750973239262));
#47007=CARTESIAN_POINT('Ctrl Pts',(13.0008637679413,18.555928374369,11.0177665156938));
#47008=CARTESIAN_POINT('Ctrl Pts',(12.9887483958524,18.5714639783347,11.0230515158204));
#47009=CARTESIAN_POINT('Ctrl Pts',(12.9766482540743,18.5870350362773,11.0282787901708));
#47010=CARTESIAN_POINT('Ctrl Pts',(12.9645637645202,18.6026420312121,11.0334480392572));
#47011=CARTESIAN_POINT('Ctrl Pts',(12.8572271761536,18.7412661396995,11.0793622302421));
#47012=CARTESIAN_POINT('Ctrl Pts',(12.7511223420231,18.8827189620378,11.1207063336849));
#47013=CARTESIAN_POINT('Ctrl Pts',(12.6465462824545,19.0273228911961,11.1572752841488));
#47014=CARTESIAN_POINT('Ctrl Pts',(12.644292060807,19.0304399459864,11.1580635574889));
#47015=CARTESIAN_POINT('Ctrl Pts',(12.6420385516737,19.0335584688927,11.1588496076951));
#47016=CARTESIAN_POINT('Ctrl Pts',(12.6397857586885,19.0366784643387,11.1596334314464));
#47017=CARTESIAN_POINT('Ctrl Pts',(12.5836913769038,19.1143661244414,11.1791505859489));
#47018=CARTESIAN_POINT('Ctrl Pts',(12.5281517057416,19.1928079324649,11.1972529590116));
#47019=CARTESIAN_POINT('Ctrl Pts',(12.4729858003008,19.2724054736595,11.2139668936264));
#47020=CARTESIAN_POINT('Ctrl Pts',(12.4443163748122,19.313771889349,11.2226530358955));
#47021=CARTESIAN_POINT('Ctrl Pts',(12.4157289692281,19.3554805340295,11.2309679359619));
#47022=CARTESIAN_POINT('Ctrl Pts',(12.3873311427962,19.39739837676,11.2388739303386));
#47023=CARTESIAN_POINT('Ctrl Pts',(12.3663714964643,19.428336771314,11.2447091250298));
#47024=CARTESIAN_POINT('Ctrl Pts',(12.3455020862917,19.4594076778139,11.2503257124173));
#47025=CARTESIAN_POINT('Ctrl Pts',(12.3247145835032,19.4906334206159,11.2557233274532));
#47026=CARTESIAN_POINT('Origin',(6.61325378140121E-15,19.4906334205523,
8.67361737988404E-16));
#47027=CARTESIAN_POINT('Origin',(3.30643715532042E-15,11.4559962546824,
4.33680868994202E-16));
#47028=CARTESIAN_POINT('',(9.18375896983081E-16,11.4559962546824,19.5));
#47029=CARTESIAN_POINT('Origin',(0.,11.4559962546824,0.));
#47030=CARTESIAN_POINT('Origin',(1.28576993672729E-15,11.4559962546824,
16.5));
#47031=CARTESIAN_POINT('Origin',(6.61363325216158E-15,52.,8.67361737988404E-16));
#47032=CARTESIAN_POINT('',(-4.71428571428571,51.,-15.8121949837485));
#47033=CARTESIAN_POINT('',(8.63430047075471E-15,51.,16.5));
#47034=CARTESIAN_POINT('Origin',(6.61363325216158E-15,51.,8.67361737988404E-16));
#47035=CARTESIAN_POINT('',(8.63430047075471E-15,20.5439967627459,16.5));
#47036=CARTESIAN_POINT('',(8.63430047075471E-15,52.,16.5));
#47037=CARTESIAN_POINT('',(12.0252610002882,20.5440037453176,11.2979244951432));
#47038=CARTESIAN_POINT('Origin',(6.61363325216158E-15,20.5440037453176,
8.67361737988404E-16));
#47039=CARTESIAN_POINT('',(15.4998953469709,26.9999999999978,5.65714310527842));
#47040=CARTESIAN_POINT('Ctrl Pts',(12.0252610013046,20.5440037453176,11.2979244960981));
#47041=CARTESIAN_POINT('Ctrl Pts',(12.0249308728691,20.548893260366,11.2982758756345));
#47042=CARTESIAN_POINT('Ctrl Pts',(12.0246060118186,20.5537834284514,11.2986216185138));
#47043=CARTESIAN_POINT('Ctrl Pts',(12.024286421815,20.5586742495714,11.298961724254));
#47044=CARTESIAN_POINT('Ctrl Pts',(12.0228356969254,20.5808753067053,11.3005055768679));
#47045=CARTESIAN_POINT('Ctrl Pts',(12.0214935973948,20.6030898283043,11.3019332419997));
#47046=CARTESIAN_POINT('Ctrl Pts',(12.0202605030161,20.6253178445758,11.3032445556378));
#47047=CARTESIAN_POINT('Ctrl Pts',(12.0196817441633,20.6357506722801,11.3038600270809));
#47048=CARTESIAN_POINT('Ctrl Pts',(12.0191271097146,20.6461843806063,11.3044497486797));
#47049=CARTESIAN_POINT('Ctrl Pts',(12.0185964357884,20.656622724066,11.3050139192154));
#47050=CARTESIAN_POINT('Ctrl Pts',(12.0177638774852,20.6729991260151,11.3058990293379));
#47051=CARTESIAN_POINT('Ctrl Pts',(12.0169903907423,20.6893867131252,11.3067211441569));
#47052=CARTESIAN_POINT('Ctrl Pts',(12.0162772436363,20.7057571332248,11.3074789941909));
#47053=CARTESIAN_POINT('Ctrl Pts',(12.0162631181461,20.7060813863941,11.3074940051237));
#47054=CARTESIAN_POINT('Ctrl Pts',(12.0162490161176,20.706405637056,11.307508991068));
#47055=CARTESIAN_POINT('Ctrl Pts',(12.0162349375449,20.7067298853232,11.3075239520309));
#47056=CARTESIAN_POINT('Ctrl Pts',(12.0155382159022,20.7227763120345,11.3082643414754));
#47057=CARTESIAN_POINT('Ctrl Pts',(12.0148990649862,20.738814572496,11.3089434156603));
#47058=CARTESIAN_POINT('Ctrl Pts',(12.0143172936214,20.7548446975429,11.3095614401351));
#47059=CARTESIAN_POINT('Ctrl Pts',(12.0129319285457,20.7930170393609,11.3110331343007));
#47060=CARTESIAN_POINT('Ctrl Pts',(12.0118718817328,20.8311432832627,11.3121590426822));
#47061=CARTESIAN_POINT('Ctrl Pts',(12.0111346855915,20.8692237895445,11.3129419381104));
#47062=CARTESIAN_POINT('Ctrl Pts',(12.0093466729179,20.9615851355062,11.3148407908979));
#47063=CARTESIAN_POINT('Ctrl Pts',(12.0094576599568,21.0536774553069,11.3147220486198));
#47064=CARTESIAN_POINT('Ctrl Pts',(12.01143572497,21.1455054304304,11.3126217927108));
#47065=CARTESIAN_POINT('Ctrl Pts',(12.0117737384095,21.1611970732783,11.3122628991866));
#47066=CARTESIAN_POINT('Ctrl Pts',(12.0121662715151,21.1768809958035,11.3118461408723));
#47067=CARTESIAN_POINT('Ctrl Pts',(12.0126131765915,21.1925572116773,11.3113716032014));
#47068=CARTESIAN_POINT('Ctrl Pts',(12.0156753838789,21.2999711235487,11.3081200565288));
#47069=CARTESIAN_POINT('Ctrl Pts',(12.0212890769295,21.4070235554608,11.3021571360844));
#47070=CARTESIAN_POINT('Ctrl Pts',(12.029405224626,21.5137197802307,11.293511875714));
#47071=CARTESIAN_POINT('Ctrl Pts',(12.0298842581913,21.5200172349913,11.2930016127108));
#47072=CARTESIAN_POINT('Ctrl Pts',(12.0303720112037,21.526313448837,11.292482003453));
#47073=CARTESIAN_POINT('Ctrl Pts',(12.0308684730983,21.5326084229108,11.2919530544105));
#47074=CARTESIAN_POINT('Ctrl Pts',(12.038783442791,21.6329676439405,11.2835201501216));
#47075=CARTESIAN_POINT('Ctrl Pts',(12.0489119741868,21.7330116990756,11.2727132659417));
#47076=CARTESIAN_POINT('Ctrl Pts',(12.0612142372056,21.8327433602281,11.2595345438906));
#47077=CARTESIAN_POINT('Ctrl Pts',(12.0646499496549,21.8605959032351,11.2558540584914));
#47078=CARTESIAN_POINT('Ctrl Pts',(12.0682552832817,21.8884240721786,11.2519884939938));
#47079=CARTESIAN_POINT('Ctrl Pts',(12.0720293911064,21.9162279265017,11.2479378723508));
#47080=CARTESIAN_POINT('Ctrl Pts',(12.0806670632113,21.9798616614262,11.2386673524827));
#47081=CARTESIAN_POINT('Ctrl Pts',(12.0901888787009,22.0433679653625,11.2284267261222));
#47082=CARTESIAN_POINT('Ctrl Pts',(12.1005853276592,22.1067471382375,11.217211539774));
#47083=CARTESIAN_POINT('Ctrl Pts',(12.1029321776561,22.1210540821047,11.2146798714946));
#47084=CARTESIAN_POINT('Ctrl Pts',(12.1053235973978,22.1353545469586,11.2120985328033));
#47085=CARTESIAN_POINT('Ctrl Pts',(12.1077594815789,22.1496485338453,11.2094674447032));
#47086=CARTESIAN_POINT('Ctrl Pts',(12.1107170104573,22.1670035786097,11.2062729089786));
#47087=CARTESIAN_POINT('Ctrl Pts',(12.1137401289893,22.1843493271757,11.2030049893633));
#47088=CARTESIAN_POINT('Ctrl Pts',(12.1168286615825,22.2016858050301,11.1996635300287));
#47089=CARTESIAN_POINT('Ctrl Pts',(12.1184242270949,22.2106419954981,11.1979373001397));
#47090=CARTESIAN_POINT('Ctrl Pts',(12.1200374772146,22.219596819521,11.1961911962994));
#47091=CARTESIAN_POINT('Ctrl Pts',(12.1216670572837,22.2285432875991,11.1944266373505));
#47092=CARTESIAN_POINT('Ctrl Pts',(12.1229129709795,22.235383409983,11.1930775240402));
#47093=CARTESIAN_POINT('Ctrl Pts',(12.1241684933701,22.2422189946054,11.191717554553));
#47094=CARTESIAN_POINT('Ctrl Pts',(12.1254330313338,22.2490469590199,11.1903473495079));
#47095=CARTESIAN_POINT('Ctrl Pts',(12.1283503922125,22.2647994605947,11.187186208673));
#47096=CARTESIAN_POINT('Ctrl Pts',(12.1313172199455,22.2805198972878,11.1839689876802));
#47097=CARTESIAN_POINT('Ctrl Pts',(12.1343330639684,22.2962091557006,11.1806959127187));
#47098=CARTESIAN_POINT('Ctrl Pts',(12.1350293696224,22.2998315311472,11.1799402169387));
#47099=CARTESIAN_POINT('Ctrl Pts',(12.1357282849766,22.303452247295,11.1791815485227));
#47100=CARTESIAN_POINT('Ctrl Pts',(12.136429805251,22.3070713144085,11.178419909148));
#47101=CARTESIAN_POINT('Ctrl Pts',(12.1465437361255,22.3592479883444,11.1674392315131));
#47102=CARTESIAN_POINT('Ctrl Pts',(12.1571983969572,22.411075698049,11.1558418062304));
#47103=CARTESIAN_POINT('Ctrl Pts',(12.1683725405619,22.4625644347832,11.1436401560417));
#47104=CARTESIAN_POINT('Ctrl Pts',(12.1832259279363,22.5310065614632,11.1274209411048));
#47105=CARTESIAN_POINT('Ctrl Pts',(12.1989982808949,22.5988489749547,11.1101329448993));
#47106=CARTESIAN_POINT('Ctrl Pts',(12.2156434245513,22.6661129579501,11.0918012840217));
#47107=CARTESIAN_POINT('Ctrl Pts',(12.2240424301989,22.7000538229085,11.0825512753454));
#47108=CARTESIAN_POINT('Ctrl Pts',(12.2326636902816,22.7338473804668,11.0730354852607));
#47109=CARTESIAN_POINT('Ctrl Pts',(12.2415021288752,22.7674955939997,11.0632558073106));
#47110=CARTESIAN_POINT('Ctrl Pts',(12.2641668096522,22.8537807461063,11.0381774774118));
#47111=CARTESIAN_POINT('Ctrl Pts',(12.2882575055527,22.9391117544965,11.0113662686165));
#47112=CARTESIAN_POINT('Ctrl Pts',(12.3136878264858,23.0235234978828,10.9828544610159));
#47113=CARTESIAN_POINT('Ctrl Pts',(12.3178278371292,23.0372655783292,10.9782127898692));
#47114=CARTESIAN_POINT('Ctrl Pts',(12.3220033536933,23.0509832918754,10.9735260433554));
#47115=CARTESIAN_POINT('Ctrl Pts',(12.3262140559314,23.0646767404433,10.9687942764753));
#47116=CARTESIAN_POINT('Ctrl Pts',(12.3562893074409,23.162483207494,10.9349972823026));
#47117=CARTESIAN_POINT('Ctrl Pts',(12.3881579513823,23.259053126514,10.8989055023022));
#47118=CARTESIAN_POINT('Ctrl Pts',(12.4217002577817,23.3544275618513,10.8605415533984));
#47119=CARTESIAN_POINT('Ctrl Pts',(12.4234325753308,23.3593532460336,10.8585602185091));
#47120=CARTESIAN_POINT('Ctrl Pts',(12.4251693574216,23.3642757416104,10.8565728222644));
#47121=CARTESIAN_POINT('Ctrl Pts',(12.4269105870875,23.3691950546363,10.854579368199));
#47122=CARTESIAN_POINT('Ctrl Pts',(12.4420267918443,23.411901277955,10.8372735179623));
#47123=CARTESIAN_POINT('Ctrl Pts',(12.4574784902714,23.4543673858017,10.8195106603123));
#47124=CARTESIAN_POINT('Ctrl Pts',(12.4732557741443,23.4965962769449,10.8012911523043));
#47125=CARTESIAN_POINT('Ctrl Pts',(12.4783984540648,23.5103609827268,10.7953524179347));
#47126=CARTESIAN_POINT('Ctrl Pts',(12.4835754560386,23.5240997521511,10.7893654779865));
#47127=CARTESIAN_POINT('Ctrl Pts',(12.4887867248453,23.5378134440997,10.7833300117045));
#47128=CARTESIAN_POINT('Ctrl Pts',(12.4924901191887,23.5475590955087,10.7790409004501));
#47129=CARTESIAN_POINT('Ctrl Pts',(12.4962117800455,23.55729444906,10.774726155287));
#47130=CARTESIAN_POINT('Ctrl Pts',(12.4999498795827,23.5670152413277,10.7703877686227));
#47131=CARTESIAN_POINT('Ctrl Pts',(12.504448981637,23.5787149930396,10.7651661729537));
#47132=CARTESIAN_POINT('Ctrl Pts',(12.5089736617026,23.590398206173,10.7599082780242));
#47133=CARTESIAN_POINT('Ctrl Pts',(12.5135167964196,23.6020472903523,10.7546221314614));
#47134=CARTESIAN_POINT('Ctrl Pts',(12.5159900547159,23.6083889896161,10.7517443814812));
#47135=CARTESIAN_POINT('Ctrl Pts',(12.5184694270114,23.6147222115016,10.7488575096783));
#47136=CARTESIAN_POINT('Ctrl Pts',(12.5209543788166,23.621045733523,10.7459620994861));
#47137=CARTESIAN_POINT('Ctrl Pts',(12.523034041566,23.6263379058562,10.7435389230253));
#47138=CARTESIAN_POINT('Ctrl Pts',(12.5251178344798,23.6316238943125,10.7411095107864));
#47139=CARTESIAN_POINT('Ctrl Pts',(12.5272057361195,23.6369037580822,10.7386738679465));
#47140=CARTESIAN_POINT('Ctrl Pts',(12.5359929025913,23.6591246525012,10.7284231939234));
#47141=CARTESIAN_POINT('Ctrl Pts',(12.5448522441492,23.6812349383611,10.7180628615953));
#47142=CARTESIAN_POINT('Ctrl Pts',(12.5537816116273,23.7032364478602,10.7075939056153));
#47143=CARTESIAN_POINT('Ctrl Pts',(12.5821071150075,23.773029054472,10.6743845603033));
#47144=CARTESIAN_POINT('Ctrl Pts',(12.6111358407004,23.8417290631451,10.6400837415979));
#47145=CARTESIAN_POINT('Ctrl Pts',(12.6408066531758,23.9093846481827,10.604716206553));
#47146=CARTESIAN_POINT('Ctrl Pts',(12.6573308096376,23.9470631402563,10.5850194529426));
#47147=CARTESIAN_POINT('Ctrl Pts',(12.6740544347473,23.9844172157351,10.5649914598182));
#47148=CARTESIAN_POINT('Ctrl Pts',(12.6909669667773,24.0214553684772,10.5446364303458));
#47149=CARTESIAN_POINT('Ctrl Pts',(12.7139959188659,24.0718883754,10.5169200010344));
#47150=CARTESIAN_POINT('Ctrl Pts',(12.7373752989098,24.1217354114684,10.4885970630843));
#47151=CARTESIAN_POINT('Ctrl Pts',(12.7610828922023,24.1710115636718,10.4596731584983));
#47152=CARTESIAN_POINT('Ctrl Pts',(12.7858766861947,24.2225453803435,10.4294240597008));
#47153=CARTESIAN_POINT('Ctrl Pts',(12.8110293324431,24.2734549676925,10.3985178216957));
#47154=CARTESIAN_POINT('Ctrl Pts',(12.8365157707695,24.3237575293058,10.3669601555514));
#47155=CARTESIAN_POINT('Ctrl Pts',(12.8532965490679,24.356877737138,10.3461819600108));
#47156=CARTESIAN_POINT('Ctrl Pts',(12.8702220812317,24.3897347297404,10.3251213217501));
#47157=CARTESIAN_POINT('Ctrl Pts',(12.8872863473921,24.4223316737733,10.3037784633077));
#47158=CARTESIAN_POINT('Ctrl Pts',(12.9207515320077,24.4862584046218,10.261922417974));
#47159=CARTESIAN_POINT('Ctrl Pts',(12.9547492668051,24.5491865853333,10.218982271535));
#47160=CARTESIAN_POINT('Ctrl Pts',(12.989234150632,24.6111411057364,10.1749592716658));
#47161=CARTESIAN_POINT('Ctrl Pts',(12.9990401875224,24.6287583410343,10.1624409995176));
#47162=CARTESIAN_POINT('Ctrl Pts',(13.0088856229381,24.6462968362974,10.1498351639255));
#47163=CARTESIAN_POINT('Ctrl Pts',(13.018769570305,24.6637569001809,10.137141572148));
#47164=CARTESIAN_POINT('Ctrl Pts',(13.0612011775983,24.7387126386645,10.0826482122126));
#47165=CARTESIAN_POINT('Ctrl Pts',(13.1043412580011,24.8122250522767,10.0265393117696));
#47166=CARTESIAN_POINT('Ctrl Pts',(13.1481190796857,24.8843211741588,9.96879955994731));
#47167=CARTESIAN_POINT('Ctrl Pts',(13.150400445733,24.8880782739477,9.96579060462879));
#47168=CARTESIAN_POINT('Ctrl Pts',(13.1526835438624,24.8918315272673,9.9627772203878));
#47169=CARTESIAN_POINT('Ctrl Pts',(13.1549683655095,24.8955809352535,9.95975940265458));
#47170=CARTESIAN_POINT('Ctrl Pts',(13.2010973193871,24.9712788647993,9.89883176954819));
#47171=CARTESIAN_POINT('Ctrl Pts',(13.2479284546171,25.0454100868088,9.83609760807509));
#47172=CARTESIAN_POINT('Ctrl Pts',(13.2953897478999,25.1179881253617,9.77152044143306));
#47173=CARTESIAN_POINT('Ctrl Pts',(13.3010243543399,25.1266045927006,9.7638538378943));
#47174=CARTESIAN_POINT('Ctrl Pts',(13.3066676460292,25.1351988393214,9.75616152364732));
#47175=CARTESIAN_POINT('Ctrl Pts',(13.3123196583909,25.1437711353646,9.74844322509082));
#47176=CARTESIAN_POINT('Ctrl Pts',(13.3261977499658,25.1648197640443,9.72949152305712));
#47177=CARTESIAN_POINT('Ctrl Pts',(13.34012850467,25.1857358948461,9.71038301825754));
#47178=CARTESIAN_POINT('Ctrl Pts',(13.354112658698,25.206523063251,9.69111320224889));
#47179=CARTESIAN_POINT('Ctrl Pts',(13.3584191706195,25.2129246080545,9.68517893606442));
#47180=CARTESIAN_POINT('Ctrl Pts',(13.3627307231837,25.2193138613263,9.67922939251358));
#47181=CARTESIAN_POINT('Ctrl Pts',(13.3670465731033,25.2256898232767,9.6732655098805));
#47182=CARTESIAN_POINT('Ctrl Pts',(13.3767333995054,25.2400005239987,9.65987971175828));
#47183=CARTESIAN_POINT('Ctrl Pts',(13.3864388290379,25.254239747419,9.64642588898842));
#47184=CARTESIAN_POINT('Ctrl Pts',(13.3961546301693,25.2683965644849,9.63291446679527));
#47185=CARTESIAN_POINT('Ctrl Pts',(13.4105486129811,25.2893699231161,9.6128972622249));
#47186=CARTESIAN_POINT('Ctrl Pts',(13.4249722375238,25.3101727876637,9.5927441957544));
#47187=CARTESIAN_POINT('Ctrl Pts',(13.4394268689906,25.3308108782405,9.57245033620673));
#47188=CARTESIAN_POINT('Ctrl Pts',(13.4531522150938,25.3504077068919,9.55318037095716));
#47189=CARTESIAN_POINT('Ctrl Pts',(13.4669038118876,25.3698533742983,9.53378584359692));
#47190=CARTESIAN_POINT('Ctrl Pts',(13.4806800176673,25.3891488043011,9.51426645944222));
#47191=CARTESIAN_POINT('Ctrl Pts',(13.5155059835076,25.4379272558502,9.4649218563875));
#47192=CARTESIAN_POINT('Ctrl Pts',(13.5504889007219,25.4857465093747,9.41477989849423));
#47193=CARTESIAN_POINT('Ctrl Pts',(13.5856048493766,25.5326144032833,9.36383157029569));
#47194=CARTESIAN_POINT('Ctrl Pts',(13.6074054038267,25.5617107572836,9.33220201604527));
#47195=CARTESIAN_POINT('Ctrl Pts',(13.6292572492356,25.5904404157791,9.30026164404338));
#47196=CARTESIAN_POINT('Ctrl Pts',(13.6511549037297,25.6188047072121,9.26800786546799));
#47197=CARTESIAN_POINT('Ctrl Pts',(13.6538698198203,25.6223213702058,9.26400897588554));
#47198=CARTESIAN_POINT('Ctrl Pts',(13.6565854424971,25.6258324098416,9.2600052645616));
#47199=CARTESIAN_POINT('Ctrl Pts',(13.6593017621577,25.6293378259766,9.25599672497029));
#47200=CARTESIAN_POINT('Ctrl Pts',(13.6708601828647,25.6442539917827,9.23893967984864));
#47201=CARTESIAN_POINT('Ctrl Pts',(13.6824315688055,25.6590689268798,9.22179469795511));
#47202=CARTESIAN_POINT('Ctrl Pts',(13.694014042668,25.6737812611331,9.20456296622561));
#47203=CARTESIAN_POINT('Ctrl Pts',(13.6947698389658,25.6747412915975,9.20343853640167));
#47204=CARTESIAN_POINT('Ctrl Pts',(13.6955256987437,25.6757009054187,9.20231371272741));
#47205=CARTESIAN_POINT('Ctrl Pts',(13.6962816185107,25.6766600985106,9.20118850000519));
#47206=CARTESIAN_POINT('Ctrl Pts',(13.7086219042892,25.6923187932376,9.18281955774556));
#47207=CARTESIAN_POINT('Ctrl Pts',(13.7209791439012,25.7078665937885,9.16434550060255));
#47208=CARTESIAN_POINT('Ctrl Pts',(13.7333406641673,25.7232888198184,9.1457834092639));
#47209=CARTESIAN_POINT('Ctrl Pts',(13.7345433154336,25.7247892468908,9.14397750495978));
#47210=CARTESIAN_POINT('Ctrl Pts',(13.7357459848049,25.726288457548,9.14217080098322));
#47211=CARTESIAN_POINT('Ctrl Pts',(13.7369486596423,25.7277864371561,9.14036331457088));
#47212=CARTESIAN_POINT('Ctrl Pts',(13.7655659843295,25.7634304595377,9.09735466092379));
#47213=CARTESIAN_POINT('Ctrl Pts',(13.7941628056774,25.7983490149194,9.05393888933006));
#47214=CARTESIAN_POINT('Ctrl Pts',(13.8227306450084,25.8325548745127,9.01011195910166));
#47215=CARTESIAN_POINT('Ctrl Pts',(13.842323756366,25.8560147941913,8.98005347569739));
#47216=CARTESIAN_POINT('Ctrl Pts',(13.8619031653407,25.8791397721896,8.94980169723303));
#47217=CARTESIAN_POINT('Ctrl Pts',(13.8814664318801,25.9019324890728,8.91935478464348));
#47218=CARTESIAN_POINT('Ctrl Pts',(13.9188560303246,25.9454942598026,8.86116420418492));
#47219=CARTESIAN_POINT('Ctrl Pts',(13.9561842683538,25.9878408888805,8.80226458048654));
#47220=CARTESIAN_POINT('Ctrl Pts',(13.9934294395427,26.0289848800641,8.74265020005614));
#47221=CARTESIAN_POINT('Ctrl Pts',(14.0052802435624,26.0420762248087,8.72368187968913));
#47222=CARTESIAN_POINT('Ctrl Pts',(14.0171226430049,26.0550458029487,8.70464119597399));
#47223=CARTESIAN_POINT('Ctrl Pts',(14.028956008926,26.0678936516663,8.68552782935395));
#47224=CARTESIAN_POINT('Ctrl Pts',(14.073645714307,26.1164146369712,8.6133445867516));
#47225=CARTESIAN_POINT('Ctrl Pts',(14.1182061758798,26.1632016095437,8.54012540763018));
#47226=CARTESIAN_POINT('Ctrl Pts',(14.1626036383006,26.2082576238332,8.46585247830341));
#47227=CARTESIAN_POINT('Ctrl Pts',(14.166909323044,26.2126271752164,8.45864945810322));
#47228=CARTESIAN_POINT('Ctrl Pts',(14.171213475128,26.2169804459483,8.45143652733002));
#47229=CARTESIAN_POINT('Ctrl Pts',(14.1755160662839,26.2213174218195,8.44421366298218));
#47230=CARTESIAN_POINT('Ctrl Pts',(14.2241842207673,26.2703745141725,8.36251324917115));
#47231=CARTESIAN_POINT('Ctrl Pts',(14.2726524536592,26.3173480640962,8.27954231106037));
#47232=CARTESIAN_POINT('Ctrl Pts',(14.3208797292034,26.3622200090052,8.19526716166835));
#47233=CARTESIAN_POINT('Ctrl Pts',(14.3238709484976,26.3650031193068,8.19004013090527));
#47234=CARTESIAN_POINT('Ctrl Pts',(14.3268612416092,26.3677781409806,8.1848080812505));
#47235=CARTESIAN_POINT('Ctrl Pts',(14.329850598655,26.3705450703243,8.17957100465716));
#47236=CARTESIAN_POINT('Ctrl Pts',(14.3750584922162,26.4123892011349,8.10037096345171));
#47237=CARTESIAN_POINT('Ctrl Pts',(14.4200523911715,26.4523826410612,8.02002135269682));
#47238=CARTESIAN_POINT('Ctrl Pts',(14.4648003758821,26.490492278629,7.93848543396106));
#47239=CARTESIAN_POINT('Ctrl Pts',(14.4748141458766,26.4990205095124,7.92023920585061));
#47240=CARTESIAN_POINT('Ctrl Pts',(14.4848156256028,26.5074542835796,7.90193352052972));
#47241=CARTESIAN_POINT('Ctrl Pts',(14.4948044563928,26.5157932364357,7.88356795942912));
#47242=CARTESIAN_POINT('Ctrl Pts',(14.5324037423552,26.547182162693,7.81443754785294));
#47243=CARTESIAN_POINT('Ctrl Pts',(14.5698238573549,26.5772277118277,7.74445888208727));
#47244=CARTESIAN_POINT('Ctrl Pts',(14.6070465811387,26.6058975693601,7.67360363343441));
#47245=CARTESIAN_POINT('Ctrl Pts',(14.6237799773867,26.6187860427897,7.64175080721871));
#47246=CARTESIAN_POINT('Ctrl Pts',(14.6404735352976,26.6313962194054,7.60972072029597));
#47247=CARTESIAN_POINT('Ctrl Pts',(14.6571256324194,26.6437250310917,7.57751068593594));
#47248=CARTESIAN_POINT('Ctrl Pts',(14.6839259713877,26.663567356647,7.52567097873781));
#47249=CARTESIAN_POINT('Ctrl Pts',(14.7106189563916,26.6826802627059,7.47336488375808));
#47250=CARTESIAN_POINT('Ctrl Pts',(14.7371979544204,26.7010468771463,7.42057925314658));
#47251=CARTESIAN_POINT('Ctrl Pts',(14.740599812746,26.703397628675,7.41382319572207));
#47252=CARTESIAN_POINT('Ctrl Pts',(14.7439998038026,26.7057361517508,7.40705928125229));
#47253=CARTESIAN_POINT('Ctrl Pts',(14.7473979137365,26.7080624063013,7.40028747986925));
#47254=CARTESIAN_POINT('Ctrl Pts',(14.7572628866864,26.7148157011212,7.38062842269809));
#47255=CARTESIAN_POINT('Ctrl Pts',(14.7671117981769,26.7214654268918,7.36090331359513));
#47256=CARTESIAN_POINT('Ctrl Pts',(14.7769448591095,26.7280110411829,7.3411103132182));
#47257=CARTESIAN_POINT('Ctrl Pts',(14.7786852863083,26.7291695985461,7.33760700164122));
#47258=CARTESIAN_POINT('Ctrl Pts',(14.7804252430215,26.7303249048412,7.3341015033297));
#47259=CARTESIAN_POINT('Ctrl Pts',(14.7821646285529,26.7314768936909,7.3305940181548));
#47260=CARTESIAN_POINT('Ctrl Pts',(14.78794790918,26.7353071398764,7.31893198538767));
#47261=CARTESIAN_POINT('Ctrl Pts',(14.7937273787648,26.7391023078568,7.3072429141235));
#47262=CARTESIAN_POINT('Ctrl Pts',(14.7994927953372,26.7428556865468,7.29554740361937));
#47263=CARTESIAN_POINT('Ctrl Pts',(14.8051580499374,26.7465438581858,7.28405507798198));
#47264=CARTESIAN_POINT('Ctrl Pts',(14.8108113279298,26.7501927519568,7.27255334308904));
#47265=CARTESIAN_POINT('Ctrl Pts',(14.816452375147,26.7538021411957,7.26104255703003));
#47266=CARTESIAN_POINT('Ctrl Pts',(14.8165521091315,26.75386595537,7.26083904578215));
#47267=CARTESIAN_POINT('Ctrl Pts',(14.8166518399196,26.7539297576608,7.26063553045111));
#47268=CARTESIAN_POINT('Ctrl Pts',(14.8167515675295,26.7539935480794,7.26043201099886));
#47269=CARTESIAN_POINT('Ctrl Pts',(14.8397132246179,26.7686808921284,7.21357293276645));
#47270=CARTESIAN_POINT('Ctrl Pts',(14.8624748126585,26.7827163343924,7.16655984206479));
#47271=CARTESIAN_POINT('Ctrl Pts',(14.8850347731502,26.7961020023305,7.11939232524414));
#47272=CARTESIAN_POINT('Ctrl Pts',(14.9301546941337,26.8228733382067,7.02505729160283));
#47273=CARTESIAN_POINT('Ctrl Pts',(14.9744681085358,26.8470455767767,6.93010455596954));
#47274=CARTESIAN_POINT('Ctrl Pts',(15.0179634542513,26.8686149665637,6.83452897348291));
#47275=CARTESIAN_POINT('Ctrl Pts',(15.0518694820136,26.8854290030292,6.76002471791515));
#47276=CARTESIAN_POINT('Ctrl Pts',(15.0852784766965,26.9006590046989,6.68514179979587));
#47277=CARTESIAN_POINT('Ctrl Pts',(15.11818516713,26.9142986900843,6.60987724941857));
#47278=CARTESIAN_POINT('Ctrl Pts',(15.1274918520523,26.9181562720121,6.58859089558124));
#47279=CARTESIAN_POINT('Ctrl Pts',(15.1367583557927,26.921886293869,6.5672739825884));
#47280=CARTESIAN_POINT('Ctrl Pts',(15.1459845498898,26.9254881988036,6.54592640551724));
#47281=CARTESIAN_POINT('Ctrl Pts',(15.1844555772193,26.9405072826993,6.45691210424756));
#47282=CARTESIAN_POINT('Ctrl Pts',(15.2222256053613,26.9533040744962,6.36736498601499));
#47283=CARTESIAN_POINT('Ctrl Pts',(15.2592854167753,26.963841419386,6.2772771620655));
#47284=CARTESIAN_POINT('Ctrl Pts',(15.2625387870946,26.964766461468,6.26936862067291));
#47285=CARTESIAN_POINT('Ctrl Pts',(15.2657866840963,26.965674091811,6.2614559125951));
#47286=CARTESIAN_POINT('Ctrl Pts',(15.269029101094,26.966564271014,6.25353903103056));
#47287=CARTESIAN_POINT('Ctrl Pts',(15.3092065579625,26.977594664871,6.15543932089992));
#47288=CARTESIAN_POINT('Ctrl Pts',(15.3485425859871,26.9859469157609,6.05669887485067));
#47289=CARTESIAN_POINT('Ctrl Pts',(15.3870245205822,26.9915481270336,5.9573044625394));
#47290=CARTESIAN_POINT('Ctrl Pts',(15.3892689468374,26.9918748129389,5.95150736759178));
#47291=CARTESIAN_POINT('Ctrl Pts',(15.3915104679287,26.9921921361717,5.94570804740638));
#47292=CARTESIAN_POINT('Ctrl Pts',(15.3937490813168,26.9925000827492,5.93990649938684));
#47293=CARTESIAN_POINT('Ctrl Pts',(15.4298927376898,26.9974720512608,5.84623728470405));
#47294=CARTESIAN_POINT('Ctrl Pts',(15.4652784277793,26.9999999999997,5.75198738946509));
#47295=CARTESIAN_POINT('Ctrl Pts',(15.4998946833985,27.,5.65714286308472));
#47296=CARTESIAN_POINT('',(16.4260329799192,25.1379309923314,1.56059116342174));
#47297=CARTESIAN_POINT('Ctrl Pts',(15.4998966741159,26.9999999999935,5.65714358966582));
#47298=CARTESIAN_POINT('Ctrl Pts',(15.4605694492474,27.0857112046842,5.76489474592549));
#47299=CARTESIAN_POINT('Ctrl Pts',(15.4207785141578,27.1734809441547,5.87042507646245));
#47300=CARTESIAN_POINT('Ctrl Pts',(15.3806244193455,27.2632762176172,5.97380887466604));
#47301=CARTESIAN_POINT('Ctrl Pts',(15.3782691166024,27.2685433032006,5.97987301693189));
#47302=CARTESIAN_POINT('Ctrl Pts',(15.3759125601364,27.2738173579326,5.98592977147193));
#47303=CARTESIAN_POINT('Ctrl Pts',(15.3735547702585,27.2790983825627,5.99197914719141));
#47304=CARTESIAN_POINT('Ctrl Pts',(15.3310004839505,27.3744123188118,6.10116057542921));
#47305=CARTESIAN_POINT('Ctrl Pts',(15.2880444697824,27.4719959961733,6.20793920008953));
#47306=CARTESIAN_POINT('Ctrl Pts',(15.2447991620941,27.5718319675762,6.31237932440066));
#47307=CARTESIAN_POINT('Ctrl Pts',(15.2015538544059,27.6716679389791,6.41681944871178));
#47308=CARTESIAN_POINT('Ctrl Pts',(15.1580191426619,27.7737562144739,6.51892100698712));
#47309=CARTESIAN_POINT('Ctrl Pts',(15.1143112165841,27.878098848085,6.61873074046543));
#47310=CARTESIAN_POINT('Ctrl Pts',(15.1126633328231,27.8820327920385,6.62249378423699));
#47311=CARTESIAN_POINT('Ctrl Pts',(15.1110152005509,27.8859699339714,6.62625357479283));
#47312=CARTESIAN_POINT('Ctrl Pts',(15.1093668257744,27.8899102732374,6.63001011493869));
#47313=CARTESIAN_POINT('Ctrl Pts',(15.067294250942,27.9904821947445,6.72589080824484));
#47314=CARTESIAN_POINT('Ctrl Pts',(15.0250644654567,28.0931422469056,6.81965016197501));
#47315=CARTESIAN_POINT('Ctrl Pts',(14.9827816132864,28.1979088402624,6.91131356524541));
#47316=CARTESIAN_POINT('Ctrl Pts',(14.9787573508417,28.207879980937,6.92003761228592));
#47317=CARTESIAN_POINT('Ctrl Pts',(14.9747326086664,28.2178702120797,6.92874266722994));
#47318=CARTESIAN_POINT('Ctrl Pts',(14.9707074756758,28.2278795472534,6.93742875118335));
#47319=CARTESIAN_POINT('Ctrl Pts',(14.952758123344,28.2725143665395,6.97616277105936));
#47320=CARTESIAN_POINT('Ctrl Pts',(14.9348010697903,28.317529336006,7.01451936651037));
#47321=CARTESIAN_POINT('Ctrl Pts',(14.9168444926374,28.3629268553635,7.05249958405971));
#47322=CARTESIAN_POINT('Ctrl Pts',(14.9115517161979,28.3763079646263,7.06369441250069));
#47323=CARTESIAN_POINT('Ctrl Pts',(14.9062586162459,28.3897232443503,7.07485731092418));
#47324=CARTESIAN_POINT('Ctrl Pts',(14.900965620398,28.4031722110485,7.08598783372623));
#47325=CARTESIAN_POINT('Ctrl Pts',(14.8952664954411,28.4176531107047,7.09797239636471));
#47326=CARTESIAN_POINT('Ctrl Pts',(14.8895690962475,28.4321690472932,7.10991600819615));
#47327=CARTESIAN_POINT('Ctrl Pts',(14.8838763075017,28.4467132589687,7.12181336541017));
#47328=CARTESIAN_POINT('Ctrl Pts',(14.877938180411,28.4618842728988,7.13422345514567));
#47329=CARTESIAN_POINT('Ctrl Pts',(14.8720042057682,28.4770882994026,7.14658502557187));
#47330=CARTESIAN_POINT('Ctrl Pts',(14.8660770570502,28.4923191860082,7.15889327576865));
#47331=CARTESIAN_POINT('Ctrl Pts',(14.8610446054279,28.5052509857072,7.16934360806462));
#47332=CARTESIAN_POINT('Ctrl Pts',(14.8560159746172,28.5182049390111,7.17975781925992));
#47333=CARTESIAN_POINT('Ctrl Pts',(14.8509911673286,28.5311814410601,7.19013639432679));
#47334=CARTESIAN_POINT('Ctrl Pts',(14.8444171067273,28.5481588704351,7.20371490142723));
#47335=CARTESIAN_POINT('Ctrl Pts',(14.8378500820084,28.5651738792742,7.21723139465462));
#47336=CARTESIAN_POINT('Ctrl Pts',(14.8312904741886,28.5822263963677,7.23068619636096));
#47337=CARTESIAN_POINT('Ctrl Pts',(14.7941745019158,28.678713986635,7.30681697441842));
#47338=CARTESIAN_POINT('Ctrl Pts',(14.7572952651303,28.7763985017568,7.38097825825209));
#47339=CARTESIAN_POINT('Ctrl Pts',(14.7207229839317,28.8752782662337,7.45321250522372));
#47340=CARTESIAN_POINT('Ctrl Pts',(14.6776871829316,28.9916333233289,7.53821290925047));
#47341=CARTESIAN_POINT('Ctrl Pts',(14.6350754185611,29.1096418353901,7.62054685582819));
#47342=CARTESIAN_POINT('Ctrl Pts',(14.5930071299595,29.2293096316852,7.70026989277396));
#47343=CARTESIAN_POINT('Ctrl Pts',(14.5814101538139,29.2622984844567,7.72224716326552));
#47344=CARTESIAN_POINT('Ctrl Pts',(14.5698545944106,29.2954136234644,7.74402578590885));
#47345=CARTESIAN_POINT('Ctrl Pts',(14.5583428293979,29.3286549581115,7.76560712769879));
#47346=CARTESIAN_POINT('Ctrl Pts',(14.5280954110866,29.4159973033722,7.82231258269372));
#47347=CARTESIAN_POINT('Ctrl Pts',(14.4981498437657,29.5042107576476,7.87765592020842));
#47348=CARTESIAN_POINT('Ctrl Pts',(14.4685529155124,29.5933054917983,7.93164594712575));
#47349=CARTESIAN_POINT('Ctrl Pts',(14.4276917901088,29.7163084964947,8.00618386003138));
#47350=CARTESIAN_POINT('Ctrl Pts',(14.3874934405528,29.8409884290493,8.0781455526749));
#47351=CARTESIAN_POINT('Ctrl Pts',(14.348083905333,29.9673763912336,8.14754584487634));
#47352=CARTESIAN_POINT('Ctrl Pts',(14.3318729112048,30.0193657004558,8.17609344695027));
#47353=CARTESIAN_POINT('Ctrl Pts',(14.3157957407696,30.0716445884368,8.20420699797485));
#47354=CARTESIAN_POINT('Ctrl Pts',(14.2998608525879,30.1242146835024,8.2318879727946));
#47355=CARTESIAN_POINT('Ctrl Pts',(14.2770574294696,30.1994444628066,8.27150048679177));
#47356=CARTESIAN_POINT('Ctrl Pts',(14.2545460134195,30.2752720256852,8.31022525165558));
#47357=CARTESIAN_POINT('Ctrl Pts',(14.2323537327013,30.3517071915215,8.34806018280675));
#47358=CARTESIAN_POINT('Ctrl Pts',(14.214138504925,30.4144444997552,8.37911475973689));
#47359=CARTESIAN_POINT('Ctrl Pts',(14.1961383970943,30.4775913242493,8.40956964533723));
#47360=CARTESIAN_POINT('Ctrl Pts',(14.1783685323836,30.5411531688201,8.43942330730726));
#47361=CARTESIAN_POINT('Ctrl Pts',(14.1593600597948,30.609145446752,8.47135785067454));
#47362=CARTESIAN_POINT('Ctrl Pts',(14.1406150048816,30.6776125759273,8.50260447704652));
#47363=CARTESIAN_POINT('Ctrl Pts',(14.1221532487268,30.7465637771849,8.53315820493967));
#47364=CARTESIAN_POINT('Ctrl Pts',(14.1022298693507,30.8209738674047,8.56613088137767));
#47365=CARTESIAN_POINT('Ctrl Pts',(14.0826363732492,30.8959476343974,8.59829668510921));
#47366=CARTESIAN_POINT('Ctrl Pts',(14.0633976982587,30.9714964270601,8.62964919221027));
#47367=CARTESIAN_POINT('Ctrl Pts',(14.0481434474469,31.0313986933219,8.65450844094409));
#47368=CARTESIAN_POINT('Ctrl Pts',(14.033112419075,31.0916627211746,8.67885607314034));
#47369=CARTESIAN_POINT('Ctrl Pts',(14.0183177786232,31.1522954179624,8.70268732550796));
#47370=CARTESIAN_POINT('Ctrl Pts',(14.015101549896,31.1654764494213,8.70786803663916));
#47371=CARTESIAN_POINT('Ctrl Pts',(14.0118965191854,31.1786747841575,8.71302430103908));
#47372=CARTESIAN_POINT('Ctrl Pts',(14.0087028170895,31.191890502718,8.71815607697348));
#47373=CARTESIAN_POINT('Ctrl Pts',(13.999750872967,31.2289341500401,8.73254044033435));
#47374=CARTESIAN_POINT('Ctrl Pts',(13.9908879533214,31.2661144055239,8.74673237050487));
#47375=CARTESIAN_POINT('Ctrl Pts',(13.9821170337287,31.303433206279,8.76073074892257));
#47376=CARTESIAN_POINT('Ctrl Pts',(13.9777432789681,31.3220428036803,8.76771125690659));
#47377=CARTESIAN_POINT('Ctrl Pts',(13.9733909131801,31.3406934119555,8.77464599131914));
#47378=CARTESIAN_POINT('Ctrl Pts',(13.9690630125404,31.3593734023405,8.78153052202542));
#47379=CARTESIAN_POINT('Ctrl Pts',(13.9650372173515,31.3767494517654,8.78793448387731));
#47380=CARTESIAN_POINT('Ctrl Pts',(13.961030484189,31.3941600858426,8.79429835191505));
#47381=CARTESIAN_POINT('Ctrl Pts',(13.9570487976368,31.4115807756301,8.80061298178852));
#47382=CARTESIAN_POINT('Ctrl Pts',(13.9567217978581,31.4130114662759,8.80113157674668));
#47383=CARTESIAN_POINT('Ctrl Pts',(13.9563949570268,31.4144422679483,8.80164985548056));
#47384=CARTESIAN_POINT('Ctrl Pts',(13.9560682763309,31.4158731763214,8.80216781630477));
#47385=CARTESIAN_POINT('Ctrl Pts',(13.9524171557598,31.4318656088748,8.80795676387294));
#47386=CARTESIAN_POINT('Ctrl Pts',(13.9487865760586,31.4478688324497,8.81370518755723));
#47387=CARTESIAN_POINT('Ctrl Pts',(13.9451764341561,31.4638840446531,8.81941354815297));
#47388=CARTESIAN_POINT('Ctrl Pts',(13.9373101220175,31.4987803621828,8.83185177010061));
#47389=CARTESIAN_POINT('Ctrl Pts',(13.92954125731,31.533731632952,8.84409912661643));
#47390=CARTESIAN_POINT('Ctrl Pts',(13.9218713056012,31.568737905583,8.85615636330126));
#47391=CARTESIAN_POINT('Ctrl Pts',(13.8999348550734,31.6688576190942,8.89064067116655));
#47392=CARTESIAN_POINT('Ctrl Pts',(13.8788078574992,31.7694274729138,8.92356928315047));
#47393=CARTESIAN_POINT('Ctrl Pts',(13.8585278428624,31.8704501006104,8.95495427283813));
#47394=CARTESIAN_POINT('Ctrl Pts',(13.8504447031737,31.9107153581073,8.96746359594845));
#47395=CARTESIAN_POINT('Ctrl Pts',(13.8424960957031,31.951052419582,8.97972818763168));
#47396=CARTESIAN_POINT('Ctrl Pts',(13.8346844161992,31.9914616384529,8.99174802005895));
#47397=CARTESIAN_POINT('Ctrl Pts',(13.807273796088,32.1332546737276,9.03392474534529));
#47398=CARTESIAN_POINT('Ctrl Pts',(13.7815485167864,32.2759361339262,9.0730889007526));
#47399=CARTESIAN_POINT('Ctrl Pts',(13.7576063783065,32.4195184154285,9.10924700295637));
#47400=CARTESIAN_POINT('Ctrl Pts',(13.7365494340305,32.5457980333979,9.14104780236572));
#47401=CARTESIAN_POINT('Ctrl Pts',(13.716872430334,32.6727747711858,9.17052232737716));
#47402=CARTESIAN_POINT('Ctrl Pts',(13.6986465683587,32.8004595027004,9.1976672148543));
#47403=CARTESIAN_POINT('Ctrl Pts',(13.6961492852466,32.8179546930028,9.20138657085338));
#47404=CARTESIAN_POINT('Ctrl Pts',(13.6936792456254,32.8354631714845,9.20506219838908));
#47405=CARTESIAN_POINT('Ctrl Pts',(13.6912366347723,32.8529849844081,9.20869400810665));
#47406=CARTESIAN_POINT('Ctrl Pts',(13.6709671751925,32.9983858280898,9.23883176835602));
#47407=CARTESIAN_POINT('Ctrl Pts',(13.6525860055183,33.1447047525089,9.2659530160941));
#47408=CARTESIAN_POINT('Ctrl Pts',(13.6361884527326,33.2919630415462,9.29002162328209));
#47409=CARTESIAN_POINT('Ctrl Pts',(13.6197908999469,33.4392213305834,9.31409023047008));
#47410=CARTESIAN_POINT('Ctrl Pts',(13.6053769480128,33.5874190011587,9.33510616152985));
#47411=CARTESIAN_POINT('Ctrl Pts',(13.5930518504658,33.7365821076625,9.35301783205155));
#47412=CARTESIAN_POINT('Ctrl Pts',(13.5924247354764,33.7441716962714,9.35392919823146));
#47413=CARTESIAN_POINT('Ctrl Pts',(13.5918030226177,33.7517637632298,9.3548325359547));
#47414=CARTESIAN_POINT('Ctrl Pts',(13.5911867246683,33.7593583129635,9.35572783994931));
#47415=CARTESIAN_POINT('Ctrl Pts',(13.5845976814368,33.8405541315953,9.36529982819296));
#47416=CARTESIAN_POINT('Ctrl Pts',(13.5786276639973,33.9220343469512,9.37395107782386));
#47417=CARTESIAN_POINT('Ctrl Pts',(13.5732924325667,34.0038056340085,9.38167002937256));
#47418=CARTESIAN_POINT('Ctrl Pts',(13.5706230872623,34.0447177863659,9.38553200749673));
#47419=CARTESIAN_POINT('Ctrl Pts',(13.5681126448878,34.0857028095819,9.3891605744006));
#47420=CARTESIAN_POINT('Ctrl Pts',(13.5657630841551,34.1267615927872,9.39255406929206));
#47421=CARTESIAN_POINT('Ctrl Pts',(13.5646152616427,34.1468198934904,9.39421188123031));
#47422=CARTESIAN_POINT('Ctrl Pts',(13.5635054330467,34.1669044611196,9.39581417050262));
#47423=CARTESIAN_POINT('Ctrl Pts',(13.562434633342,34.1869983310107,9.39735956752719));
#47424=CARTESIAN_POINT('Ctrl Pts',(13.5614279561067,34.2058889239908,9.39881242187242));
#47425=CARTESIAN_POINT('Ctrl Pts',(13.5604553138571,34.2247967000574,9.40021565665452));
#47426=CARTESIAN_POINT('Ctrl Pts',(13.5595183430496,34.2436929639982,9.40156701329765));
#47427=CARTESIAN_POINT('Ctrl Pts',(13.5594112076896,34.2458536055287,9.40172153047071));
#47428=CARTESIAN_POINT('Ctrl Pts',(13.5593045331735,34.2480141986753,9.40187537735987));
#47429=CARTESIAN_POINT('Ctrl Pts',(13.5591983208464,34.2501747229023,9.4020285521773));
#47430=CARTESIAN_POINT('Ctrl Pts',(13.5583756349098,34.2669094367188,9.40321499419979));
#47431=CARTESIAN_POINT('Ctrl Pts',(13.5575806104702,34.2836402092014,9.40436124872476));
#47432=CARTESIAN_POINT('Ctrl Pts',(13.5568132309541,34.3003672974803,9.40546738423807));
#47433=CARTESIAN_POINT('Ctrl Pts',(13.555080327866,34.3381405535122,9.40796526906137));
#47434=CARTESIAN_POINT('Ctrl Pts',(13.5534883604341,34.375894555659,9.41025862411392));
#47435=CARTESIAN_POINT('Ctrl Pts',(13.5520369777938,34.4136293845627,9.4123484688034));
#47436=CARTESIAN_POINT('Ctrl Pts',(13.5491342125133,34.4890990423703,9.41652815818236));
#47437=CARTESIAN_POINT('Ctrl Pts',(13.5467937861962,34.564492007726,9.41989380592011));
#47438=CARTESIAN_POINT('Ctrl Pts',(13.5450131527534,34.639808895649,9.42245319556493));
#47439=CARTESIAN_POINT('Ctrl Pts',(13.5442006828786,34.6741745887956,9.42362099739002));
#47440=CARTESIAN_POINT('Ctrl Pts',(13.5435048599725,34.7085244273738,9.42462079538545));
#47441=CARTESIAN_POINT('Ctrl Pts',(13.5429254222363,34.7428584709684,9.42545335820768));
#47442=CARTESIAN_POINT('Ctrl Pts',(13.5409650335913,34.8590194749976,9.42827013488828));
#47443=CARTESIAN_POINT('Ctrl Pts',(13.5403378655916,34.9749998595297,9.4291761058855));
#47444=CARTESIAN_POINT('Ctrl Pts',(13.5410293473817,35.0908012044776,9.42818546292229));
#47445=CARTESIAN_POINT('Ctrl Pts',(13.5419252124423,35.2408302875462,9.4269020127561));
#47446=CARTESIAN_POINT('Ctrl Pts',(13.545033190514,35.3905590014421,9.4224368778565));
#47447=CARTESIAN_POINT('Ctrl Pts',(13.5503249881556,35.5399902323981,9.41481602126595));
#47448=CARTESIAN_POINT('Ctrl Pts',(13.5524631372416,35.6003678718186,9.4117368166823));
#47449=CARTESIAN_POINT('Ctrl Pts',(13.5549580993085,35.6606969039799,9.40814200182775));
#47450=CARTESIAN_POINT('Ctrl Pts',(13.5578078379326,35.7209775476613,9.40403352980553));
#47451=CARTESIAN_POINT('Ctrl Pts',(13.562011040672,35.8098880759867,9.3979737667407));
#47452=CARTESIAN_POINT('Ctrl Pts',(13.566985985049,35.8986933353278,9.39079652578675));
#47453=CARTESIAN_POINT('Ctrl Pts',(13.5727235618244,35.9873935429952,9.38249904885336));
#47454=CARTESIAN_POINT('Ctrl Pts',(13.5823511708345,36.1362317985809,9.36857594737473));
#47455=CARTESIAN_POINT('Ctrl Pts',(13.5941242809196,36.2847745196704,9.35150127372894));
#47456=CARTESIAN_POINT('Ctrl Pts',(13.6080006813988,36.4330226315577,9.33126069412123));
#47457=CARTESIAN_POINT('Ctrl Pts',(13.6160160175688,36.5186542371842,9.31956925799733));
#47458=CARTESIAN_POINT('Ctrl Pts',(13.6247337631313,36.6041874492391,9.30682057126));
#47459=CARTESIAN_POINT('Ctrl Pts',(13.6341456855963,36.6896224774574,9.29301196727616));
#47460=CARTESIAN_POINT('Ctrl Pts',(13.6410279774516,36.7520952401738,9.28291468448575));
#47461=CARTESIAN_POINT('Ctrl Pts',(13.6482810994821,36.8145154277135,9.27224936331575));
#47462=CARTESIAN_POINT('Ctrl Pts',(13.6559013066663,36.8768830050661,9.26101289493422));
#47463=CARTESIAN_POINT('Ctrl Pts',(13.658078080858,36.8946988110537,9.25780310630416));
#47464=CARTESIAN_POINT('Ctrl Pts',(13.6602848252828,36.9125104930323,9.25454668824333));
#47465=CARTESIAN_POINT('Ctrl Pts',(13.6625214262135,36.9303178286985,9.25124360711876));
#47466=CARTESIAN_POINT('Ctrl Pts',(13.6675536560891,36.9703833608706,9.24381185508443));
#47467=CARTESIAN_POINT('Ctrl Pts',(13.6727370256631,37.0104268883538,9.23614384654524));
#47468=CARTESIAN_POINT('Ctrl Pts',(13.6780701456487,37.0504458776819,9.22823911105019));
#47469=CARTESIAN_POINT('Ctrl Pts',(13.6801894433611,37.0663487924424,9.22509789392069));
#47470=CARTESIAN_POINT('Ctrl Pts',(13.6823330914514,37.082252742982,9.22191824754957));
#47471=CARTESIAN_POINT('Ctrl Pts',(13.6844999020291,37.0981498912587,9.21870177221577));
#47472=CARTESIAN_POINT('Ctrl Pts',(13.6870106441776,37.1165703478635,9.21497475506304));
#47473=CARTESIAN_POINT('Ctrl Pts',(13.6895539090126,37.1349919943203,9.21119617473931));
#47474=CARTESIAN_POINT('Ctrl Pts',(13.692126041947,37.153389257747,9.20737120104998));
#47475=CARTESIAN_POINT('Ctrl Pts',(13.6929190136733,37.159061013488,9.20619198672997));
#47476=CARTESIAN_POINT('Ctrl Pts',(13.6937147748413,37.1647308023172,9.20500829519152));
#47477=CARTESIAN_POINT('Ctrl Pts',(13.6945132874207,37.1703983687995,9.20382017537598));
#47478=CARTESIAN_POINT('Ctrl Pts',(13.6963048804354,37.1831144772008,9.20115443507714));
#47479=CARTESIAN_POINT('Ctrl Pts',(13.6981102581906,37.1958192091792,9.19846651393387));
#47480=CARTESIAN_POINT('Ctrl Pts',(13.6999295033177,37.2085136766366,9.19575620104296));
#47481=CARTESIAN_POINT('Ctrl Pts',(13.7051896678105,37.2452184537887,9.18791960364278));
#47482=CARTESIAN_POINT('Ctrl Pts',(13.7105651593549,37.2818337180102,9.17989671027503));
#47483=CARTESIAN_POINT('Ctrl Pts',(13.7160536764026,37.3183604197314,9.17168881921092));
#47484=CARTESIAN_POINT('Ctrl Pts',(13.7324696154778,37.4276103509729,9.14713933918296));
#47485=CARTESIAN_POINT('Ctrl Pts',(13.749897166982,37.536067723453,9.1209341917559));
#47486=CARTESIAN_POINT('Ctrl Pts',(13.7682796425987,37.6437540820578,9.09310044392041));
#47487=CARTESIAN_POINT('Ctrl Pts',(13.7744812082209,37.6800834662732,9.08371036951942));
#47488=CARTESIAN_POINT('Ctrl Pts',(13.7807913364897,37.7163252869045,9.07413535277473));
#47489=CARTESIAN_POINT('Ctrl Pts',(13.7872080111268,37.7524800859917,9.06437582107082));
#47490=CARTESIAN_POINT('Ctrl Pts',(13.8126447804049,37.8958037442233,9.0256874084189));
#47491=CARTESIAN_POINT('Ctrl Pts',(13.8397556926634,38.0377606814329,8.98409980770552));
#47492=CARTESIAN_POINT('Ctrl Pts',(13.868407440965,38.178392692106,8.9396504174699));
#47493=CARTESIAN_POINT('Ctrl Pts',(13.8944482538081,38.3062093904499,8.8992515475674));
#47494=CARTESIAN_POINT('Ctrl Pts',(13.9217625847717,38.4329310416233,8.8564876540994));
#47495=CARTESIAN_POINT('Ctrl Pts',(13.9502567594613,38.5585839638948,8.81137539463128));
#47496=CARTESIAN_POINT('Ctrl Pts',(13.9531136768512,38.5711823290918,8.80685229473544));
#47497=CARTESIAN_POINT('Ctrl Pts',(13.9559824579279,38.5837699469257,8.80230558332653));
#47498=CARTESIAN_POINT('Ctrl Pts',(13.9588630164218,38.5963468272929,8.79773524200746));
#47499=CARTESIAN_POINT('Ctrl Pts',(13.990473540025,38.7343623456489,8.74758146716013));
#47500=CARTESIAN_POINT('Ctrl Pts',(14.0235015619679,38.8710858072657,8.69458344629727));
#47501=CARTESIAN_POINT('Ctrl Pts',(14.0578212325299,39.0065423683161,8.6387349163809));
#47502=CARTESIAN_POINT('Ctrl Pts',(14.0921409030919,39.1419989293664,8.58288638646454));
#47503=CARTESIAN_POINT('Ctrl Pts',(14.1277522803669,39.2761886042384,8.52418741505491));
#47504=CARTESIAN_POINT('Ctrl Pts',(14.164539316697,39.4091280855466,8.46261347849984));
#47505=CARTESIAN_POINT('Ctrl Pts',(14.1667788306083,39.4172211489582,8.45886499258629));
#47506=CARTESIAN_POINT('Ctrl Pts',(14.1690226941704,39.4253095865658,8.45510586318291));
#47507=CARTESIAN_POINT('Ctrl Pts',(14.1712708793468,39.4333934036186,8.45133608751763));
#47508=CARTESIAN_POINT('Ctrl Pts',(14.1874874309478,39.4917033852633,8.4241440384631));
#47509=CARTESIAN_POINT('Ctrl Pts',(14.2039291632183,39.5497722972026,8.39639657437115));
#47510=CARTESIAN_POINT('Ctrl Pts',(14.220586013407,39.6076010566071,8.36809019771358));
#47511=CARTESIAN_POINT('Ctrl Pts',(14.2242846970821,39.620442037101,8.36180471564109));
#47512=CARTESIAN_POINT('Ctrl Pts',(14.2279940116495,39.6332712521396,8.35549163407334));
#47513=CARTESIAN_POINT('Ctrl Pts',(14.2317138707491,39.6460887874945,8.34915087306062));
#47514=CARTESIAN_POINT('Ctrl Pts',(14.2375313413513,39.6661340723086,8.33923458596492));
#47515=CARTESIAN_POINT('Ctrl Pts',(14.2433757952081,39.6861546944092,8.32924851654006));
#47516=CARTESIAN_POINT('Ctrl Pts',(14.2492418576234,39.7061341133082,8.31920104913758));
#47517=CARTESIAN_POINT('Ctrl Pts',(14.2536890975557,39.7212811170836,8.31158375919293));
#47518=CARTESIAN_POINT('Ctrl Pts',(14.2581484788514,39.736403444488,8.30393165731456));
#47519=CARTESIAN_POINT('Ctrl Pts',(14.2626178939433,39.7514947403366,8.29624799601414));
#47520=CARTESIAN_POINT('Ctrl Pts',(14.2678134243439,39.7690378158295,8.28731602280211));
#47521=CARTESIAN_POINT('Ctrl Pts',(14.2730238234764,39.7865435386285,8.27833918385668));
#47522=CARTESIAN_POINT('Ctrl Pts',(14.2782491820152,39.8040136477705,8.26931679747083));
#47523=CARTESIAN_POINT('Ctrl Pts',(14.2834414501267,39.8213731246233,8.26035154680477));
#47524=CARTESIAN_POINT('Ctrl Pts',(14.2886481552757,39.8386962121138,8.25134189848024));
#47525=CARTESIAN_POINT('Ctrl Pts',(14.2938689492472,39.8559830980089,8.2422879385366));
#47526=CARTESIAN_POINT('Ctrl Pts',(14.32774350029,39.9681471676544,8.18354230905482));
#47527=CARTESIAN_POINT('Ctrl Pts',(14.3622105379506,40.07878847771,8.12293253524994));
#47528=CARTESIAN_POINT('Ctrl Pts',(14.3971792690442,40.1879497097792,8.06047326532415));
#47529=CARTESIAN_POINT('Ctrl Pts',(14.4053895058454,40.2135794520311,8.04580858117672));
#47530=CARTESIAN_POINT('Ctrl Pts',(14.4136274917622,40.2391274299263,8.03104176990634));
#47531=CARTESIAN_POINT('Ctrl Pts',(14.4218920252206,40.2645942448818,8.01617305282824));
#47532=CARTESIAN_POINT('Ctrl Pts',(14.454252553542,40.3643118624307,7.95795324616492));
#47533=CARTESIAN_POINT('Ctrl Pts',(14.4870188730222,40.4627881460053,7.89817432298111));
#47534=CARTESIAN_POINT('Ctrl Pts',(14.5201258358726,40.5600444217448,7.8368339102019));
#47535=CARTESIAN_POINT('Ctrl Pts',(14.5616879635914,40.6821389120185,7.75982781085761));
#47536=CARTESIAN_POINT('Ctrl Pts',(14.6037856063819,40.8023132277205,7.68036347799239));
#47537=CARTESIAN_POINT('Ctrl Pts',(14.6462939201702,40.9206016188664,7.59842619851696));
#47538=CARTESIAN_POINT('Ctrl Pts',(14.6605297485143,40.9602158279793,7.5709858005891));
#47539=CARTESIAN_POINT('Ctrl Pts',(14.6748118124644,40.9996181534556,7.54326767465988));
#47540=CARTESIAN_POINT('Ctrl Pts',(14.6891352187837,41.0388102533568,7.51527155359934));
#47541=CARTESIAN_POINT('Ctrl Pts',(14.7175816348888,41.1166461226299,7.45967100082168));
#47542=CARTESIAN_POINT('Ctrl Pts',(14.7461916611224,41.1936525631517,7.40297395014157));
#47543=CARTESIAN_POINT('Ctrl Pts',(14.7749303180739,41.2698321114896,7.34516658947509));
#47544=CARTESIAN_POINT('Ctrl Pts',(14.8181395311428,41.384369765117,7.25825193065136));
#47545=CARTESIAN_POINT('Ctrl Pts',(14.8616378266614,41.4970416057414,7.16883096877626));
#47546=CARTESIAN_POINT('Ctrl Pts',(14.9053081022752,41.6078521323305,7.07685057936598));
#47547=CARTESIAN_POINT('Ctrl Pts',(14.9252103018943,41.6583526888091,7.03493163002678));
#47548=CARTESIAN_POINT('Ctrl Pts',(14.9451486273982,41.7084657999447,6.99248017876618));
#47549=CARTESIAN_POINT('Ctrl Pts',(14.9651116680086,41.7581924532683,6.9494915471597));
#47550=CARTESIAN_POINT('Ctrl Pts',(14.9889524029723,41.8175781944316,6.89815264580769));
#47551=CARTESIAN_POINT('Ctrl Pts',(15.0128287365156,41.8764113900424,6.84604605414212));
#47552=CARTESIAN_POINT('Ctrl Pts',(15.0367217535436,41.9346894966983,6.7931586175325));
#47553=CARTESIAN_POINT('Ctrl Pts',(15.0586716715574,41.988228137783,6.74457225038686));
#47554=CARTESIAN_POINT('Ctrl Pts',(15.080635583353,42.0412985081664,6.69532707559198));
#47555=CARTESIAN_POINT('Ctrl Pts',(15.1025992182023,42.0938977223522,6.64541171525283));
#47556=CARTESIAN_POINT('Ctrl Pts',(15.1031379467204,42.0951878866127,6.64418738110714));
#47557=CARTESIAN_POINT('Ctrl Pts',(15.1036766779631,42.0964777746802,6.64296263716632));
#47558=CARTESIAN_POINT('Ctrl Pts',(15.1042154112924,42.0977673854986,6.64173748421894));
#47559=CARTESIAN_POINT('Ctrl Pts',(15.1146585934605,42.1227661000223,6.61798826597259));
#47560=CARTESIAN_POINT('Ctrl Pts',(15.125102165282,42.1476594144795,6.59408588091983));
#47561=CARTESIAN_POINT('Ctrl Pts',(15.1355215378525,42.1723927739372,6.57008277606289));
#47562=CARTESIAN_POINT('Ctrl Pts',(15.1366606880725,42.1750968726416,6.56745851610917));
#47563=CARTESIAN_POINT('Ctrl Pts',(15.1377995943815,42.1777991668441,6.56483294813743));
#47564=CARTESIAN_POINT('Ctrl Pts',(15.1389382253939,42.1804995871324,6.56220613876985));
#47565=CARTESIAN_POINT('Ctrl Pts',(15.1487514780318,42.203773067505,6.53956707161244));
#47566=CARTESIAN_POINT('Ctrl Pts',(15.1585492995077,42.2269193893911,6.5168244186884));
#47567=CARTESIAN_POINT('Ctrl Pts',(15.1683284209863,42.249934449691,6.49398282359018));
#47568=CARTESIAN_POINT('Ctrl Pts',(15.1700553459567,42.2539987495787,6.489949156453));
#47569=CARTESIAN_POINT('Ctrl Pts',(15.1717817099298,42.258059005505,6.48591235260955));
#47570=CARTESIAN_POINT('Ctrl Pts',(15.1735075060744,42.2621152203853,6.48187241181925));
#47571=CARTESIAN_POINT('Ctrl Pts',(15.1964839485354,42.3161177676152,6.42808653021052));
#47572=CARTESIAN_POINT('Ctrl Pts',(15.2193597296865,42.3694041467529,6.37374468565707));
#47573=CARTESIAN_POINT('Ctrl Pts',(15.2421189807697,42.4219798813043,6.31884554139977));
#47574=CARTESIAN_POINT('Ctrl Pts',(15.2608644872042,42.4652835368918,6.27362822479454));
#47575=CARTESIAN_POINT('Ctrl Pts',(15.2795307517416,42.508106509307,6.22803369293663));
#47576=CARTESIAN_POINT('Ctrl Pts',(15.2981092430933,42.5504495124992,6.18205979987793));
#47577=CARTESIAN_POINT('Ctrl Pts',(15.3409384613079,42.6480633439594,6.07607563460213));
#47578=CARTESIAN_POINT('Ctrl Pts',(15.3833002938721,42.7431310467078,5.968077837435));
#47579=CARTESIAN_POINT('Ctrl Pts',(15.4250886320099,42.8356685001976,5.85804219315313));
#47580=CARTESIAN_POINT('Ctrl Pts',(15.4529471198793,42.897359240734,5.78468616135029));
#47581=CARTESIAN_POINT('Ctrl Pts',(15.4805511466514,42.9579234845588,5.71042330098948));
#47582=CARTESIAN_POINT('Ctrl Pts',(15.5078694486391,43.017364224858,5.63524490719013));
#47583=CARTESIAN_POINT('Ctrl Pts',(15.5215291942096,43.0470858887221,5.59765407404954));
#47584=CARTESIAN_POINT('Ctrl Pts',(15.5351176224385,43.0765266266366,5.55983436456525));
#47585=CARTESIAN_POINT('Ctrl Pts',(15.5486308477265,43.1056851559705,5.521783643378));
#47586=CARTESIAN_POINT('Ctrl Pts',(15.5891693471925,43.1931582055674,5.40763479233376));
#47587=CARTESIAN_POINT('Ctrl Pts',(15.6290303150042,43.2780960580346,5.29140933264386));
#47588=CARTESIAN_POINT('Ctrl Pts',(15.6681066473624,43.3604744479936,5.1730534869981));
#47589=CARTESIAN_POINT('Ctrl Pts',(15.6976993071593,43.4228599258919,5.08342214076338));
#47590=CARTESIAN_POINT('Ctrl Pts',(15.7268423285855,43.4837755221708,4.99256790568704));
#47591=CARTESIAN_POINT('Ctrl Pts',(15.7554897945147,43.5432056956577,4.90046337961948));
#47592=CARTESIAN_POINT('Ctrl Pts',(15.7646705571918,43.5622515100411,4.87094629083393));
#47593=CARTESIAN_POINT('Ctrl Pts',(15.7738004920941,43.5811448088722,4.84130084737862));
#47594=CARTESIAN_POINT('Ctrl Pts',(15.7828779731803,43.5998843939893,4.81152567589992));
#47595=CARTESIAN_POINT('Ctrl Pts',(15.820280642411,43.6770986009926,4.68884066234464));
#47596=CARTESIAN_POINT('Ctrl Pts',(15.8567922974239,43.7517065136738,4.56395518348118));
#47597=CARTESIAN_POINT('Ctrl Pts',(15.8922960486642,43.8236398234513,4.43678015380184));
#47598=CARTESIAN_POINT('Ctrl Pts',(15.9220503656959,43.883924340706,4.33019969344502));
#47599=CARTESIAN_POINT('Ctrl Pts',(15.951097141453,43.9423283107648,4.22200998600328));
#47600=CARTESIAN_POINT('Ctrl Pts',(15.9793684755964,43.9988013639996,4.11215066858206));
#47601=CARTESIAN_POINT('Ctrl Pts',(15.9848313526463,44.0097136663654,4.09092252487934));
#47602=CARTESIAN_POINT('Ctrl Pts',(15.9902652197226,44.0205536468183,4.0696318793639));
#47603=CARTESIAN_POINT('Ctrl Pts',(15.9956695421084,44.0313207899642,4.04827818753736));
#47604=CARTESIAN_POINT('Ctrl Pts',(16.0040126986106,44.0479430330382,4.01531250190834));
#47605=CARTESIAN_POINT('Ctrl Pts',(16.0122853930047,44.0643920223782,3.98219675102727));
#47606=CARTESIAN_POINT('Ctrl Pts',(16.0204856406259,44.0806659925568,3.94892897658108));
#47607=CARTESIAN_POINT('Ctrl Pts',(16.0239840231979,44.0876087796871,3.93473630732213));
#47608=CARTESIAN_POINT('Ctrl Pts',(16.0274694356842,44.094520134833,3.92051509179209));
#47609=CARTESIAN_POINT('Ctrl Pts',(16.0309415561632,44.1013995895602,3.90626584129641));
#47610=CARTESIAN_POINT('Ctrl Pts',(16.0356081246678,44.1106456531553,3.88711469029829));
#47611=CARTESIAN_POINT('Ctrl Pts',(16.0402460460161,44.1198248975802,3.8679318106028));
#47612=CARTESIAN_POINT('Ctrl Pts',(16.0448535023226,44.1289342001359,3.84872390390704));
#47613=CARTESIAN_POINT('Ctrl Pts',(16.0485719715433,44.1362859054851,3.83322207272546));
#47614=CARTESIAN_POINT('Ctrl Pts',(16.0522710666275,44.1435929733322,3.81770199088401));
#47615=CARTESIAN_POINT('Ctrl Pts',(16.0559499973327,44.1508540876384,3.8021664460082));
#47616=CARTESIAN_POINT('Ctrl Pts',(16.0641803427192,44.167098339955,3.76741099385671));
#47617=CARTESIAN_POINT('Ctrl Pts',(16.0723121239858,44.1831172675052,3.73256848436886));
#47618=CARTESIAN_POINT('Ctrl Pts',(16.0803438330845,44.198910582354,3.69764008656643));
#47619=CARTESIAN_POINT('Ctrl Pts',(16.0842385396404,44.2065690179529,3.6807027375868));
#47620=CARTESIAN_POINT('Ctrl Pts',(16.0881097169479,44.2141744366289,3.66374520113459));
#47621=CARTESIAN_POINT('Ctrl Pts',(16.0919571938468,44.2217267787567,3.64676760402783));
#47622=CARTESIAN_POINT('Ctrl Pts',(16.119779354582,44.2763398361267,3.52399794276193));
#47623=CARTESIAN_POINT('Ctrl Pts',(16.146363769354,44.3281808208329,3.40017266404339));
#47624=CARTESIAN_POINT('Ctrl Pts',(16.1716578797485,44.3772491775588,3.27528341069522));
#47625=CARTESIAN_POINT('Ctrl Pts',(16.1742349382788,44.3822484451867,3.26255922665919));
#47626=CARTESIAN_POINT('Ctrl Pts',(16.1767986099626,44.3872189871422,3.24982401275424));
#47627=CARTESIAN_POINT('Ctrl Pts',(16.1793488358425,44.392160772613,3.23707775248512));
#47628=CARTESIAN_POINT('Ctrl Pts',(16.2069298067276,44.4456067211725,3.09922555823363));
#47629=CARTESIAN_POINT('Ctrl Pts',(16.2329384035846,44.4956855666432,2.96008015930213));
#47630=CARTESIAN_POINT('Ctrl Pts',(16.2572990629811,44.5423720081378,2.81962161298135));
#47631=CARTESIAN_POINT('Ctrl Pts',(16.2807607446571,44.58733558696,2.6843463871008));
#47632=CARTESIAN_POINT('Ctrl Pts',(16.3026939376851,44.6291520070692,2.54785305659329));
#47633=CARTESIAN_POINT('Ctrl Pts',(16.3230308540642,44.6677770232203,2.41011695510189));
#47634=CARTESIAN_POINT('Ctrl Pts',(16.3238101006238,44.6692570121423,2.40483934166183));
#47635=CARTESIAN_POINT('Ctrl Pts',(16.3245870042843,44.6707323159118,2.39955990406438));
#47636=CARTESIAN_POINT('Ctrl Pts',(16.3253615607141,44.6722029293553,2.39427864025978));
#47637=CARTESIAN_POINT('Ctrl Pts',(16.3463506296786,44.7120538760335,2.25116600709553));
#47638=CARTESIAN_POINT('Ctrl Pts',(16.3656162765854,44.7484612211025,2.10671223998137));
#47639=CARTESIAN_POINT('Ctrl Pts',(16.3830708867426,44.7813476320185,1.96087946147297));
#47640=CARTESIAN_POINT('Ctrl Pts',(16.4005254968998,44.8142340429344,1.81504668296456));
#47641=CARTESIAN_POINT('Ctrl Pts',(16.416169147287,44.8435995213574,1.66783495942057));
#47642=CARTESIAN_POINT('Ctrl Pts',(16.4299130047968,44.8693369120098,1.51919671520907));
#47643=CARTESIAN_POINT('Ctrl Pts',(16.4299744557924,44.8694519880194,1.51853212973313));
#47644=CARTESIAN_POINT('Ctrl Pts',(16.4300358688024,44.8695669915828,1.51786751575435));
#47645=CARTESIAN_POINT('Ctrl Pts',(16.4300972438189,44.8696819226926,1.51720287326893));
#47646=CARTESIAN_POINT('Ctrl Pts',(16.4334675848922,44.8759932373363,1.48070476707978));
#47647=CARTESIAN_POINT('Ctrl Pts',(16.4367232683546,44.8820856492454,1.4441205857469));
#47648=CARTESIAN_POINT('Ctrl Pts',(16.4398627890822,44.8879572706997,1.40744951143586));
#47649=CARTESIAN_POINT('Ctrl Pts',(16.4414611352971,44.8909465435032,1.38878007813454));
#47650=CARTESIAN_POINT('Ctrl Pts',(16.4430293733771,44.893878591633,1.37008812314347));
#47651=CARTESIAN_POINT('Ctrl Pts',(16.4445673042119,44.8967531505756,1.35137353294673));
#47652=CARTESIAN_POINT('Ctrl Pts',(16.4461052350467,44.8996277095182,1.33265894274999));
#47653=CARTESIAN_POINT('Ctrl Pts',(16.4476131566932,44.902445337259,1.31391780126205));
#47654=CARTESIAN_POINT('Ctrl Pts',(16.4490892691905,44.9052027752656,1.29517070927396));
#47655=CARTESIAN_POINT('Ctrl Pts',(16.4549937191796,44.916232527292,1.22018234132153));
#47656=CARTESIAN_POINT('Ctrl Pts',(16.4603932334168,44.9263069163642,1.14505238033023));
#47657=CARTESIAN_POINT('Ctrl Pts',(16.4652837831854,44.9354238512759,1.0697803390153));
#47658=CARTESIAN_POINT('Ctrl Pts',(16.4654957634851,44.9358190237382,1.06651768131284));
#47659=CARTESIAN_POINT('Ctrl Pts',(16.4657067875804,44.9362123981677,1.06325475685442));
#47660=CARTESIAN_POINT('Ctrl Pts',(16.4659168551513,44.9366039744898,1.05999156564776));
#47661=CARTESIAN_POINT('Ctrl Pts',(16.4705532092148,44.9452463673385,0.987970407184138));
#47662=CARTESIAN_POINT('Ctrl Pts',(16.4747234822227,44.9530123827719,0.915819173905195));
#47663=CARTESIAN_POINT('Ctrl Pts',(16.4784236180288,44.9598986924698,0.843537246033712));
#47664=CARTESIAN_POINT('Ctrl Pts',(16.4786783669902,44.9603728048634,0.838560740570758));
#47665=CARTESIAN_POINT('Ctrl Pts',(16.4789308802764,44.9608427339334,0.83358375782864));
#47666=CARTESIAN_POINT('Ctrl Pts',(16.4791811594326,44.9613084838401,0.828606248227442));
#47667=CARTESIAN_POINT('Ctrl Pts',(16.4808308405885,44.9643784112603,0.795797667937533));
#47668=CARTESIAN_POINT('Ctrl Pts',(16.4823838000093,44.9672673955566,0.762958679875174));
#47669=CARTESIAN_POINT('Ctrl Pts',(16.4838394108821,44.9699745720358,0.730094620377697));
#47670=CARTESIAN_POINT('Ctrl Pts',(16.4841034886147,44.9704657094954,0.724132404460733));
#47671=CARTESIAN_POINT('Ctrl Pts',(16.4843643638248,44.9709508668914,0.718169308811079));
#47672=CARTESIAN_POINT('Ctrl Pts',(16.484622032976,44.9714300393822,0.712205328484882));
#47673=CARTESIAN_POINT('Ctrl Pts',(16.4860001270905,44.9739928016937,0.680308121744984));
#47674=CARTESIAN_POINT('Ctrl Pts',(16.4872841965825,44.9763800615371,0.648441210361427));
#47675=CARTESIAN_POINT('Ctrl Pts',(16.4884754167523,44.9785942330604,0.616586113928043));
#47676=CARTESIAN_POINT('Ctrl Pts',(16.4887361289235,44.979078829846,0.6096142613972));
#47677=CARTESIAN_POINT('Ctrl Pts',(16.4889923805622,44.9795551113289,0.602643277310825));
#47678=CARTESIAN_POINT('Ctrl Pts',(16.4892441756933,44.9800230876665,0.595673160690036));
#47679=CARTESIAN_POINT('Ctrl Pts',(16.4944547318202,44.9897072184245,0.451436122767426));
#47680=CARTESIAN_POINT('Ctrl Pts',(16.4977573423716,44.9958371005211,0.307570384139903));
#47681=CARTESIAN_POINT('Ctrl Pts',(16.4991842745932,44.9984857834022,0.164068590449055));
#47682=CARTESIAN_POINT('Ctrl Pts',(16.4992938671831,44.9986892100349,0.153047230779077));
#47683=CARTESIAN_POINT('Ctrl Pts',(16.4993923956434,44.9988720974294,0.142028018465499));
#47684=CARTESIAN_POINT('Ctrl Pts',(16.4994798745568,44.9990344787445,0.13101095028804));
#47685=CARTESIAN_POINT('Ctrl Pts',(16.5005864417034,45.0010885260745,-0.00834978501705821));
#47686=CARTESIAN_POINT('Ctrl Pts',(16.4999249385232,44.99986126589,-0.147367414719779));
#47687=CARTESIAN_POINT('Ctrl Pts',(16.4975203492931,44.9953967706039,-0.286046671625515));
#47688=CARTESIAN_POINT('Ctrl Pts',(16.4972585106042,44.9949106262023,-0.301147627060495));
#47689=CARTESIAN_POINT('Ctrl Pts',(16.4969760035298,44.9943860851946,-0.316244569169732));
#47690=CARTESIAN_POINT('Ctrl Pts',(16.496672860267,44.9938232046973,-0.331337503657238));
#47691=CARTESIAN_POINT('Ctrl Pts',(16.4939720147342,44.9888082382989,-0.465807537110266));
#47692=CARTESIAN_POINT('Ctrl Pts',(16.4896330752602,44.9807498770209,-0.599959432563676));
#47693=CARTESIAN_POINT('Ctrl Pts',(16.4836750864447,44.9696687937092,-0.733795728849868));
#47694=CARTESIAN_POINT('Ctrl Pts',(16.4828199556229,44.9680783617411,-0.753004818622123));
#47695=CARTESIAN_POINT('Ctrl Pts',(16.4819314724365,44.9664256375575,-0.772207405753413));
#47696=CARTESIAN_POINT('Ctrl Pts',(16.4810096931329,44.964710682917,-0.791403496870234));
#47697=CARTESIAN_POINT('Ctrl Pts',(16.4747882752629,44.9531358412971,-0.920964774557578));
#47698=CARTESIAN_POINT('Ctrl Pts',(16.4670500736832,44.9387261544842,-1.05023011813212));
#47699=CARTESIAN_POINT('Ctrl Pts',(16.4578093131587,44.9214832065221,-1.1792002767713));
#47700=CARTESIAN_POINT('Ctrl Pts',(16.4561366865308,44.9183621415591,-1.20254455898384));
#47701=CARTESIAN_POINT('Ctrl Pts',(16.4544148316611,44.9151482076373,-1.22587916896365));
#47702=CARTESIAN_POINT('Ctrl Pts',(16.4526438329193,44.9118414151564,-1.2492041094649));
#47703=CARTESIAN_POINT('Ctrl Pts',(16.443180940093,44.8941723891387,-1.37383514783657));
#47704=CARTESIAN_POINT('Ctrl Pts',(16.4323149566667,44.8738522519087,-1.49819010731742));
#47705=CARTESIAN_POINT('Ctrl Pts',(16.4200562281029,44.8508667452653,-1.6222682560188));
#47706=CARTESIAN_POINT('Ctrl Pts',(16.4173388192111,44.8457715170114,-1.64977282656279));
#47707=CARTESIAN_POINT('Ctrl Pts',(16.4145529103487,44.8405451493894,-1.67726442598618));
#47708=CARTESIAN_POINT('Ctrl Pts',(16.4116986443443,44.8351875376271,-1.70474268064929));
#47709=CARTESIAN_POINT('Ctrl Pts',(16.4038308879674,44.820419333107,-1.78048622137831));
#47710=CARTESIAN_POINT('Ctrl Pts',(16.3954436387708,44.8046533890257,-1.85612832314843));
#47711=CARTESIAN_POINT('Ctrl Pts',(16.3865397744708,44.7878852560871,-1.9316610001985));
#47712=CARTESIAN_POINT('Ctrl Pts',(16.3820866822432,44.7794990049107,-1.96943717981755));
#47713=CARTESIAN_POINT('Ctrl Pts',(16.377504371403,44.7708620589204,-2.00718598805293));
#47714=CARTESIAN_POINT('Ctrl Pts',(16.3727932172076,44.7619737563975,-2.04490642000078));
#47715=CARTESIAN_POINT('Ctrl Pts',(16.3720401557642,44.7605529924721,-2.05093589850025));
#47716=CARTESIAN_POINT('Ctrl Pts',(16.3712837309502,44.7591256713598,-2.05696519021422));
#47717=CARTESIAN_POINT('Ctrl Pts',(16.3705239817059,44.7576918606981,-2.06299400873138));
#47718=CARTESIAN_POINT('Ctrl Pts',(16.3682159895784,44.7533361818419,-2.08130855893217));
#47719=CARTESIAN_POINT('Ctrl Pts',(16.3658775520689,44.7489210288428,-2.09961695772403));
#47720=CARTESIAN_POINT('Ctrl Pts',(16.3635087125001,44.7444463373124,-2.11791921235832));
#47721=CARTESIAN_POINT('Ctrl Pts',(16.3617786253703,44.7411782366236,-2.13128630382624));
#47722=CARTESIAN_POINT('Ctrl Pts',(16.3600322470299,44.7378782361758,-2.14465061537265));
#47723=CARTESIAN_POINT('Ctrl Pts',(16.3582707990857,44.7345485708757,-2.15800288780629));
#47724=CARTESIAN_POINT('Ctrl Pts',(16.3576204681566,44.7333192502277,-2.16293257974857));
#47725=CARTESIAN_POINT('Ctrl Pts',(16.3569681873215,44.7320860844049,-2.16785987516607));
#47726=CARTESIAN_POINT('Ctrl Pts',(16.3563140031161,44.7308491577237,-2.17278446775161));
#47727=CARTESIAN_POINT('Ctrl Pts',(16.3514618653041,44.7216747712565,-2.20931057415699));
#47728=CARTESIAN_POINT('Ctrl Pts',(16.3465010296124,44.7122858451787,-2.24571805287309));
#47729=CARTESIAN_POINT('Ctrl Pts',(16.341433306043,44.7026846488829,-2.28200831008602));
#47730=CARTESIAN_POINT('Ctrl Pts',(16.3312978589041,44.6834822562912,-2.35458882451186));
#47731=CARTESIAN_POINT('Ctrl Pts',(16.3207348679184,44.663430782441,-2.42670045515599));
#47732=CARTESIAN_POINT('Ctrl Pts',(16.3097587820106,44.6425471384181,-2.49835388334598));
#47733=CARTESIAN_POINT('Ctrl Pts',(16.3043316767858,44.6322212595444,-2.53378278739943));
#47734=CARTESIAN_POINT('Ctrl Pts',(16.298803590232,44.6216917192259,-2.56909957998654));
#47735=CARTESIAN_POINT('Ctrl Pts',(16.2931762640366,44.610960536853,-2.60430551760671));
#47736=CARTESIAN_POINT('Ctrl Pts',(16.2760415418866,44.578285013538,-2.71150455640482));
#47737=CARTESIAN_POINT('Ctrl Pts',(16.2579866657359,44.5437398675915,-2.81767574143081));
#47738=CARTESIAN_POINT('Ctrl Pts',(16.2390566392221,44.507368577513,-2.92284842704556));
#47739=CARTESIAN_POINT('Ctrl Pts',(16.2320092324275,44.4938280113313,-2.96200287295586));
#47740=CARTESIAN_POINT('Ctrl Pts',(16.2248405515908,44.4800339777492,-3.0010187855979));
#47741=CARTESIAN_POINT('Ctrl Pts',(16.2175529061345,44.4659887626675,-3.03989765234625));
#47742=CARTESIAN_POINT('Ctrl Pts',(16.1988363578857,44.4299170372631,-3.13974858358623));
#47743=CARTESIAN_POINT('Ctrl Pts',(16.1793357237602,44.3921918998984,-3.23869700091219));
#47744=CARTESIAN_POINT('Ctrl Pts',(16.1590864494294,44.3528367566819,-3.33676146628663));
#47745=CARTESIAN_POINT('Ctrl Pts',(16.1309527334746,44.298157936961,-3.4730092038118));
#47746=CARTESIAN_POINT('Ctrl Pts',(16.1013735545187,44.2403372266431,-3.60755228756136));
#47747=CARTESIAN_POINT('Ctrl Pts',(16.0704438737352,44.1794272699162,-3.74043491721408));
#47748=CARTESIAN_POINT('Ctrl Pts',(16.0595449233439,44.1579639188604,-3.78725988118906));
#47749=CARTESIAN_POINT('Ctrl Pts',(16.0484783200874,44.1361163383025,-3.83387845461765));
#47750=CARTESIAN_POINT('Ctrl Pts',(16.0372481693921,44.113887257799,-3.88029266336609));
#47751=CARTESIAN_POINT('Ctrl Pts',(16.0166087396519,44.073033349629,-3.96559541899249));
#47752=CARTESIAN_POINT('Ctrl Pts',(15.9954165095932,44.0308907581977,-4.05020776137457));
#47753=CARTESIAN_POINT('Ctrl Pts',(15.9736952183765,43.9874629851133,-4.13413673701598));
#47754=CARTESIAN_POINT('Ctrl Pts',(15.9401551232136,43.9204056620733,-4.26373243194281));
#47755=CARTESIAN_POINT('Ctrl Pts',(15.905353150331,43.8502891232181,-4.39170062734481));
#47756=CARTESIAN_POINT('Ctrl Pts',(15.869376700399,43.777119676058,-4.51806349542216));
#47757=CARTESIAN_POINT('Ctrl Pts',(15.8538182611451,43.745476687352,-4.57271060514651));
#47758=CARTESIAN_POINT('Ctrl Pts',(15.8380402437097,43.7132618093626,-4.62705717641083));
#47759=CARTESIAN_POINT('Ctrl Pts',(15.822049652599,43.6804760856509,-4.68110508221071));
#47760=CARTESIAN_POINT('Ctrl Pts',(15.8027755650205,43.6409581650331,-4.74625114608124));
#47761=CARTESIAN_POINT('Ctrl Pts',(15.783192557801,43.6006087489436,-4.81096243631331));
#47762=CARTESIAN_POINT('Ctrl Pts',(15.7633127763008,43.5594253043274,-4.87524053934891));
#47763=CARTESIAN_POINT('Ctrl Pts',(15.7615479512871,43.555769249395,-4.88094681957486));
#47764=CARTESIAN_POINT('Ctrl Pts',(15.7597807873781,43.552106620627,-4.88664968554212));
#47765=CARTESIAN_POINT('Ctrl Pts',(15.7580112930854,43.548437415296,-4.89234913800578));
#47766=CARTESIAN_POINT('Ctrl Pts',(15.7498073372243,43.5314257760349,-4.91877366881019));
#47767=CARTESIAN_POINT('Ctrl Pts',(15.7415544292727,43.514275118157,-4.94512121020454));
#47768=CARTESIAN_POINT('Ctrl Pts',(15.7332502456038,43.4969785891754,-4.97140188570682));
#47769=CARTESIAN_POINT('Ctrl Pts',(15.7318779865615,43.494120352985,-4.9757447442022));
#47770=CARTESIAN_POINT('Ctrl Pts',(15.7305044376723,43.4912583615479,-4.98008541804862));
#47771=CARTESIAN_POINT('Ctrl Pts',(15.7291296393024,43.4883926909596,-4.98442379964834));
#47772=CARTESIAN_POINT('Ctrl Pts',(15.7203852640188,43.4701656551905,-5.01201798193912));
#47773=CARTESIAN_POINT('Ctrl Pts',(15.711597089659,43.4518037974615,-5.03949821938434));
#47774=CARTESIAN_POINT('Ctrl Pts',(15.7027746567282,43.4333249627762,-5.06684004878928));
#47775=CARTESIAN_POINT('Ctrl Pts',(15.701816203265,43.4313174549562,-5.06981041663333));
#47776=CARTESIAN_POINT('Ctrl Pts',(15.7008572951018,43.4293084622317,-5.07277931161621));
#47777=CARTESIAN_POINT('Ctrl Pts',(15.6998979279679,43.4272979728774,-5.07574675362532));
#47778=CARTESIAN_POINT('Ctrl Pts',(15.6803175074106,43.3862644355702,-5.13631143263322));
#47779=CARTESIAN_POINT('Ctrl Pts',(15.6605550261926,43.3446258030676,-5.19624268367425));
#47780=CARTESIAN_POINT('Ctrl Pts',(15.6406249503671,43.3023913589472,-5.25555493854259));
#47781=CARTESIAN_POINT('Ctrl Pts',(15.619858525843,43.2583845822638,-5.31735618179178));
#47782=CARTESIAN_POINT('Ctrl Pts',(15.598910322171,43.213730246343,-5.37848484512116));
#47783=CARTESIAN_POINT('Ctrl Pts',(15.5777971164023,43.1684369147297,-5.43895550636533));
#47784=CARTESIAN_POINT('Ctrl Pts',(15.5583845406235,43.1267918778816,-5.49455536678717));
#47785=CARTESIAN_POINT('Ctrl Pts',(15.5388325010489,43.0846079034054,-5.54960000848349));
#47786=CARTESIAN_POINT('Ctrl Pts',(15.5191535351483,43.0418879348754,-5.60409744798316));
#47787=CARTESIAN_POINT('Ctrl Pts',(15.4780716363702,42.9527055341427,-5.71786655071465));
#47788=CARTESIAN_POINT('Ctrl Pts',(15.4364351847114,42.8611928677454,-5.82925514163746));
#47789=CARTESIAN_POINT('Ctrl Pts',(15.3943559547313,42.7673817983009,-5.93833747396013));
#47790=CARTESIAN_POINT('Ctrl Pts',(15.3682783871389,42.7092446958513,-6.00593856589142));
#47791=CARTESIAN_POINT('Ctrl Pts',(15.3420312154126,42.6502231410027,-6.07265263288714));
#47792=CARTESIAN_POINT('Ctrl Pts',(15.3156411568502,42.5903237758893,-6.13849622909734));
#47793=CARTESIAN_POINT('Ctrl Pts',(15.2994477444082,42.553568452971,-6.17889903864669));
#47794=CARTESIAN_POINT('Ctrl Pts',(15.2832003544436,42.5164826160552,-6.21897402344193));
#47795=CARTESIAN_POINT('Ctrl Pts',(15.2669052552736,42.4790655001611,-6.25872313049107));
#47796=CARTESIAN_POINT('Ctrl Pts',(15.2240543808514,42.3806705092686,-6.363250508741));
#47797=CARTESIAN_POINT('Ctrl Pts',(15.1808723838033,42.2799892221281,-6.4655276503284));
#47798=CARTESIAN_POINT('Ctrl Pts',(15.1374702843923,42.1770158208016,-6.56559359303154));
#47799=CARTESIAN_POINT('Ctrl Pts',(15.1058399630617,42.1019714838535,-6.63851904974661));
#47800=CARTESIAN_POINT('Ctrl Pts',(15.0740932923155,42.0257078582054,-6.71026872409978));
#47801=CARTESIAN_POINT('Ctrl Pts',(15.0422738349374,41.948220165619,-6.78085524655767));
#47802=CARTESIAN_POINT('Ctrl Pts',(15.0304316665642,41.9193817636449,-6.80712525719604));
#47803=CARTESIAN_POINT('Ctrl Pts',(15.0185794677439,41.8903734206547,-6.83323385195918));
#47804=CARTESIAN_POINT('Ctrl Pts',(15.0067196161185,41.8611942483808,-6.85918119667358));
#47805=CARTESIAN_POINT('Ctrl Pts',(14.9722967908615,41.7765026704379,-6.93449250251397));
#47806=CARTESIAN_POINT('Ctrl Pts',(14.9378087380572,41.6903744753995,-7.00844713018512));
#47807=CARTESIAN_POINT('Ctrl Pts',(14.9033129588711,41.6027897699871,-7.0810495585008));
#47808=CARTESIAN_POINT('Ctrl Pts',(14.8939892424914,41.5791168751655,-7.10067295782853));
#47809=CARTESIAN_POINT('Ctrl Pts',(14.8846649774315,41.5553375106934,-7.12019752487661));
#47810=CARTESIAN_POINT('Ctrl Pts',(14.8753413457217,41.5314511178781,-7.13962322834019));
#47811=CARTESIAN_POINT('Ctrl Pts',(14.8643865713129,41.5033858689625,-7.16244740306092));
#47812=CARTESIAN_POINT('Ctrl Pts',(14.8534326525802,41.4751729344196,-7.18513513563339));
#47813=CARTESIAN_POINT('Ctrl Pts',(14.8424815052911,41.4468114212109,-7.20768636692352));
#47814=CARTESIAN_POINT('Ctrl Pts',(14.839526559386,41.4391586397165,-7.21377136119811));
#47815=CARTESIAN_POINT('Ctrl Pts',(14.8365718795728,41.4314952045087,-7.21984628480176));
#47816=CARTESIAN_POINT('Ctrl Pts',(14.8336174020316,41.4238208387543,-7.2259113453007));
#47817=CARTESIAN_POINT('Ctrl Pts',(14.8310971738157,41.4172744518406,-7.23108496276333));
#47818=CARTESIAN_POINT('Ctrl Pts',(14.8285769848935,41.4107198134149,-7.23625161312468));
#47819=CARTESIAN_POINT('Ctrl Pts',(14.8260571075248,41.4041575738866,-7.24141079712401));
#47820=CARTESIAN_POINT('Ctrl Pts',(14.8205831639148,41.3899023844958,-7.25261812119303));
#47821=CARTESIAN_POINT('Ctrl Pts',(14.8151098042831,41.3756089978122,-7.26379201309443));
#47822=CARTESIAN_POINT('Ctrl Pts',(14.8096438019145,41.3612944710306,-7.27491924106125));
#47823=CARTESIAN_POINT('Ctrl Pts',(14.806022034559,41.3518096808106,-7.28229213047671));
#47824=CARTESIAN_POINT('Ctrl Pts',(14.8024024578911,41.342312907149,-7.28964665424675));
#47825=CARTESIAN_POINT('Ctrl Pts',(14.7987860936221,41.3328066241553,-7.29698089316516));
#47826=CARTESIAN_POINT('Ctrl Pts',(14.787192400397,41.3023304551242,-7.32049371149171));
#47827=CARTESIAN_POINT('Ctrl Pts',(14.7756248165093,41.2717387024353,-7.34381230341903));
#47828=CARTESIAN_POINT('Ctrl Pts',(14.7640863609218,41.2410335710712,-7.36693653612173));
#47829=CARTESIAN_POINT('Ctrl Pts',(14.7574965735345,41.2234974037867,-7.38014313694009));
#47830=CARTESIAN_POINT('Ctrl Pts',(14.7509162585555,41.2059243753268,-7.39328652526075));
#47831=CARTESIAN_POINT('Ctrl Pts',(14.7443459874502,41.1883148488364,-7.40636660041844));
#47832=CARTESIAN_POINT('Ctrl Pts',(14.7010199283645,41.0721930978521,-7.49261998327614));
#47833=CARTESIAN_POINT('Ctrl Pts',(14.6581251019111,40.954469129494,-7.57613167115738));
#47834=CARTESIAN_POINT('Ctrl Pts',(14.6157752637112,40.8351450172988,-7.65696941752765));
#47835=CARTESIAN_POINT('Ctrl Pts',(14.5743516489294,40.7184306148866,-7.73603918043128));
#47836=CARTESIAN_POINT('Ctrl Pts',(14.5334494998714,40.6001850804501,-7.81255034269787));
#47837=CARTESIAN_POINT('Ctrl Pts',(14.4931826853823,40.4803989550325,-7.88654903288741));
#47838=CARTESIAN_POINT('Ctrl Pts',(14.4922823277783,40.4777205621614,-7.88820362822203));
#47839=CARTESIAN_POINT('Ctrl Pts',(14.4913822873103,40.4750413992675,-7.88985696731292));
#47840=CARTESIAN_POINT('Ctrl Pts',(14.4904825653626,40.47236146595,-7.89150905022655));
#47841=CARTESIAN_POINT('Ctrl Pts',(14.4493444574659,40.3498265136191,-7.96704745998726));
#47842=CARTESIAN_POINT('Ctrl Pts',(14.408872387569,40.2256806345653,-8.03995982187575));
#47843=CARTESIAN_POINT('Ctrl Pts',(14.3691870118136,40.0999011485163,-8.1102716271545));
#47844=CARTESIAN_POINT('Ctrl Pts',(14.3295016360582,39.9741216624673,-8.18058343243325));
#47845=CARTESIAN_POINT('Ctrl Pts',(14.2906028707937,39.846708554917,-8.24829461494413));
#47846=CARTESIAN_POINT('Ctrl Pts',(14.2526202581606,39.7176264034462,-8.31341191098604));
#47847=CARTESIAN_POINT('Ctrl Pts',(14.248137967391,39.7023935456742,-8.32109633906382));
#47848=CARTESIAN_POINT('Ctrl Pts',(14.2436684144369,39.6871374675747,-8.32874467778675));
#47849=CARTESIAN_POINT('Ctrl Pts',(14.2392118009553,39.6718581285822,-8.33635695538212));
#47850=CARTESIAN_POINT('Ctrl Pts',(14.2059033893122,39.557661437553,-8.39325057578117));
#47851=CARTESIAN_POINT('Ctrl Pts',(14.1733193051381,39.4421622806704,-8.44812547388581));
#47852=CARTESIAN_POINT('Ctrl Pts',(14.1415516469276,39.325327603003,-8.5009715729199));
#47853=CARTESIAN_POINT('Ctrl Pts',(14.1346399853956,39.2999079846639,-8.51246925233306));
#47854=CARTESIAN_POINT('Ctrl Pts',(14.1277670070846,39.2744250860744,-8.52387082842112));
#47855=CARTESIAN_POINT('Ctrl Pts',(14.1209336546232,39.2488785816658,-8.53517619746252));
#47856=CARTESIAN_POINT('Ctrl Pts',(14.0921569708267,39.1412968809374,-8.5827854832335));
#47857=CARTESIAN_POINT('Ctrl Pts',(14.0640830121568,39.032587235213,-8.62868866018023));
#47858=CARTESIAN_POINT('Ctrl Pts',(14.0367872922916,38.9227161423072,-8.67286593317823));
#47859=CARTESIAN_POINT('Ctrl Pts',(14.0277166460954,38.8862048571731,-8.68754649171477));
#47860=CARTESIAN_POINT('Ctrl Pts',(14.0187320348612,38.8495651717845,-8.70203629691729));
#47861=CARTESIAN_POINT('Ctrl Pts',(14.0098362084193,38.8127959120846,-8.71633463178559));
#47862=CARTESIAN_POINT('Ctrl Pts',(13.9856056306185,38.7126432827975,-8.75528063840029));
#47863=CARTESIAN_POINT('Ctrl Pts',(13.9620337294482,38.6115293995748,-8.79280618368359));
#47864=CARTESIAN_POINT('Ctrl Pts',(13.9391806731364,38.5094228580167,-8.82888688050722));
#47865=CARTESIAN_POINT('Ctrl Pts',(13.9313698855874,38.4745245716522,-8.84121865152567));
#47866=CARTESIAN_POINT('Ctrl Pts',(13.9236430764078,38.4395103239397,-8.85338162525871));
#47867=CARTESIAN_POINT('Ctrl Pts',(13.9160027405551,38.4043787548999,-8.8653746637582));
#47868=CARTESIAN_POINT('Ctrl Pts',(13.9130052106185,38.390595600344,-8.87007988779891));
#47869=CARTESIAN_POINT('Ctrl Pts',(13.910020831446,38.3767936600104,-8.87475920513983));
#47870=CARTESIAN_POINT('Ctrl Pts',(13.9070497732776,38.3629729696956,-8.87941251455177));
#47871=CARTESIAN_POINT('Ctrl Pts',(13.9024479688811,38.3415664169289,-8.88661991962326));
#47872=CARTESIAN_POINT('Ctrl Pts',(13.8978835001752,38.3201396295624,-8.89375650346339));
#47873=CARTESIAN_POINT('Ctrl Pts',(13.8933570138086,38.2986941565034,-8.90082193318904));
#47874=CARTESIAN_POINT('Ctrl Pts',(13.8817723344466,38.243808554508,-8.91890455429896));
#47875=CARTESIAN_POINT('Ctrl Pts',(13.8704362542691,38.1887995487795,-8.93652141653211));
#47876=CARTESIAN_POINT('Ctrl Pts',(13.8593562640666,38.1336760029268,-8.95367209281636));
#47877=CARTESIAN_POINT('Ctrl Pts',(13.85618744769,38.1179109714023,-8.95857709208856));
#47878=CARTESIAN_POINT('Ctrl Pts',(13.8530394321209,38.1021358845332,-8.96344418765362));
#47879=CARTESIAN_POINT('Ctrl Pts',(13.8499123051586,38.0863505151219,-8.96827348830095));
#47880=CARTESIAN_POINT('Ctrl Pts',(13.8378223340655,38.0253217618366,-8.98694433407386));
#47881=CARTESIAN_POINT('Ctrl Pts',(13.8260460707125,37.9641458211664,-9.00504796639664));
#47882=CARTESIAN_POINT('Ctrl Pts',(13.8145911106071,37.9028221956007,-9.02258679352785));
#47883=CARTESIAN_POINT('Ctrl Pts',(13.7994004865694,37.8214998573276,-9.04584534061672));
#47884=CARTESIAN_POINT('Ctrl Pts',(13.7847749381894,37.7399183242153,-9.06811310342971));
#47885=CARTESIAN_POINT('Ctrl Pts',(13.7707320465202,37.6580753553695,-9.08939044769318));
#47886=CARTESIAN_POINT('Ctrl Pts',(13.7460996778528,37.5145161633648,-9.12671263179219));
#47887=CARTESIAN_POINT('Ctrl Pts',(13.7232576460597,37.3701536907579,-9.16099116468723));
#47888=CARTESIAN_POINT('Ctrl Pts',(13.702299523627,37.2249766791102,-9.19222897002465));
#47889=CARTESIAN_POINT('Ctrl Pts',(13.689764940887,37.1381495661241,-9.21091160044037));
#47890=CARTESIAN_POINT('Ctrl Pts',(13.677905036562,37.0510307339763,-9.22850534417129));
#47891=CARTESIAN_POINT('Ctrl Pts',(13.666739988455,36.9636177322509,-9.24501044282744));
#47892=CARTESIAN_POINT('Ctrl Pts',(13.6592368088238,36.9048741023298,-9.25610226427426));
#47893=CARTESIAN_POINT('Ctrl Pts',(13.6520474529696,36.845997636278,-9.26670251302155));
#47894=CARTESIAN_POINT('Ctrl Pts',(13.6451779510603,36.7869869886694,-9.27680829891729));
#47895=CARTESIAN_POINT('Ctrl Pts',(13.6280863402507,36.6401660057417,-9.30195192093463));
#47896=CARTESIAN_POINT('Ctrl Pts',(13.6129724662781,36.492515433864,-9.32403804535087));
#47897=CARTESIAN_POINT('Ctrl Pts',(13.5999250865708,36.3440166675744,-9.34302753896882));
#47898=CARTESIAN_POINT('Ctrl Pts',(13.5898455510966,36.229296423642,-9.35769755539006));
#47899=CARTESIAN_POINT('Ctrl Pts',(13.5810002995574,36.114069533427,-9.37051802455725));
#47900=CARTESIAN_POINT('Ctrl Pts',(13.5734319623329,35.9983267443972,-9.38146815610025));
#47901=CARTESIAN_POINT('Ctrl Pts',(13.5712035217423,35.9642471412434,-9.38469234086887));
#47902=CARTESIAN_POINT('Ctrl Pts',(13.5690857701538,35.9301227262426,-9.38775395342427));
#47903=CARTESIAN_POINT('Ctrl Pts',(13.5670797784949,35.8959531945743,-9.39065210232899));
#47904=CARTESIAN_POINT('Ctrl Pts',(13.5642827085755,35.8483086449258,-9.39469315857526));
#47905=CARTESIAN_POINT('Ctrl Pts',(13.5617027314333,35.8005764620705,-9.39841668469839));
#47906=CARTESIAN_POINT('Ctrl Pts',(13.5593426708374,35.7527558543533,-9.40182037346003));
#47907=CARTESIAN_POINT('Ctrl Pts',(13.5579822327385,35.7251900466087,-9.40378240268769));
#47908=CARTESIAN_POINT('Ctrl Pts',(13.5566948689149,35.697594853584,-9.4056381399649));
#47909=CARTESIAN_POINT('Ctrl Pts',(13.5554811164538,35.669970111593,-9.40738708330099));
#47910=CARTESIAN_POINT('Ctrl Pts',(13.5548859234267,35.6564236477657,-9.40824472018485));
#47911=CARTESIAN_POINT('Ctrl Pts',(13.5543085108019,35.6428719569098,-9.40907656239463));
#47912=CARTESIAN_POINT('Ctrl Pts',(13.5537488650355,35.6293134090097,-9.40988266151869));
#47913=CARTESIAN_POINT('Ctrl Pts',(13.5527479600881,35.6050644671116,-9.41132433882568));
#47914=CARTESIAN_POINT('Ctrl Pts',(13.5518034882189,35.5807810331349,-9.41268424408725));
#47915=CARTESIAN_POINT('Ctrl Pts',(13.5509164078193,35.5564825681396,-9.41396115050902));
#47916=CARTESIAN_POINT('Ctrl Pts',(13.550295559802,35.5394766081131,-9.4148548291661));
#47917=CARTESIAN_POINT('Ctrl Pts',(13.5497028741862,35.5224643640414,-9.41570777996314));
#47918=CARTESIAN_POINT('Ctrl Pts',(13.5491389538032,35.5054603497194,-9.41651918760508));
#47919=CARTESIAN_POINT('Ctrl Pts',(13.5490747427451,35.5035241796801,-9.41661157891552));
#47920=CARTESIAN_POINT('Ctrl Pts',(13.5490109040932,35.5015881247004,-9.41670343285821));
#47921=CARTESIAN_POINT('Ctrl Pts',(13.5489474379496,35.499652191645,-9.41679474932162));
#47922=CARTESIAN_POINT('Ctrl Pts',(13.5483265934797,35.4807143255304,-9.41768803380448));
#47923=CARTESIAN_POINT('Ctrl Pts',(13.5477412466006,35.4617829285047,-9.41853009944171));
#47924=CARTESIAN_POINT('Ctrl Pts',(13.5471913035612,35.442857980976,-9.4193211140302));
#47925=CARTESIAN_POINT('Ctrl Pts',(13.5430022229461,35.2987009953143,-9.42534650873831));
#47926=CARTESIAN_POINT('Ctrl Pts',(13.5408674811866,35.1549181959707,-9.42840961630309));
#47927=CARTESIAN_POINT('Ctrl Pts',(13.5407592808403,35.0115034033078,-9.42856500737733));
#47928=CARTESIAN_POINT('Ctrl Pts',(13.5407538447441,35.0042980972761,-9.42857281438402));
#47929=CARTESIAN_POINT('Ctrl Pts',(13.5407535274295,34.9970937191213,-9.42857329535632));
#47930=CARTESIAN_POINT('Ctrl Pts',(13.5407583244004,34.9898902683715,-9.42856645346899));
#47931=CARTESIAN_POINT('Ctrl Pts',(13.5408586005346,34.8393089525897,-9.42842343029414));
#47932=CARTESIAN_POINT('Ctrl Pts',(13.5431955597245,34.6891331210029,-9.42507782600044));
#47933=CARTESIAN_POINT('Ctrl Pts',(13.5477229961778,34.5393569862264,-9.41856595336358));
#47934=CARTESIAN_POINT('Ctrl Pts',(13.5522504326312,34.3895808514499,-9.41205408072671));
#47935=CARTESIAN_POINT('Ctrl Pts',(13.5589683476105,34.2402044010644,-9.40237594907378));
#47936=CARTESIAN_POINT('Ctrl Pts',(13.5678384517885,34.0912233027804,-9.38955637262442));
#47937=CARTESIAN_POINT('Ctrl Pts',(13.5689885488583,34.0719064242919,-9.387894187264));
#47938=CARTESIAN_POINT('Ctrl Pts',(13.5701748380717,34.0525961922414,-9.38617917383737));
#47939=CARTESIAN_POINT('Ctrl Pts',(13.5713972196396,34.0332925947168,-9.38441140971383));
#47940=CARTESIAN_POINT('Ctrl Pts',(13.5796024352172,33.9037175231669,-9.37254532296499));
#47941=CARTESIAN_POINT('Ctrl Pts',(13.5894337323259,33.7744414510532,-9.35830230953036));
#47942=CARTESIAN_POINT('Ctrl Pts',(13.6008538043109,33.6454626048097,-9.34167733991798));
#47943=CARTESIAN_POINT('Ctrl Pts',(13.6139751948495,33.4972689844025,-9.32257564605289));
#47944=CARTESIAN_POINT('Ctrl Pts',(13.6291932512565,33.3494676061594,-9.30033053952966));
#47945=CARTESIAN_POINT('Ctrl Pts',(13.6464570722265,33.2020569656426,-9.27492584007278));
#47946=CARTESIAN_POINT('Ctrl Pts',(13.6517062465988,33.1572358244975,-9.26720137991093));
#47947=CARTESIAN_POINT('Ctrl Pts',(13.6571445977731,33.1124507933225,-9.25918474429875));
#47948=CARTESIAN_POINT('Ctrl Pts',(13.6627705971131,33.0677018138577,-9.25087561318739));
#47949=CARTESIAN_POINT('Ctrl Pts',(13.6728200500002,32.9877688572938,-9.23603341065783));
#47950=CARTESIAN_POINT('Ctrl Pts',(13.6834677371398,32.907951109785,-9.22025577061754));
#47951=CARTESIAN_POINT('Ctrl Pts',(13.6947039744194,32.8282485786631,-9.20353644274965));
#47952=CARTESIAN_POINT('Ctrl Pts',(13.6978656042632,32.8058220407795,-9.19883199190547));
#47953=CARTESIAN_POINT('Ctrl Pts',(13.7010738298154,32.7834046255516,-9.19405297520816));
#47954=CARTESIAN_POINT('Ctrl Pts',(13.704328429154,32.7609963352982,-9.18919922232318));
#47955=CARTESIAN_POINT('Ctrl Pts',(13.7068555947766,32.7435965097287,-9.18543032908765));
#47956=CARTESIAN_POINT('Ctrl Pts',(13.7094107324537,32.7262021023487,-9.18161635742941));
#47957=CARTESIAN_POINT('Ctrl Pts',(13.7119938175221,32.7088126084929,-9.17775710880594));
#47958=CARTESIAN_POINT('Ctrl Pts',(13.7148526957193,32.689566457659,-9.17348581248596));
#47959=CARTESIAN_POINT('Ctrl Pts',(13.717746213636,32.670324099751,-9.16915843765454));
#47960=CARTESIAN_POINT('Ctrl Pts',(13.7206719802958,32.6510994569933,-9.16477824576685));
#47961=CARTESIAN_POINT('Ctrl Pts',(13.7237925263614,32.6305949567047,-9.16010644785847));
#47962=CARTESIAN_POINT('Ctrl Pts',(13.7269492160484,32.6101141402426,-9.15537537818358));
#47963=CARTESIAN_POINT('Ctrl Pts',(13.7301396445541,32.5896707038453,-9.15058825109336));
#47964=CARTESIAN_POINT('Ctrl Pts',(13.7326432238633,32.5736284185275,-9.14683171735109));
#47965=CARTESIAN_POINT('Ctrl Pts',(13.735168271931,32.557604298108,-9.14303964568289));
#47966=CARTESIAN_POINT('Ctrl Pts',(13.7377149247936,32.5415963237026,-9.13921163623647));
#47967=CARTESIAN_POINT('Ctrl Pts',(13.7492988688276,32.4687809501066,-9.12179919348068));
#47968=CARTESIAN_POINT('Ctrl Pts',(13.761323702081,32.3963376875117,-9.10365238666682));
#47969=CARTESIAN_POINT('Ctrl Pts',(13.7737713161574,32.3242591214252,-9.08478005398837));
#47970=CARTESIAN_POINT('Ctrl Pts',(13.7855758014131,32.2559046267088,-9.0668827950056));
#47971=CARTESIAN_POINT('Ctrl Pts',(13.7977609475819,32.187878518565,-9.04833238126448));
#47972=CARTESIAN_POINT('Ctrl Pts',(13.8103118541531,32.1201748608641,-9.02913542323162));
#47973=CARTESIAN_POINT('Ctrl Pts',(13.8242303510202,32.0450939778811,-9.00784669809264));
#47974=CARTESIAN_POINT('Ctrl Pts',(13.8385981219998,31.9704087713137,-8.98576461959821));
#47975=CARTESIAN_POINT('Ctrl Pts',(13.8533964756602,31.8961139063031,-8.96289268199796));
#47976=CARTESIAN_POINT('Ctrl Pts',(13.8815391405615,31.7548241697653,-8.91939613567287));
#47977=CARTESIAN_POINT('Ctrl Pts',(13.9112357191329,31.6149430430769,-8.87304823794877));
#47978=CARTESIAN_POINT('Ctrl Pts',(13.9423542403051,31.4764299357821,-8.82387705704306));
#47979=CARTESIAN_POINT('Ctrl Pts',(13.9621098348215,31.3884948836058,-8.79266073071149));
#47980=CARTESIAN_POINT('Ctrl Pts',(13.9824396027645,31.3011122143628,-8.76030478122907));
#47981=CARTESIAN_POINT('Ctrl Pts',(14.0033100035835,31.2142716336085,-8.7268155098858));
#47982=CARTESIAN_POINT('Ctrl Pts',(14.0153141390999,31.1643230912332,-8.70755331386777));
#47983=CARTESIAN_POINT('Ctrl Pts',(14.0274972073736,31.1145539360271,-8.68791611827075));
#47984=CARTESIAN_POINT('Ctrl Pts',(14.039853406829,31.0649633164737,-8.66790286279505));
#47985=CARTESIAN_POINT('Ctrl Pts',(14.0736921057848,30.9291544011065,-8.61309454332662));
#47986=CARTESIAN_POINT('Ctrl Pts',(14.10882687604,30.7946821312524,-8.55546981872774));
#47987=CARTESIAN_POINT('Ctrl Pts',(14.1451333866133,30.6615234073939,-8.49501412466315));
#47988=CARTESIAN_POINT('Ctrl Pts',(14.1736757128249,30.5568408126122,-8.44748694251072));
#47989=CARTESIAN_POINT('Ctrl Pts',(14.2029432110629,30.4529709991461,-8.39820846486423));
#47990=CARTESIAN_POINT('Ctrl Pts',(14.2328774579981,30.3499044844853,-8.34716714015086));
#47991=CARTESIAN_POINT('Ctrl Pts',(14.2410202775501,30.3218679672295,-8.33328269877051));
#47992=CARTESIAN_POINT('Ctrl Pts',(14.2492125117705,30.2938910607097,-8.31926745952062));
#47993=CARTESIAN_POINT('Ctrl Pts',(14.2574530348856,30.2659737110311,-8.30512090606144));
#47994=CARTESIAN_POINT('Ctrl Pts',(14.2670865206991,30.2333372644947,-8.28858304552095));
#47995=CARTESIAN_POINT('Ctrl Pts',(14.2767858699329,30.2007820737878,-8.27186594876041));
#47996=CARTESIAN_POINT('Ctrl Pts',(14.2865492521489,30.1683080065208,-8.25496883936316));
#47997=CARTESIAN_POINT('Ctrl Pts',(14.2893829928678,30.1588826778092,-8.25006459349105));
#47998=CARTESIAN_POINT('Ctrl Pts',(14.292222325135,30.1494635276478,-8.24514484143581));
#47999=CARTESIAN_POINT('Ctrl Pts',(14.2950670737642,30.1400509907427,-8.24020978838424));
#48000=CARTESIAN_POINT('Ctrl Pts',(14.3020236340514,30.1170335333246,-8.2281415888526));
#48001=CARTESIAN_POINT('Ctrl Pts',(14.3090108870272,30.0940614536975,-8.2159847713543));
#48002=CARTESIAN_POINT('Ctrl Pts',(14.3160202505588,30.0711599081366,-8.20375303932115));
#48003=CARTESIAN_POINT('Ctrl Pts',(14.3195972339208,30.0594729058764,-8.19751100296879));
#48004=CARTESIAN_POINT('Ctrl Pts',(14.3231806312391,30.0478021255475,-8.19124831435603));
#48005=CARTESIAN_POINT('Ctrl Pts',(14.3267695230049,30.0361502051769,-8.18496640400546));
#48006=CARTESIAN_POINT('Ctrl Pts',(14.3373838140425,30.00168918433,-8.1663874027196));
#48007=CARTESIAN_POINT('Ctrl Pts',(14.3480518032559,29.9673744337054,-8.14763050023152));
#48008=CARTESIAN_POINT('Ctrl Pts',(14.3587697894377,29.9332076692579,-8.12869793595085));
#48009=CARTESIAN_POINT('Ctrl Pts',(14.3644386177442,29.9151365952559,-8.11868435182325));
#48010=CARTESIAN_POINT('Ctrl Pts',(14.3701214124312,29.8971068793201,-8.10862166579222));
#48011=CARTESIAN_POINT('Ctrl Pts',(14.3758176419001,29.879118802236,-8.09851018473152));
#48012=CARTESIAN_POINT('Ctrl Pts',(14.4131276182726,29.7612979288577,-8.03228056362499));
#48013=CARTESIAN_POINT('Ctrl Pts',(14.4510196947368,29.6452440596771,-7.96394759139418));
#48014=CARTESIAN_POINT('Ctrl Pts',(14.4893852619753,29.5309085105395,-7.89352359406489));
#48015=CARTESIAN_POINT('Ctrl Pts',(14.4923724608226,29.5220061784439,-7.88804027923891));
#48016=CARTESIAN_POINT('Ctrl Pts',(14.4953625194179,29.5131142368237,-7.88254431476432));
#48017=CARTESIAN_POINT('Ctrl Pts',(14.4983553912906,29.5042326741083,-7.8770356952244));
#48018=CARTESIAN_POINT('Ctrl Pts',(14.5397866909133,29.3812823101657,-7.80077808167639));
#48019=CARTESIAN_POINT('Ctrl Pts',(14.5817591054257,29.2603242335815,-7.72209176784764));
#48020=CARTESIAN_POINT('Ctrl Pts',(14.6241433376865,29.1413144445618,-7.64097208577998));
#48021=CARTESIAN_POINT('Ctrl Pts',(14.6665275699472,29.022304655542,-7.55985240371234));
#48022=CARTESIAN_POINT('Ctrl Pts',(14.7093237189971,28.9052431377277,-7.47629941382632));
#48023=CARTESIAN_POINT('Ctrl Pts',(14.7524104879707,28.7901025279864,-7.39028991647064));
#48024=CARTESIAN_POINT('Ctrl Pts',(14.7549211635545,28.783393259121,-7.38527812398457));
#48025=CARTESIAN_POINT('Ctrl Pts',(14.7574328257359,28.7766905125821,-7.38025798958));
#48026=CARTESIAN_POINT('Ctrl Pts',(14.7599454485781,28.7699942792284,-7.37522951202236));
#48027=CARTESIAN_POINT('Ctrl Pts',(14.8005530124361,28.6617736107886,-7.29396215263163));
#48028=CARTESIAN_POINT('Ctrl Pts',(14.8414126162536,28.5552547310724,-7.2105156873878));
#48029=CARTESIAN_POINT('Ctrl Pts',(14.8824237170485,28.4504289161673,-7.12485201694789));
#48030=CARTESIAN_POINT('Ctrl Pts',(14.9259724098299,28.3391169269646,-7.03388784397486));
#48031=CARTESIAN_POINT('Ctrl Pts',(14.969691679003,28.2297133004615,-6.94042438590296));
#48032=CARTESIAN_POINT('Ctrl Pts',(15.0134672850339,28.1222220970918,-6.84439955098032));
#48033=CARTESIAN_POINT('Ctrl Pts',(15.0212656977202,28.1030730586198,-6.82729319064052));
#48034=CARTESIAN_POINT('Ctrl Pts',(15.0290658824068,28.0839846740001,-6.81010556361074));
#48035=CARTESIAN_POINT('Ctrl Pts',(15.0368671643906,28.0649569085011,-6.79283636491335));
#48036=CARTESIAN_POINT('Ctrl Pts',(15.0728575949509,27.9771742242786,-6.71316665192975));
#48037=CARTESIAN_POINT('Ctrl Pts',(15.108872128155,27.8906849392576,-6.63175735053518));
#48038=CARTESIAN_POINT('Ctrl Pts',(15.1448458274244,27.8055007475085,-6.54856071175149));
#48039=CARTESIAN_POINT('Ctrl Pts',(15.1550957132048,27.7812294533839,-6.52485572554879));
#48040=CARTESIAN_POINT('Ctrl Pts',(15.1653425249988,27.7570636708736,-6.50100506088306));
#48041=CARTESIAN_POINT('Ctrl Pts',(15.1755841559372,27.7330051752369,-6.47700899536732));
#48042=CARTESIAN_POINT('Ctrl Pts',(15.1762765507258,27.7313786787247,-6.47538671950028));
#48043=CARTESIAN_POINT('Ctrl Pts',(15.176968933695,27.7297526458408,-6.47376374952505));
#48044=CARTESIAN_POINT('Ctrl Pts',(15.1776612975255,27.7281270926064,-6.47214010149995));
#48045=CARTESIAN_POINT('Ctrl Pts',(15.1884972135519,27.7026861935163,-6.44672902009784));
#48046=CARTESIAN_POINT('Ctrl Pts',(15.1993295170106,27.6773601866701,-6.42114932420259));
#48047=CARTESIAN_POINT('Ctrl Pts',(15.2101297653433,27.6522113320498,-6.39546343288883));
#48048=CARTESIAN_POINT('Ctrl Pts',(15.2102270648348,27.6519847658921,-6.3952320285649));
#48049=CARTESIAN_POINT('Ctrl Pts',(15.2103243621927,27.6517582130066,-6.39500061453552));
#48050=CARTESIAN_POINT('Ctrl Pts',(15.2104216574152,27.6515316733944,-6.39476919080245));
#48051=CARTESIAN_POINT('Ctrl Pts',(15.2218073439199,27.6250215432897,-6.36768751085094));
#48052=CARTESIAN_POINT('Ctrl Pts',(15.233164174659,27.5986923805235,-6.34047202426355));
#48053=CARTESIAN_POINT('Ctrl Pts',(15.2444901971976,27.5725432631787,-6.31312273186159));
#48054=CARTESIAN_POINT('Ctrl Pts',(15.2548441070592,27.5486385249507,-6.28812082961882));
#48055=CARTESIAN_POINT('Ctrl Pts',(15.2651722657739,27.5248842285587,-6.26300711771079));
#48056=CARTESIAN_POINT('Ctrl Pts',(15.2754732056469,27.5012797929199,-6.23778152604866));
#48057=CARTESIAN_POINT('Ctrl Pts',(15.287880939932,27.4728476722624,-6.2073966832686));
#48058=CARTESIAN_POINT('Ctrl Pts',(15.3002492612591,27.4446333351571,-6.17684932533396));
#48059=CARTESIAN_POINT('Ctrl Pts',(15.3125756070521,27.4166357721296,-6.14613929864308));
#48060=CARTESIAN_POINT('Ctrl Pts',(15.3431043357434,27.3472940531772,-6.0700796059574));
#48061=CARTESIAN_POINT('Ctrl Pts',(15.3733751765106,27.2792782283333,-5.99302430475968));
#48062=CARTESIAN_POINT('Ctrl Pts',(15.4033505610025,27.2125834223929,-5.91496498170904));
#48063=CARTESIAN_POINT('Ctrl Pts',(15.4454288718318,27.1189597767709,-5.80538825686893));
#48064=CARTESIAN_POINT('Ctrl Pts',(15.4869241736851,27.0279350941902,-5.69383535682826));
#48065=CARTESIAN_POINT('Ctrl Pts',(15.5277334515159,26.9395021548202,-5.58027802205931));
#48066=CARTESIAN_POINT('Ctrl Pts',(15.5435349373662,26.9052606314599,-5.53630825062664));
#48067=CARTESIAN_POINT('Ctrl Pts',(15.5592336972788,26.871408433392,-5.49203755996307));
#48068=CARTESIAN_POINT('Ctrl Pts',(15.574823623311,26.8379446654303,-5.44746446549149));
#48069=CARTESIAN_POINT('Ctrl Pts',(15.5994965958972,26.7849841428569,-5.37692206935047));
#48070=CARTESIAN_POINT('Ctrl Pts',(15.6238973986934,26.7329965873824,-5.30562234479574));
#48071=CARTESIAN_POINT('Ctrl Pts',(15.6480018369203,26.6819887826648,-5.23355301636256));
#48072=CARTESIAN_POINT('Ctrl Pts',(15.6873369656403,26.5987510591629,-5.11594578220904));
#48073=CARTESIAN_POINT('Ctrl Pts',(15.7258820530778,26.5181175702425,-4.99629189854525));
#48074=CARTESIAN_POINT('Ctrl Pts',(15.7635321084066,26.4401221421386,-4.87453424819488));
#48075=CARTESIAN_POINT('Ctrl Pts',(15.7814963336588,26.4029076566122,-4.81643919792282));
#48076=CARTESIAN_POINT('Ctrl Pts',(15.799257015528,26.3662951462581,-4.7578644141531));
#48077=CARTESIAN_POINT('Ctrl Pts',(15.8168026043343,26.3302880236965,-4.69880361108633));
#48078=CARTESIAN_POINT('Ctrl Pts',(15.8360296778645,26.290830151935,-4.63408270511698));
#48079=CARTESIAN_POINT('Ctrl Pts',(15.8549987958215,26.252099025531,-4.56877841580672));
#48080=CARTESIAN_POINT('Ctrl Pts',(15.8736935430838,26.2141060677325,-4.5028778267482));
#48081=CARTESIAN_POINT('Ctrl Pts',(15.9094481069526,26.1414427887319,-4.37683991955305));
#48082=CARTESIAN_POINT('Ctrl Pts',(15.9441982142166,26.071473598024,-4.2486243383595));
#48083=CARTESIAN_POINT('Ctrl Pts',(15.9778282576488,26.0042788083171,-4.11813863898061));
#48084=CARTESIAN_POINT('Ctrl Pts',(15.99657064445,25.9668304255266,-4.04541754795051));
#48085=CARTESIAN_POINT('Ctrl Pts',(16.0149654186617,25.9302457759999,-3.97199016296204));
#48086=CARTESIAN_POINT('Ctrl Pts',(16.0329923372658,25.8945387960944,-3.89784000610498));
#48087=CARTESIAN_POINT('Ctrl Pts',(16.0473116754131,25.8661756392668,-3.83894024663796));
#48088=CARTESIAN_POINT('Ctrl Pts',(16.0613984893021,25.8383679468724,-3.77958327653742));
#48089=CARTESIAN_POINT('Ctrl Pts',(16.0752417085548,25.8111258267813,-3.71975861341477));
#48090=CARTESIAN_POINT('Ctrl Pts',(16.0776115084942,25.8064622891054,-3.70951731907025));
#48091=CARTESIAN_POINT('Ctrl Pts',(16.0799740221123,25.8018156156547,-3.69926296026429));
#48092=CARTESIAN_POINT('Ctrl Pts',(16.082329545527,25.7971851587797,-3.68899395351471));
#48093=CARTESIAN_POINT('Ctrl Pts',(16.0838593165519,25.7941779550665,-3.68232485021419));
#48094=CARTESIAN_POINT('Ctrl Pts',(16.0853860612706,25.7911777468393,-3.67564986683594));
#48095=CARTESIAN_POINT('Ctrl Pts',(16.0869097019712,25.7881846675679,-3.66896929579596));
#48096=CARTESIAN_POINT('Ctrl Pts',(16.0907794266855,25.7805828800706,-3.65200206011619));
#48097=CARTESIAN_POINT('Ctrl Pts',(16.0946280676787,25.7730291844909,-3.63500339665168));
#48098=CARTESIAN_POINT('Ctrl Pts',(16.0984513321492,25.7655317108836,-3.61799165083566));
#48099=CARTESIAN_POINT('Ctrl Pts',(16.1010438385578,25.760447770569,-3.60645620504334));
#48100=CARTESIAN_POINT('Ctrl Pts',(16.1036256032075,25.7553878660265,-3.5949106355367));
#48101=CARTESIAN_POINT('Ctrl Pts',(16.1061956520486,25.7503538215281,-3.58335898535595));
#48102=CARTESIAN_POINT('Ctrl Pts',(16.1112058941486,25.7405400851994,-3.56083934949041));
#48103=CARTESIAN_POINT('Ctrl Pts',(16.1161742261471,25.7308194838903,-3.53828527581221));
#48104=CARTESIAN_POINT('Ctrl Pts',(16.1210997272461,25.7211931674899,-3.51569958736613));
#48105=CARTESIAN_POINT('Ctrl Pts',(16.1238878355848,25.7157441355057,-3.50291482800349));
#48106=CARTESIAN_POINT('Ctrl Pts',(16.1266622680174,25.7103252359564,-3.4901197249234));
#48107=CARTESIAN_POINT('Ctrl Pts',(16.1294229723656,25.7049364454398,-3.4773142766403));
#48108=CARTESIAN_POINT('Ctrl Pts',(16.1414199393083,25.6815188195244,-3.42166668806785));
#48109=CARTESIAN_POINT('Ctrl Pts',(16.1531576830853,25.6586694316974,-3.36582381852307));
#48110=CARTESIAN_POINT('Ctrl Pts',(16.1646318524645,25.6363874743175,-3.30978527491759));
#48111=CARTESIAN_POINT('Ctrl Pts',(16.1823179306242,25.6020424662609,-3.22340847243103));
#48112=CARTESIAN_POINT('Ctrl Pts',(16.1993778298018,25.569046127284,-3.13656665175364));
#48113=CARTESIAN_POINT('Ctrl Pts',(16.2157956548538,25.5373983162666,-3.04925749651258));
#48114=CARTESIAN_POINT('Ctrl Pts',(16.2255826815076,25.5185323599673,-2.99721058854791));
#48115=CARTESIAN_POINT('Ctrl Pts',(16.2351416656231,25.500144713963,-2.94499782115509));
#48116=CARTESIAN_POINT('Ctrl Pts',(16.2444690004062,25.4822373725231,-2.89261825720388));
#48117=CARTESIAN_POINT('Ctrl Pts',(16.2694430230024,25.4342903050961,-2.7523715046085));
#48118=CARTESIAN_POINT('Ctrl Pts',(16.2927563240971,25.3897821894178,-2.61092958676889));
#48119=CARTESIAN_POINT('Ctrl Pts',(16.3143388732363,25.3487423680397,-2.46827426826731));
#48120=CARTESIAN_POINT('Ctrl Pts',(16.3290674062958,25.320735650111,-2.37092230297782));
#48121=CARTESIAN_POINT('Ctrl Pts',(16.3429899648793,25.2943464232017,-2.27300479163498));
#48122=CARTESIAN_POINT('Ctrl Pts',(16.3560840754507,25.2695873114563,-2.1745145933834));
#48123=CARTESIAN_POINT('Ctrl Pts',(16.3621775026809,25.2580655020991,-2.12868155625828));
#48124=CARTESIAN_POINT('Ctrl Pts',(16.36809158417,25.2468966669633,-2.08272451927544));
#48125=CARTESIAN_POINT('Ctrl Pts',(16.3738237295954,25.2360837950792,-2.03664236952968));
#48126=CARTESIAN_POINT('Ctrl Pts',(16.3918736303947,25.2020352407632,-1.89153470567869));
#48127=CARTESIAN_POINT('Ctrl Pts',(16.4081195618896,25.1715109887614,-1.74518744974002));
#48128=CARTESIAN_POINT('Ctrl Pts',(16.422479453318,25.1445929873555,-1.59756606226281));
#48129=CARTESIAN_POINT('Ctrl Pts',(16.4328873816435,25.1250830467201,-1.49057132432628));
#48130=CARTESIAN_POINT('Ctrl Pts',(16.4423045573777,25.1074701737894,-1.38290671322239));
#48131=CARTESIAN_POINT('Ctrl Pts',(16.4506992102471,25.0917907162153,-1.27455697949911));
#48132=CARTESIAN_POINT('Ctrl Pts',(16.4538867185929,25.0858371166259,-1.23341582859115));
#48133=CARTESIAN_POINT('Ctrl Pts',(16.4569266867854,25.0801628066784,-1.19217577139639));
#48134=CARTESIAN_POINT('Ctrl Pts',(16.4598171317225,25.0747707396732,-1.15083574514861));
#48135=CARTESIAN_POINT('Ctrl Pts',(16.4611299753143,25.0723216563077,-1.13205905514945));
#48136=CARTESIAN_POINT('Ctrl Pts',(16.462411971524,25.0699307471454,-1.11326175181383));
#48137=CARTESIAN_POINT('Ctrl Pts',(16.4636629333543,25.0675982499494,-1.09444373942888));
#48138=CARTESIAN_POINT('Ctrl Pts',(16.4649138951847,25.0652657527534,-1.0756257270439));
#48139=CARTESIAN_POINT('Ctrl Pts',(16.4661340498209,25.0629912442797,-1.05678322505441));
#48140=CARTESIAN_POINT('Ctrl Pts',(16.4673219194188,25.0607773949756,-1.03793713672155));
#48141=CARTESIAN_POINT('Ctrl Pts',(16.4696976586148,25.0563496963676,-1.00024496005579));
#48142=CARTESIAN_POINT('Ctrl Pts',(16.4719451548503,25.0521629702833,-0.962525713485337));
#48143=CARTESIAN_POINT('Ctrl Pts',(16.4740640279585,25.0482172985549,-0.924779372504798));
#48144=CARTESIAN_POINT('Ctrl Pts',(16.4761199328798,25.0443888833974,-0.888154768660442));
#48145=CARTESIAN_POINT('Ctrl Pts',(16.4780547473837,25.0407875238464,-0.851504629468));
#48146=CARTESIAN_POINT('Ctrl Pts',(16.4798681346825,25.0374132198755,-0.814828978053869));
#48147=CARTESIAN_POINT('Ctrl Pts',(16.4817926027118,25.0338322197672,-0.77590672540095));
#48148=CARTESIAN_POINT('Ctrl Pts',(16.4835802779039,25.0305070766299,-0.736955706434156));
#48149=CARTESIAN_POINT('Ctrl Pts',(16.4852306641202,25.0274381872021,-0.697975849237231));
#48150=CARTESIAN_POINT('Ctrl Pts',(16.4868334200033,25.0244578662707,-0.660120955133343));
#48151=CARTESIAN_POINT('Ctrl Pts',(16.4883066964389,25.0217191663817,-0.622238876861686));
#48152=CARTESIAN_POINT('Ctrl Pts',(16.4896500561993,25.0192225741471,-0.584329551221999));
#48153=CARTESIAN_POINT('Ctrl Pts',(16.489672264156,25.0191813013518,-0.58370284742364));
#48154=CARTESIAN_POINT('Ctrl Pts',(16.4896944360742,25.0191400957001,-0.583076151230041));
#48155=CARTESIAN_POINT('Ctrl Pts',(16.4897165719879,25.0190989571266,-0.582449461762879));
#48156=CARTESIAN_POINT('Ctrl Pts',(16.4904036405537,25.0178220719222,-0.562997875556125));
#48157=CARTESIAN_POINT('Ctrl Pts',(16.4910560498663,25.0166097642747,-0.543552782867375));
#48158=CARTESIAN_POINT('Ctrl Pts',(16.4916746257547,25.0154604569063,-0.524087815387606));
#48159=CARTESIAN_POINT('Ctrl Pts',(16.4922416397358,25.0144069510089,-0.506245366450441));
#48160=CARTESIAN_POINT('Ctrl Pts',(16.4927805500429,25.0134057777586,-0.488373007878846));
#48161=CARTESIAN_POINT('Ctrl Pts',(16.4932898396429,25.0124597261385,-0.470521203664524));
#48162=CARTESIAN_POINT('Ctrl Pts',(16.4933360446607,25.0123738961275,-0.468901608581097));
#48163=CARTESIAN_POINT('Ctrl Pts',(16.4933820019059,25.012288527186,-0.467282315369493));
#48164=CARTESIAN_POINT('Ctrl Pts',(16.493427709802,25.0122036222164,-0.465663377919828));
#48165=CARTESIAN_POINT('Ctrl Pts',(16.4945251650366,25.0101650378337,-0.426792383474895));
#48166=CARTESIAN_POINT('Ctrl Pts',(16.4954849227943,25.0083826845251,-0.387926620808362));
#48167=CARTESIAN_POINT('Ctrl Pts',(16.4963070000775,25.0068562319132,-0.349077869818753));
#48168=CARTESIAN_POINT('Ctrl Pts',(16.4970554181005,25.0054665515637,-0.313710020579238));
#48169=CARTESIAN_POINT('Ctrl Pts',(16.4976897549768,25.0042888272114,-0.278356255691909));
#48170=CARTESIAN_POINT('Ctrl Pts',(16.498210217178,25.0033226005218,-0.243025431918962));
#48171=CARTESIAN_POINT('Ctrl Pts',(16.4999726614186,25.0000506613489,-0.123384453707664));
#48172=CARTESIAN_POINT('Ctrl Pts',(16.5004305548395,24.9992010730262,-0.00393429210566608));
#48173=CARTESIAN_POINT('Ctrl Pts',(16.499596954495,25.0007483441252,0.115327096639625));
#48174=CARTESIAN_POINT('Ctrl Pts',(16.4993749034989,25.0011604997717,0.14709544984387));
#48175=CARTESIAN_POINT('Ctrl Pts',(16.4990612127222,25.0017427308057,0.178850407212994));
#48176=CARTESIAN_POINT('Ctrl Pts',(16.4986560772927,25.0024948211525,0.210591977021957));
#48177=CARTESIAN_POINT('Ctrl Pts',(16.4970960245892,25.0053908911909,0.332819060104328));
#48178=CARTESIAN_POINT('Ctrl Pts',(16.494180020726,25.0108042715314,0.454847837492651));
#48179=CARTESIAN_POINT('Ctrl Pts',(16.4899193671244,25.0187223059899,0.576679517355416));
#48180=CARTESIAN_POINT('Ctrl Pts',(16.4889197880066,25.0205799322226,0.605262081080578));
#48181=CARTESIAN_POINT('Ctrl Pts',(16.4878461984108,25.0225754170087,0.633833795606361));
#48182=CARTESIAN_POINT('Ctrl Pts',(16.4866987100243,25.0247087838443,0.662394655330664));
#48183=CARTESIAN_POINT('Ctrl Pts',(16.4817000544053,25.0340020945612,0.786810643869416));
#48184=CARTESIAN_POINT('Ctrl Pts',(16.4752990557455,25.0459105789055,0.911020810466703));
#48185=CARTESIAN_POINT('Ctrl Pts',(16.4675050432796,25.0604360570855,1.03502543425808));
#48186=CARTESIAN_POINT('Ctrl Pts',(16.4658835433093,25.0634580002168,1.06082389104392));
#48187=CARTESIAN_POINT('Ctrl Pts',(16.4642017499146,25.0665932131767,1.08661345083528));
#48188=CARTESIAN_POINT('Ctrl Pts',(16.462459724081,25.0698418499384,1.11239410072457));
#48189=CARTESIAN_POINT('Ctrl Pts',(16.4539313788003,25.085746031989,1.23860708767925));
#48190=CARTESIAN_POINT('Ctrl Pts',(16.4439594021546,25.1043674102929,1.36460664508112));
#48191=CARTESIAN_POINT('Ctrl Pts',(16.4325509764523,25.1257240376614,1.49039203107667));
#48192=CARTESIAN_POINT('Ctrl Pts',(16.4304280078101,25.1296982450929,1.5137991546437));
#48193=CARTESIAN_POINT('Ctrl Pts',(16.4282552963827,25.1337671697023,1.53719886137606));
#48194=CARTESIAN_POINT('Ctrl Pts',(16.4260328727072,25.1379310344828,1.560591134797));
#48195=CARTESIAN_POINT('',(16.4999920017365,20.5440045013611,0.0163625070472239));
#48196=CARTESIAN_POINT('Ctrl Pts',(16.4260328550488,25.1379310203705,1.56059112033272));
#48197=CARTESIAN_POINT('Ctrl Pts',(16.4325781611128,25.0612095504425,1.49169837182591));
#48198=CARTESIAN_POINT('Ctrl Pts',(16.4443923286176,24.904358406813,1.35815502612164));
#48199=CARTESIAN_POINT('Ctrl Pts',(16.4587719843597,24.6590142485308,1.17040662826285));
#48200=CARTESIAN_POINT('Ctrl Pts',(16.470251474698,24.4036762388895,0.995167615974384));
#48201=CARTESIAN_POINT('Ctrl Pts',(16.4762395063454,24.2267833177273,0.886709887603812));
#48202=CARTESIAN_POINT('Ctrl Pts',(16.4795386598462,24.1141229826323,0.821569064101446));
#48203=CARTESIAN_POINT('Ctrl Pts',(16.4801762990835,24.091485733423,0.808673248628822));
#48204=CARTESIAN_POINT('Ctrl Pts',(16.4814090233489,24.046000126645,0.783147417153865));
#48205=CARTESIAN_POINT('Ctrl Pts',(16.4820042698769,24.0231445615983,0.770513634247026));
#48206=CARTESIAN_POINT('Ctrl Pts',(16.4837257714998,23.9543880665996,0.7330816742982));
#48207=CARTESIAN_POINT('Ctrl Pts',(16.4869148522506,23.8160056559258,0.660032469923707));
#48208=CARTESIAN_POINT('Ctrl Pts',(16.4894179646491,23.6750358803599,0.592386407658213));
#48209=CARTESIAN_POINT('Ctrl Pts',(16.4915535542388,23.5323553154947,0.528316178904632));
#48210=CARTESIAN_POINT('Ctrl Pts',(16.4922040416757,23.4845098446298,0.507555720552931));
#48211=CARTESIAN_POINT('Ctrl Pts',(16.4933958339036,23.3882488812412,0.467226741424712));
#48212=CARTESIAN_POINT('Ctrl Pts',(16.4939373899151,23.3398009033332,0.447646619206234));
#48213=CARTESIAN_POINT('Ctrl Pts',(16.4954125301957,23.194122538035,0.390893759436398));
#48214=CARTESIAN_POINT('Ctrl Pts',(16.496986028094,22.998707615173,0.320392791852394));
#48215=CARTESIAN_POINT('Ctrl Pts',(16.4984694808079,22.7021396582226,0.2297772781522));
#48216=CARTESIAN_POINT('Ctrl Pts',(16.4993275684369,22.402181338922,0.154058563252679));
#48217=CARTESIAN_POINT('Ctrl Pts',(16.4997658338623,22.098859610186,0.0931210861774427));
#48218=CARTESIAN_POINT('Ctrl Pts',(16.4999479248813,21.792174258382,0.0469681249854355));
#48219=CARTESIAN_POINT('Ctrl Pts',(16.4999811846693,21.5854566915983,0.0261372463727013));
#48220=CARTESIAN_POINT('Ctrl Pts',(16.4999920914489,21.455540117511,0.0162749117889595));
#48221=CARTESIAN_POINT('Ctrl Pts',(16.4999937468063,21.4295168568963,0.0144601446280865));
#48222=CARTESIAN_POINT('Ctrl Pts',(16.4999963161695,21.3774149533551,0.0111492969632006));
#48223=CARTESIAN_POINT('Ctrl Pts',(16.4999990408472,21.2992639192183,0.00666633889523769));
#48224=CARTESIAN_POINT('Ctrl Pts',(16.5000002603666,21.1169242222562,-0.000419245858196618));
#48225=CARTESIAN_POINT('Ctrl Pts',(16.5000000702348,20.8564753422434,-0.000939509443136404));
#48226=CARTESIAN_POINT('Ctrl Pts',(16.4999993099702,20.6481548381454,0.0088764751499754));
#48227=CARTESIAN_POINT('Ctrl Pts',(16.4999918882417,20.5440044054399,0.0163611721806806));
#48228=CARTESIAN_POINT('',(8.52036860632481,20.5440036583397,-14.1298732767534));
#48229=CARTESIAN_POINT('Origin',(6.61363325216158E-15,20.5440037453176,
8.67361737988404E-16));
#48230=CARTESIAN_POINT('',(6.24602095305321E-15,27.1622780870028,-16.5000001006436));
#48231=CARTESIAN_POINT('Ctrl Pts',(8.52036867104336,20.5440037453176,-14.1298732375596));
#48232=CARTESIAN_POINT('Ctrl Pts',(8.58356973556036,20.6246183822895,-14.0917627491615));
#48233=CARTESIAN_POINT('Ctrl Pts',(8.64460810914305,20.7071305594912,-14.0543784285267));
#48234=CARTESIAN_POINT('Ctrl Pts',(8.71820078920157,20.812702180057,-14.0086857037865));
#48235=CARTESIAN_POINT('Ctrl Pts',(8.73278393179618,20.8339381962245,-13.9995991057947));
#48236=CARTESIAN_POINT('Ctrl Pts',(8.76167886001795,20.8766555969633,-13.9815333163542));
#48237=CARTESIAN_POINT('Ctrl Pts',(8.77598021132686,20.8981217579526,-13.9725606313828));
#48238=CARTESIAN_POINT('Ctrl Pts',(8.8184076223346,20.9627832131134,-13.9458525761399));
#48239=CARTESIAN_POINT('Ctrl Pts',(8.90140518031076,21.0932318928779,-13.8932455450086));
#48240=CARTESIAN_POINT('Ctrl Pts',(9.03052355651088,21.3162917133111,-13.8097792924337));
#48241=CARTESIAN_POINT('Ctrl Pts',(9.17080434164138,21.5931460660356,-13.7169551928144));
#48242=CARTESIAN_POINT('Ctrl Pts',(9.29632299716888,21.8794396203386,-13.6321374667544));
#48243=CARTESIAN_POINT('Ctrl Pts',(9.36997146821566,22.0768411939832,-13.5814347795442));
#48244=CARTESIAN_POINT('Ctrl Pts',(9.42132449791413,22.2274690286921,-13.5458140656644));
#48245=CARTESIAN_POINT('Ctrl Pts',(9.44191187979202,22.2907678651923,-13.5314737738112));
#48246=CARTESIAN_POINT('Ctrl Pts',(9.46146566890013,22.3547580121912,-13.5177915988317));
#48247=CARTESIAN_POINT('Ctrl Pts',(9.46920397396335,22.3804098312845,-13.5123720498178));
#48248=CARTESIAN_POINT('Ctrl Pts',(9.47303319764194,22.3932693111686,-13.5096877608054));
#48249=CARTESIAN_POINT('Ctrl Pts',(9.48438274145507,22.4318890364132,-13.5017246841252));
#48250=CARTESIAN_POINT('Ctrl Pts',(9.52126642056339,22.5608025012239,-13.4757985800892));
#48251=CARTESIAN_POINT('Ctrl Pts',(9.57917707246071,22.7944720582964,-13.4347193862869));
#48252=CARTESIAN_POINT('Ctrl Pts',(9.63851629653991,23.1094990108463,-13.3921717551923));
#48253=CARTESIAN_POINT('Ctrl Pts',(9.68000107488758,23.4280224786546,-13.3621887684031));
#48254=CARTESIAN_POINT('Ctrl Pts',(9.70346143786766,23.750099543279,-13.3451456898397));
#48255=CARTESIAN_POINT('Ctrl Pts',(9.7068399497473,23.9672442799538,-13.342685693239));
#48256=CARTESIAN_POINT('Ctrl Pts',(9.70499841460441,24.1037427373277,-13.3440251041407));
#48257=CARTESIAN_POINT('Ctrl Pts',(9.70443222180082,24.1310828669418,-13.3444368989173));
#48258=CARTESIAN_POINT('Ctrl Pts',(9.70290046268754,24.1858371549446,-13.3455507008099));
#48259=CARTESIAN_POINT('Ctrl Pts',(9.7000109928316,24.2678204701582,-13.3476514275137));
#48260=CARTESIAN_POINT('Ctrl Pts',(9.68916397490106,24.4580880152858,-13.3555317041429));
#48261=CARTESIAN_POINT('Ctrl Pts',(9.66213830977216,24.7270183053258,-13.3751235730946));
#48262=CARTESIAN_POINT('Ctrl Pts',(9.61169454034366,25.0452581559799,-13.4114533409026));
#48263=CARTESIAN_POINT('Ctrl Pts',(9.56620835788032,25.2544954002469,-13.4439075432828));
#48264=CARTESIAN_POINT('Ctrl Pts',(9.52765523426529,25.4103411250022,-13.4712298559432));
#48265=CARTESIAN_POINT('Ctrl Pts',(9.51406393953746,25.462109235537,-13.4808343470393));
#48266=CARTESIAN_POINT('Ctrl Pts',(9.4853960356642,25.5652856616541,-13.5010210497032));
#48267=CARTESIAN_POINT('Ctrl Pts',(9.47031765250651,25.6166997302657,-13.5116045036733));
#48268=CARTESIAN_POINT('Ctrl Pts',(9.42285181695582,25.7703679435337,-13.5447906756782));
#48269=CARTESIAN_POINT('Ctrl Pts',(9.35423263799206,25.9717569689352,-13.5924367699028));
#48270=CARTESIAN_POINT('Ctrl Pts',(9.23589274235606,26.2638847079763,-13.6731842177505));
#48271=CARTESIAN_POINT('Ctrl Pts',(9.10250881132217,26.5464727923424,-13.7624061878736));
#48272=CARTESIAN_POINT('Ctrl Pts',(9.00367297582431,26.7287040698433,-13.8270636691253));
#48273=CARTESIAN_POINT('Ctrl Pts',(8.92582693941875,26.86311490726,-13.8773400779457));
#48274=CARTESIAN_POINT('Ctrl Pts',(8.89925793564753,26.9075411417532,-13.8943962929227));
#48275=CARTESIAN_POINT('Ctrl Pts',(8.85846953453316,26.9736179421189,-13.9204086701232));
#48276=CARTESIAN_POINT('Ctrl Pts',(8.84471258649409,26.9955575542314,-13.9291539631109));
#48277=CARTESIAN_POINT('Ctrl Pts',(8.81690762026432,27.0392155833153,-13.9467706255413));
#48278=CARTESIAN_POINT('Ctrl Pts',(8.74675476164461,27.1476705617355,-13.9910722905394));
#48279=CARTESIAN_POINT('Ctrl Pts',(8.61476617389104,27.3367718819407,-14.0730584659179));
#48280=CARTESIAN_POINT('Ctrl Pts',(8.42682897940193,27.5764190798257,-14.1864547250946));
#48281=CARTESIAN_POINT('Ctrl Pts',(8.22702390985309,27.8039646543995,-14.3033160861774));
#48282=CARTESIAN_POINT('Ctrl Pts',(8.01529570680411,28.0196373988293,-14.4230965455344));
#48283=CARTESIAN_POINT('Ctrl Pts',(7.86606700155189,28.1555579746117,-14.5045702358948));
#48284=CARTESIAN_POINT('Ctrl Pts',(7.77020561634108,28.2380379248674,-14.5559052506994));
#48285=CARTESIAN_POINT('Ctrl Pts',(7.75089034450941,28.2544211982413,-14.5661999638286));
#48286=CARTESIAN_POINT('Ctrl Pts',(7.71207921912852,28.2868721608515,-14.5867856855695));
#48287=CARTESIAN_POINT('Ctrl Pts',(7.65358922171243,28.3350784667842,-14.6176602712913));
#48288=CARTESIAN_POINT('Ctrl Pts',(7.51520251850315,28.4442939198586,-14.6896485772748));
#48289=CARTESIAN_POINT('Ctrl Pts',(7.31206110143769,28.5911128669389,-14.7922039875687));
#48290=CARTESIAN_POINT('Ctrl Pts',(7.0595338938036,28.7528122439669,-14.9144197286055));
#48291=CARTESIAN_POINT('Ctrl Pts',(6.79811902487365,28.9000931027409,-15.0354236930373));
#48292=CARTESIAN_POINT('Ctrl Pts',(6.52759964013339,29.0328506210847,-15.1548791157694));
#48293=CARTESIAN_POINT('Ctrl Pts',(6.34097767462334,29.1114881121681,-15.2332703436679));
#48294=CARTESIAN_POINT('Ctrl Pts',(6.22229167082311,29.157455801492,-15.2818108895932));
#48295=CARTESIAN_POINT('Ctrl Pts',(6.19845201502356,29.1664901400402,-15.2914963053156));
#48296=CARTESIAN_POINT('Ctrl Pts',(6.1505652609305,29.1842373202765,-15.3108201481523));
#48297=CARTESIAN_POINT('Ctrl Pts',(6.12650550559815,29.192954592622,-15.3204635969749));
#48298=CARTESIAN_POINT('Ctrl Pts',(6.05411458449316,29.21858273349,-15.3492799421749));
#48299=CARTESIAN_POINT('Ctrl Pts',(5.90854023930549,29.2677275125996,-15.406436019442));
#48300=CARTESIAN_POINT('Ctrl Pts',(5.76056712447322,29.3105198925897,-15.4621195869495));
#48301=CARTESIAN_POINT('Ctrl Pts',(5.61095373220127,29.3490081544351,-15.5167656792345));
#48302=CARTESIAN_POINT('Ctrl Pts',(5.56080907911311,29.3611197173853,-15.5348081407752));
#48303=CARTESIAN_POINT('Ctrl Pts',(5.48517531992791,29.3781968950826,-15.5616055439635));
#48304=CARTESIAN_POINT('Ctrl Pts',(5.45992174054239,29.383701314867,-15.5704839711456));
#48305=CARTESIAN_POINT('Ctrl Pts',(5.40937365701591,29.3943253639894,-15.5881170494493));
#48306=CARTESIAN_POINT('Ctrl Pts',(5.28286658753632,29.4199307135622,-15.6319025319486));
#48307=CARTESIAN_POINT('Ctrl Pts',(5.05392249571448,29.4574578294063,-15.7080373618841));
#48308=CARTESIAN_POINT('Ctrl Pts',(4.74602717236481,29.4892626374968,-15.8037960831374));
#48309=CARTESIAN_POINT('Ctrl Pts',(4.43547463092405,29.5026830764944,-15.8937570526983));
#48310=CARTESIAN_POINT('Ctrl Pts',(4.12223271289369,29.4973754911404,-15.9778716462655));
#48311=CARTESIAN_POINT('Ctrl Pts',(3.91158214250878,29.4809872600072,-16.0300139016686));
#48312=CARTESIAN_POINT('Ctrl Pts',(3.77934373830044,29.466567150816,-16.0613604558222));
#48313=CARTESIAN_POINT('Ctrl Pts',(3.75284652996683,29.4634712408978,-16.0675722891403));
#48314=CARTESIAN_POINT('Ctrl Pts',(3.69997737442021,29.4568803671405,-16.0798290965113));
#48315=CARTESIAN_POINT('Ctrl Pts',(3.62081101329016,29.4463908628385,-16.0979763101384));
#48316=CARTESIAN_POINT('Ctrl Pts',(3.43704882469573,29.4177128600773,-16.1386741697335));
#48317=CARTESIAN_POINT('Ctrl Pts',(3.17726317966928,29.3648358288221,-16.19222548041));
#48318=CARTESIAN_POINT('Ctrl Pts',(2.86990903950336,29.2824713373728,-16.2494807144156));
#48319=CARTESIAN_POINT('Ctrl Pts',(2.56701318537708,29.1811477696582,-16.3000402857368));
#48320=CARTESIAN_POINT('Ctrl Pts',(2.36813622523175,29.1008034970775,-16.3294779261791));
#48321=CARTESIAN_POINT('Ctrl Pts',(2.22016840429561,29.0356389912742,-16.350025439958));
#48322=CARTESIAN_POINT('Ctrl Pts',(2.14648219853387,29.0018293678555,-16.3599164766422));
#48323=CARTESIAN_POINT('Ctrl Pts',(2.07325316811817,28.9661508133544,-16.3692462842728));
#48324=CARTESIAN_POINT('Ctrl Pts',(2.02453675387829,28.941946133812,-16.375342852792));
#48325=CARTESIAN_POINT('Ctrl Pts',(2.00027966959624,28.9296588123334,-16.3783232300789));
#48326=CARTESIAN_POINT('Ctrl Pts',(1.87964446253043,28.8673778523924,-16.3928760766113));
#48327=CARTESIAN_POINT('Ctrl Pts',(1.6904817909171,28.7621787042267,-16.413966852621));
#48328=CARTESIAN_POINT('Ctrl Pts',(1.41806400209131,28.5881274996996,-16.439677345571));
#48329=CARTESIAN_POINT('Ctrl Pts',(1.15686246306753,28.3980418347844,-16.4600591391421));
#48330=CARTESIAN_POINT('Ctrl Pts',(0.906884940340453,28.1919726464131,-16.4756642554084));
#48331=CARTESIAN_POINT('Ctrl Pts',(0.747798975294972,28.0438617742335,-16.4832287491238));
#48332=CARTESIAN_POINT('Ctrl Pts',(0.660487452314263,27.9574775763779,-16.4867780538133));
#48333=CARTESIAN_POINT('Ctrl Pts',(0.65081639862174,27.9478366294134,-16.4871626151795));
#48334=CARTESIAN_POINT('Ctrl Pts',(0.631534954029398,27.9284690767797,-16.487912441723));
#48335=CARTESIAN_POINT('Ctrl Pts',(0.602691356915125,27.899276349876,-16.4890086703192));
#48336=CARTESIAN_POINT('Ctrl Pts',(0.536287826182138,27.8305242123613,-16.4913578844274));
#48337=CARTESIAN_POINT('Ctrl Pts',(0.407044276552453,27.6904990051635,-16.4952601873013));
#48338=CARTESIAN_POINT('Ctrl Pts',(0.232437371388159,27.4833706236392,-16.498773144052));
#48339=CARTESIAN_POINT('Ctrl Pts',(0.0887795656506141,27.2908969996746,
-16.499907810755));
#48340=CARTESIAN_POINT('Ctrl Pts',(0.0136105057645173,27.1822328811265,
-16.500000075685));
#48341=CARTESIAN_POINT('Ctrl Pts',(6.24602095305321E-15,27.1622780870028,
-16.5000001006436));
#48342=CARTESIAN_POINT('',(-0.948483647701403,24.5,-16.4727162159814));
#48343=CARTESIAN_POINT('Ctrl Pts',(6.24602095305321E-15,27.1622780870028,
-16.5000001006436));
#48344=CARTESIAN_POINT('Ctrl Pts',(-0.0472377228897633,27.0930213634507,
-16.500000187267));
#48345=CARTESIAN_POINT('Ctrl Pts',(-0.151744971279771,26.932023013624,-16.4995362318231));
#48346=CARTESIAN_POINT('Ctrl Pts',(-0.24805737644771,26.7652319559107,-16.4982159706337));
#48347=CARTESIAN_POINT('Ctrl Pts',(-0.325446292899342,26.6216010796214,
-16.4968103092495));
#48348=CARTESIAN_POINT('Ctrl Pts',(-0.356870012161321,26.5611741884442,
-16.4961639215616));
#48349=CARTESIAN_POINT('Ctrl Pts',(-0.387256442555717,26.5000142859108,
-16.4954560075668));
#48350=CARTESIAN_POINT('Ctrl Pts',(-0.399327758053236,26.475491492047,-16.4951681953086));
#48351=CARTESIAN_POINT('Ctrl Pts',(-0.40532387922394,26.4631963125769,-16.495021913523));
#48352=CARTESIAN_POINT('Ctrl Pts',(-0.42316131880117,26.4262757584871,-16.4945771693899));
#48353=CARTESIAN_POINT('Ctrl Pts',(-0.481641589570278,26.3029164586969,
-16.4930545121647));
#48354=CARTESIAN_POINT('Ctrl Pts',(-0.578188697338098,26.0782767729238,
-16.4900107723047));
#48355=CARTESIAN_POINT('Ctrl Pts',(-0.688771519624153,25.7733547477354,
-16.4857218407985));
#48356=CARTESIAN_POINT('Ctrl Pts',(-0.781453084810564,25.463099138679,-16.4815550888826));
#48357=CARTESIAN_POINT('Ctrl Pts',(-0.856288053441708,25.1475226392437,
-16.4778094315988));
#48358=CARTESIAN_POINT('Ctrl Pts',(-0.894191822217506,24.9335626849954,
-16.4757602126714));
#48359=CARTESIAN_POINT('Ctrl Pts',(-0.914067562624034,24.7986994366961,
-16.4746622527135));
#48360=CARTESIAN_POINT('Ctrl Pts',(-0.917851839507087,24.7716698243462,
-16.4744517646284));
#48361=CARTESIAN_POINT('Ctrl Pts',(-0.925036263082085,24.7174959519111,
-16.474049922722));
#48362=CARTESIAN_POINT('Ctrl Pts',(-0.928436494465732,24.6903491769012,
-16.4738585631455));
#48363=CARTESIAN_POINT('Ctrl Pts',(-0.938041179156906,24.6088805414888,
-16.4733153881458));
#48364=CARTESIAN_POINT('Ctrl Pts',(-0.94365634381575,24.5544828879381,-16.4729941445046));
#48365=CARTESIAN_POINT('Ctrl Pts',(-0.948483646373672,24.5,-16.4727161929222));
#48366=CARTESIAN_POINT('',(-12.6567683575148,24.5,-10.5856608081032));
#48367=CARTESIAN_POINT('Origin',(6.61363325216158E-15,24.5,8.67361737988404E-16));
#48368=CARTESIAN_POINT('',(-12.6567683575148,23.5,-10.5856608081032));
#48369=CARTESIAN_POINT('',(-12.6567683575148,52.,-10.5856608081032));
#48370=CARTESIAN_POINT('',(-0.948483680554045,23.5000000000023,-16.4727167864039));
#48371=CARTESIAN_POINT('Origin',(6.61363325216158E-15,23.5,8.67361737988404E-16));
#48372=CARTESIAN_POINT('',(-1.70949320542661E-11,20.8377220411253,-16.5000002469429));
#48373=CARTESIAN_POINT('Ctrl Pts',(-0.948483646373667,23.5,-16.4727161929222));
#48374=CARTESIAN_POINT('Ctrl Pts',(-0.936570751042234,23.3655462479154,
-16.473402126333));
#48375=CARTESIAN_POINT('Ctrl Pts',(-0.919881054270985,23.2317908343366,
-16.4743522007642));
#48376=CARTESIAN_POINT('Ctrl Pts',(-0.887701935566159,23.0322016836209,
-16.4761069634426));
#48377=CARTESIAN_POINT('Ctrl Pts',(-0.875783591794726,22.9658461353017,
-16.4767465113257));
#48378=CARTESIAN_POINT('Ctrl Pts',(-0.859388727144383,22.8831203518824,
-16.4776048561917));
#48379=CARTESIAN_POINT('Ctrl Pts',(-0.856033751776329,22.8665807883718,
-16.4777795223152));
#48380=CARTESIAN_POINT('Ctrl Pts',(-0.849181370413379,22.8335596647343,
-16.478134080361));
#48381=CARTESIAN_POINT('Ctrl Pts',(-0.838688352910079,22.7841101256929,
-16.4786737977762));
#48382=CARTESIAN_POINT('Ctrl Pts',(-0.797863035066176,22.6036956423096,
-16.4807342001022));
#48383=CARTESIAN_POINT('Ctrl Pts',(-0.718348342681733,22.3133396372222,
-16.4844985774509));
#48384=CARTESIAN_POINT('Ctrl Pts',(-0.585692611919195,21.9363933078712,
-16.4898158669865));
#48385=CARTESIAN_POINT('Ctrl Pts',(-0.426443232786663,21.5696178472444,
-16.4947882638331));
#48386=CARTESIAN_POINT('Ctrl Pts',(-0.302290706141837,21.3319736271105,
-16.4973656109522));
#48387=CARTESIAN_POINT('Ctrl Pts',(-0.227236552358115,21.2002907335068,
-16.498437292914));
#48388=CARTESIAN_POINT('Ctrl Pts',(-0.218824617931184,21.1856870077043,
-16.4985510815842));
#48389=CARTESIAN_POINT('Ctrl Pts',(-0.201854838211685,21.1565352459083,
-16.4987674275792));
#48390=CARTESIAN_POINT('Ctrl Pts',(-0.193295857165294,21.1419854169811,
-16.4988699923641));
#48391=CARTESIAN_POINT('Ctrl Pts',(-0.167435923262676,21.0984815372009,
-16.4991594472239));
#48392=CARTESIAN_POINT('Ctrl Pts',(-0.114949217821082,21.0119958671242,
-16.4996658454698));
#48393=CARTESIAN_POINT('Ctrl Pts',(-0.0601661390105475,20.9270736538768,
-16.499933015325));
#48394=CARTESIAN_POINT('Ctrl Pts',(-0.0151228573542697,20.8599822262627,
-16.4999947743784));
#48395=CARTESIAN_POINT('Ctrl Pts',(-0.00758180657007838,20.8488382595036,
-16.5000000179473));
#48396=CARTESIAN_POINT('Ctrl Pts',(6.67038445962762E-15,20.8377220411027,
-16.5000000441008));
#48397=CARTESIAN_POINT('',(0.214930999317485,20.5439968211114,-16.4986004257358));
#48398=CARTESIAN_POINT('Origin',(4.47125871799245,23.8871484228103,-15.8444072749798));
#48399=CARTESIAN_POINT('',(-16.499654466181,20.5440037453176,0.106782473437621));
#48400=CARTESIAN_POINT('Origin',(6.61363325216158E-15,20.5440037453176,
8.67361737988404E-16));
#48401=CARTESIAN_POINT('',(-16.4714285499925,22.,0.970588235294111));
#48402=CARTESIAN_POINT('Ctrl Pts',(-16.499654466181,20.5440037453176,0.106782473437621));
#48403=CARTESIAN_POINT('Ctrl Pts',(-16.4996850755552,20.5535144807161,0.102052819949738));
#48404=CARTESIAN_POINT('Ctrl Pts',(-16.4997126952277,20.5631072668192,0.0974703596247774));
#48405=CARTESIAN_POINT('Ctrl Pts',(-16.4997376258724,20.5727456617118,0.0930496248789231));
#48406=CARTESIAN_POINT('Ctrl Pts',(-16.4997625565171,20.5823840566043,0.0886288901330683));
#48407=CARTESIAN_POINT('Ctrl Pts',(-16.4997848039146,20.5920679507547,0.084369593340066));
#48408=CARTESIAN_POINT('Ctrl Pts',(-16.4998047468791,20.6017971921991,0.0802702612752421));
#48409=CARTESIAN_POINT('Ctrl Pts',(-16.4998049929255,20.6019172267505,0.0802196857511204));
#48410=CARTESIAN_POINT('Ctrl Pts',(-16.4998052386174,20.6020372667433,0.080169135257586));
#48411=CARTESIAN_POINT('Ctrl Pts',(-16.4998054839553,20.6021573121326,0.0801186098125461));
#48412=CARTESIAN_POINT('Ctrl Pts',(-16.4998450097016,20.6214975065332,0.0719785893151182));
#48413=CARTESIAN_POINT('Ctrl Pts',(-16.4998754990255,20.641016717206,0.0644676880107839));
#48414=CARTESIAN_POINT('Ctrl Pts',(-16.4998995537066,20.6607098412591,0.0575735908839684));
#48415=CARTESIAN_POINT('Ctrl Pts',(-16.4998998914639,20.660986356993,0.0574767892631659));
#48416=CARTESIAN_POINT('Ctrl Pts',(-16.4999002279526,20.6612629071222,0.0573801092205637));
#48417=CARTESIAN_POINT('Ctrl Pts',(-16.4999005631797,20.6615394916358,0.0572835507204533));
#48418=CARTESIAN_POINT('Ctrl Pts',(-16.4999482732881,20.7009034849249,0.0435411755571679));
#48419=CARTESIAN_POINT('Ctrl Pts',(-16.4999708656352,20.7409617256664,0.0322534156903742));
#48420=CARTESIAN_POINT('Ctrl Pts',(-16.4999833980792,20.781710378534,0.0234067813658331));
#48421=CARTESIAN_POINT('Ctrl Pts',(-16.4999836034944,20.7823782764952,0.0232617790501028));
#48422=CARTESIAN_POINT('Ctrl Pts',(-16.4999838062025,20.7830463600297,0.0231174328684831));
#48423=CARTESIAN_POINT('Ctrl Pts',(-16.4999840062693,20.7837146291111,0.02297374275987));
#48424=CARTESIAN_POINT('Ctrl Pts',(-16.4999899521532,20.803575243884,0.0187033463386016));
#48425=CARTESIAN_POINT('Ctrl Pts',(-16.499993462673,20.8236002580073,0.0150141556328887));
#48426=CARTESIAN_POINT('Ctrl Pts',(-16.4999956982758,20.8437920839178,0.0119148065284029));
#48427=CARTESIAN_POINT('Ctrl Pts',(-16.499995798485,20.84469716762,0.0117758804909841));
#48428=CARTESIAN_POINT('Ctrl Pts',(-16.4999958961317,20.8456025864146,0.0116381392857442));
#48429=CARTESIAN_POINT('Ctrl Pts',(-16.4999959913199,20.8465083405368,0.0115015837651071));
#48430=CARTESIAN_POINT('Ctrl Pts',(-16.499996993652,20.856045936145,0.0100636534239759));
#48431=CARTESIAN_POINT('Ctrl Pts',(-16.4999977180954,20.8656207442355,0.00875729385934541));
#48432=CARTESIAN_POINT('Ctrl Pts',(-16.4999982570698,20.8752332106515,0.00758408663351017));
#48433=CARTESIAN_POINT('Ctrl Pts',(-16.4999983150879,20.8762679485595,0.00745779625827971));
#48434=CARTESIAN_POINT('Ctrl Pts',(-16.4999983709589,20.8773031577963,0.00733304411345781));
#48435=CARTESIAN_POINT('Ctrl Pts',(-16.4999984247971,20.8783388333972,0.00720983309849447));
#48436=CARTESIAN_POINT('Ctrl Pts',(-16.4999989186003,20.8878380267597,0.00607974443509351));
#48437=CARTESIAN_POINT('Ctrl Pts',(-16.4999992405276,20.8973642148206,0.00508130425039852));
#48438=CARTESIAN_POINT('Ctrl Pts',(-16.4999994608597,20.9068704272133,0.00421826344624561));
#48439=CARTESIAN_POINT('Ctrl Pts',(-16.4999994877968,20.9080326271967,0.00411275075971433));
#48440=CARTESIAN_POINT('Ctrl Pts',(-16.4999995132179,20.9091946134966,0.00400925275482219));
#48441=CARTESIAN_POINT('Ctrl Pts',(-16.4999995372511,20.9103563075049,0.00390777595391313));
#48442=CARTESIAN_POINT('Ctrl Pts',(-16.5000003852682,20.9513468671561,0.00032715073647429));
#48443=CARTESIAN_POINT('Ctrl Pts',(-16.5000000779434,20.9922292246122,-0.000777075137903916));
#48444=CARTESIAN_POINT('Ctrl Pts',(-16.4999999941945,21.0329747879212,0.000528103560881647));
#48445=CARTESIAN_POINT('Ctrl Pts',(-16.499999990816,21.0346184768029,0.000580754881455815));
#48446=CARTESIAN_POINT('Ctrl Pts',(-16.4999999878023,21.0362619608369,0.00063732859592822));
#48447=CARTESIAN_POINT('Ctrl Pts',(-16.499999985244,21.0379052402467,0.000697819978592266));
#48448=CARTESIAN_POINT('Ctrl Pts',(-16.4999999225867,21.0781518367236,0.00217935273184643));
#48449=CARTESIAN_POINT('Ctrl Pts',(-16.5000001351939,21.1182755725363,0.0060110870606543));
#48450=CARTESIAN_POINT('Ctrl Pts',(-16.4999954686141,21.1582742498412,0.0122343404349139));
#48451=CARTESIAN_POINT('Ctrl Pts',(-16.4999952233127,21.1603768029377,0.0125614692685093));
#48452=CARTESIAN_POINT('Ctrl Pts',(-16.4999949645496,21.1624787881589,0.0128951791688783));
#48453=CARTESIAN_POINT('Ctrl Pts',(-16.4999946915747,21.1645802697767,0.0132354829271487));
#48454=CARTESIAN_POINT('Ctrl Pts',(-16.499993325008,21.1751007045472,0.0149391111962692));
#48455=CARTESIAN_POINT('Ctrl Pts',(-16.4999915645246,21.1856084870641,0.0168085463933244));
#48456=CARTESIAN_POINT('Ctrl Pts',(-16.4999892357063,21.1961115765617,0.0188473228317351));
#48457=CARTESIAN_POINT('Ctrl Pts',(-16.4999874242188,21.2042814771213,0.0204331991368735));
#48458=CARTESIAN_POINT('Ctrl Pts',(-16.4999852651097,21.2124588137965,0.0221239408880127));
#48459=CARTESIAN_POINT('Ctrl Pts',(-16.4999826683071,21.2206193345647,0.0239154460820305));
#48460=CARTESIAN_POINT('Ctrl Pts',(-16.4999819294058,21.2229413514076,0.0244252058575302));
#48461=CARTESIAN_POINT('Ctrl Pts',(-16.4999811553101,21.2252612088109,0.0249429486522115));
#48462=CARTESIAN_POINT('Ctrl Pts',(-16.499980343994,21.2275783324658,0.025468565185762));
#48463=CARTESIAN_POINT('Ctrl Pts',(-16.4999739062223,21.2459646482072,0.029639318664803));
#48464=CARTESIAN_POINT('Ctrl Pts',(-16.499965168879,21.2641329203393,0.0342923029695724));
#48465=CARTESIAN_POINT('Ctrl Pts',(-16.4999528955845,21.2821222293978,0.0394268528483906));
#48466=CARTESIAN_POINT('Ctrl Pts',(-16.4999512094238,21.2845936821723,0.0401322605715414));
#48467=CARTESIAN_POINT('Ctrl Pts',(-16.4999494565824,21.2870615167562,0.0408467089387852));
#48468=CARTESIAN_POINT('Ctrl Pts',(-16.499947633876,21.2895257430366,0.0415701738064822));
#48469=CARTESIAN_POINT('Ctrl Pts',(-16.4999195782284,21.3274558582823,0.0527059635781082));
#48470=CARTESIAN_POINT('Ctrl Pts',(-16.4998753415841,21.3645335982835,0.0659717015008427));
#48471=CARTESIAN_POINT('Ctrl Pts',(-16.4997994440263,21.4007641483025,0.0813542360780683));
#48472=CARTESIAN_POINT('Ctrl Pts',(-16.4997938623563,21.4034286210488,0.0824855008291571));
#48473=CARTESIAN_POINT('Ctrl Pts',(-16.4997881092592,21.4060885042182,0.0836282355142637));
#48474=CARTESIAN_POINT('Ctrl Pts',(-16.499782178525,21.40874380041,0.0847824347605743));
#48475=CARTESIAN_POINT('Ctrl Pts',(-16.4997022260076,21.4445399778131,0.100342251065656));
#48476=CARTESIAN_POINT('Ctrl Pts',(-16.4995901346931,21.4795026091028,0.117985016276668));
#48477=CARTESIAN_POINT('Ctrl Pts',(-16.4994246315052,21.5135982764372,0.137793818801735));
#48478=CARTESIAN_POINT('Ctrl Pts',(-16.4994113971708,21.516324710114,0.139377814380164));
#48479=CARTESIAN_POINT('Ctrl Pts',(-16.4993978180569,21.5190461487608,0.140976029923642));
#48480=CARTESIAN_POINT('Ctrl Pts',(-16.4993838850203,21.5217621567528,0.142588269970934));
#48481=CARTESIAN_POINT('Ctrl Pts',(-16.4993510266202,21.5281673417792,0.146390429552292));
#48482=CARTESIAN_POINT('Ctrl Pts',(-16.4993161672843,21.5345419408095,0.150271257276818));
#48483=CARTESIAN_POINT('Ctrl Pts',(-16.4992793247798,21.5408581501453,0.154213193100599));
#48484=CARTESIAN_POINT('Ctrl Pts',(-16.4992635095367,21.5435694855291,0.155905333039508));
#48485=CARTESIAN_POINT('Ctrl Pts',(-16.4992473206821,21.5462714940611,0.157609622888016));
#48486=CARTESIAN_POINT('Ctrl Pts',(-16.4992307576353,21.5489622035107,0.159324845208098));
#48487=CARTESIAN_POINT('Ctrl Pts',(-16.4991923750128,21.5551975590362,0.16329964113873));
#48488=CARTESIAN_POINT('Ctrl Pts',(-16.4991519431483,21.5613804148635,0.167337906081907));
#48489=CARTESIAN_POINT('Ctrl Pts',(-16.499109342362,21.5675089764998,0.171437780545278));
#48490=CARTESIAN_POINT('Ctrl Pts',(-16.4990907943137,21.5701773041687,0.173222833730487));
#48491=CARTESIAN_POINT('Ctrl Pts',(-16.4990718342908,21.5728354457023,0.175019650671196));
#48492=CARTESIAN_POINT('Ctrl Pts',(-16.4990524512606,21.575483432979,0.176828195013071));
#48493=CARTESIAN_POINT('Ctrl Pts',(-16.4989443754721,21.5902480652543,0.186912266185078));
#48494=CARTESIAN_POINT('Ctrl Pts',(-16.4988231621382,21.6046972465362,0.197360668681009));
#48495=CARTESIAN_POINT('Ctrl Pts',(-16.4986867741193,21.6188338672979,0.208170018128185));
#48496=CARTESIAN_POINT('Ctrl Pts',(-16.4986621113215,21.6213901667587,0.210124653159401));
#48497=CARTESIAN_POINT('Ctrl Pts',(-16.4986369521581,21.6239362359053,0.212091100647114));
#48498=CARTESIAN_POINT('Ctrl Pts',(-16.4986112845102,21.6264720928427,0.214069340712306));
#48499=CARTESIAN_POINT('Ctrl Pts',(-16.4983021475512,21.6570135395292,0.237894940884204));
#48500=CARTESIAN_POINT('Ctrl Pts',(-16.4979196123918,21.6860781938654,0.263425997552144));
#48501=CARTESIAN_POINT('Ctrl Pts',(-16.4974392639963,21.7136459342938,0.290685235672527));
#48502=CARTESIAN_POINT('Ctrl Pts',(-16.497400197548,21.7158880021684,0.292902213238513));
#48503=CARTESIAN_POINT('Ctrl Pts',(-16.4973604834622,21.7181201515103,0.295130644757958));
#48504=CARTESIAN_POINT('Ctrl Pts',(-16.4973201084484,21.7203423726231,0.297370542231756));
#48505=CARTESIAN_POINT('Ctrl Pts',(-16.4970916547833,21.7329163511894,0.310044538830837));
#48506=CARTESIAN_POINT('Ctrl Pts',(-16.4968419806759,21.7451714933841,0.323086675437377));
#48507=CARTESIAN_POINT('Ctrl Pts',(-16.4965682638719,21.7571008003871,0.336504926313332));
#48508=CARTESIAN_POINT('Ctrl Pts',(-16.4965213022176,21.7591475143029,0.338807098668096));
#48509=CARTESIAN_POINT('Ctrl Pts',(-16.4964736410885,21.76118427836,0.341119936936436));
#48510=CARTESIAN_POINT('Ctrl Pts',(-16.4964252607106,21.7632113073105,0.343443762192151));
#48511=CARTESIAN_POINT('Ctrl Pts',(-16.4963077302334,21.7681355697923,0.349089032092526));
#48512=CARTESIAN_POINT('Ctrl Pts',(-16.4961858538074,21.7730059618872,0.354803597494513));
#48513=CARTESIAN_POINT('Ctrl Pts',(-16.4960595381071,21.7778168568144,0.360582400563539));
#48514=CARTESIAN_POINT('Ctrl Pts',(-16.496008584632,21.7797574850508,0.362913465485598));
#48515=CARTESIAN_POINT('Ctrl Pts',(-16.4959569121632,21.7816883298161,0.365254813842329));
#48516=CARTESIAN_POINT('Ctrl Pts',(-16.4959045350397,21.7836082214615,0.367605183393828));
#48517=CARTESIAN_POINT('Ctrl Pts',(-16.4958652649051,21.785047674378,0.369367390294314));
#48518=CARTESIAN_POINT('Ctrl Pts',(-16.4958256260704,21.786480009922,0.371133463281377));
#48519=CARTESIAN_POINT('Ctrl Pts',(-16.4957856214331,21.7879050133131,0.372903113111902));
#48520=CARTESIAN_POINT('Ctrl Pts',(-16.4956922600184,21.791230636081,0.377033059612092));
#48521=CARTESIAN_POINT('Ctrl Pts',(-16.495596855473,21.7945180371583,0.38118474027107));
#48522=CARTESIAN_POINT('Ctrl Pts',(-16.495499365647,21.7977677372998,0.385357857057256));
#48523=CARTESIAN_POINT('Ctrl Pts',(-16.4954449712311,21.7995809064064,0.387686246171819));
#48524=CARTESIAN_POINT('Ctrl Pts',(-16.4953899269477,21.8013822834842,0.390021339107209));
#48525=CARTESIAN_POINT('Ctrl Pts',(-16.4953342248032,21.8031719099425,0.392363112479807));
#48526=CARTESIAN_POINT('Ctrl Pts',(-16.4945912578509,21.8270423251592,0.42359817971177));
#48527=CARTESIAN_POINT('Ctrl Pts',(-16.4937314527037,21.8488302173248,0.456017327146848));
#48528=CARTESIAN_POINT('Ctrl Pts',(-16.4927345257884,21.8685708106081,0.489599721324281));
#48529=CARTESIAN_POINT('Ctrl Pts',(-16.4926692122777,21.8698641124863,0.491799866620864));
#48530=CARTESIAN_POINT('Ctrl Pts',(-16.4926033098955,21.8711486154602,0.494005011689312));
#48531=CARTESIAN_POINT('Ctrl Pts',(-16.4925368128699,21.8724243299332,0.49621515106008));
#48532=CARTESIAN_POINT('Ctrl Pts',(-16.491512221602,21.8920806363306,0.530269147916579));
#48533=CARTESIAN_POINT('Ctrl Pts',(-16.490346617639,21.9096504663962,0.565508710461108));
#48534=CARTESIAN_POINT('Ctrl Pts',(-16.4890155715004,21.9250723817395,0.601968047138723));
#48535=CARTESIAN_POINT('Ctrl Pts',(-16.488946257453,21.9258754758924,0.603866662158586));
#48536=CARTESIAN_POINT('Ctrl Pts',(-16.4888764943784,21.9266727342239,0.605768592818671));
#48537=CARTESIAN_POINT('Ctrl Pts',(-16.4888062788131,21.9274641490614,0.607673843251827));
#48538=CARTESIAN_POINT('Ctrl Pts',(-16.488517527398,21.9307187287754,0.615508911683253));
#48539=CARTESIAN_POINT('Ctrl Pts',(-16.4882211081858,21.9338741041944,0.62340032606399));
#48540=CARTESIAN_POINT('Ctrl Pts',(-16.4879167508124,21.9369290908268,0.631348731739397));
#48541=CARTESIAN_POINT('Ctrl Pts',(-16.487848077967,21.9376183943997,0.633142148565797));
#48542=CARTESIAN_POINT('Ctrl Pts',(-16.4877789945818,21.9383026502421,0.63493863384876));
#48543=CARTESIAN_POINT('Ctrl Pts',(-16.4877095008555,21.9389818061129,0.636738105814736));
#48544=CARTESIAN_POINT('Ctrl Pts',(-16.487396103929,21.9420446057924,0.644853212224946));
#48545=CARTESIAN_POINT('Ctrl Pts',(-16.4870740546098,21.9450055504829,0.653036041884953));
#48546=CARTESIAN_POINT('Ctrl Pts',(-16.4867453299528,21.9478453209401,0.661232434512168));
#48547=CARTESIAN_POINT('Ctrl Pts',(-16.4866783910109,21.9484235897912,0.66290148439462));
#48548=CARTESIAN_POINT('Ctrl Pts',(-16.4866111636593,21.9489969449142,0.664571390435223));
#48549=CARTESIAN_POINT('Ctrl Pts',(-16.4865436620896,21.9495652434028,0.666241756430982));
#48550=CARTESIAN_POINT('Ctrl Pts',(-16.4858011779881,21.9558162475649,0.684614961712526));
#48551=CARTESIAN_POINT('Ctrl Pts',(-16.4850234343973,21.9614778442179,0.703099012587878));
#48552=CARTESIAN_POINT('Ctrl Pts',(-16.4842100219045,21.9665568108032,0.721678566231952));
#48553=CARTESIAN_POINT('Ctrl Pts',(-16.4841497338362,21.9669332509083,0.723055635564778));
#48554=CARTESIAN_POINT('Ctrl Pts',(-16.4840892488147,21.9673064991026,0.724433254441731));
#48555=CARTESIAN_POINT('Ctrl Pts',(-16.4840285664534,21.9676765602153,0.725811422028464));
#48556=CARTESIAN_POINT('Ctrl Pts',(-16.4823029170785,21.9782001409525,0.765002943035284));
#48557=CARTESIAN_POINT('Ctrl Pts',(-16.4804177593127,21.9861539386864,0.804636913831577));
#48558=CARTESIAN_POINT('Ctrl Pts',(-16.4783635401719,21.9915540521472,0.844710032025303));
#48559=CARTESIAN_POINT('Ctrl Pts',(-16.4783260674647,21.9916525600749,0.845441038856458));
#48560=CARTESIAN_POINT('Ctrl Pts',(-16.478288538507,21.9917502179696,0.846172191647967));
#48561=CARTESIAN_POINT('Ctrl Pts',(-16.4782509532398,21.9918470259295,0.846903490398947));
#48562=CARTESIAN_POINT('Ctrl Pts',(-16.476155695451,21.9972437584032,0.88767104425426));
#48563=CARTESIAN_POINT('Ctrl Pts',(-16.473885478833,21.9999999929008,0.928892770239698));
#48564=CARTESIAN_POINT('Ctrl Pts',(-16.4714285499925,22.,0.970588235294111));
#48565=CARTESIAN_POINT('',(-16.20259362019,22.0000000000005,3.11864719131614));
#48566=CARTESIAN_POINT('Origin',(6.61363325216158E-15,22.,8.67361737988404E-16));
#48567=CARTESIAN_POINT('',(-12.9440892692056,20.5440037453176,10.2323288156136));
#48568=CARTESIAN_POINT('Ctrl Pts',(-16.2025936491961,22.0000000000008,3.11864719690075));
#48569=CARTESIAN_POINT('Ctrl Pts',(-16.2007285738033,22.0380649929751,3.12833708065861));
#48570=CARTESIAN_POINT('Ctrl Pts',(-16.1987464412966,22.076002889804,3.13858807784552));
#48571=CARTESIAN_POINT('Ctrl Pts',(-16.1966434424578,22.113812826353,3.14940330822996));
#48572=CARTESIAN_POINT('Ctrl Pts',(-16.1954407636136,22.1354358581637,3.15558840378915));
#48573=CARTESIAN_POINT('Ctrl Pts',(-16.1941985162796,22.1570170203631,3.16195812198267));
#48574=CARTESIAN_POINT('Ctrl Pts',(-16.1929158191893,22.1785560753722,3.16851342763732));
#48575=CARTESIAN_POINT('Ctrl Pts',(-16.1923820249429,22.1875195506344,3.17124141733076));
#48576=CARTESIAN_POINT('Ctrl Pts',(-16.1918415464089,22.1964703807905,3.17399990822218));
#48577=CARTESIAN_POINT('Ctrl Pts',(-16.1912942180195,22.2054106120283,3.17678950286713));
#48578=CARTESIAN_POINT('Ctrl Pts',(-16.1903609681165,22.2206546046626,3.18154604205381));
#48579=CARTESIAN_POINT('Ctrl Pts',(-16.1894050293091,22.2359116524264,3.18640708997119));
#48580=CARTESIAN_POINT('Ctrl Pts',(-16.188431284714,22.2510992279796,3.19134650893528));
#48581=CARTESIAN_POINT('Ctrl Pts',(-16.1880901743651,22.2564195545014,3.19307682603722));
#48582=CARTESIAN_POINT('Ctrl Pts',(-16.1877467681858,22.2617332382891,3.19481732744566));
#48583=CARTESIAN_POINT('Ctrl Pts',(-16.1874010331489,22.2670407278125,3.19656812763937));
#48584=CARTESIAN_POINT('Ctrl Pts',(-16.1867593824459,22.2768909137073,3.19981744302596));
#48585=CARTESIAN_POINT('Ctrl Pts',(-16.1861095468107,22.2867219813628,3.20310305888488));
#48586=CARTESIAN_POINT('Ctrl Pts',(-16.1854514865211,22.2965339989238,3.20642482797795));
#48587=CARTESIAN_POINT('Ctrl Pts',(-16.1841491605544,22.3159523492761,3.21299873346044));
#48588=CARTESIAN_POINT('Ctrl Pts',(-16.1828147481359,22.3352962992668,3.21971388856837));
#48589=CARTESIAN_POINT('Ctrl Pts',(-16.1814477998186,22.354566151568,3.22656954932038));
#48590=CARTESIAN_POINT('Ctrl Pts',(-16.1743353285268,22.4548305650421,3.26224075185642));
#48591=CARTESIAN_POINT('Ctrl Pts',(-16.1663424831819,22.5530897779929,3.301714432485));
#48592=CARTESIAN_POINT('Ctrl Pts',(-16.1573962736503,22.6493676325255,3.34492834844848));
#48593=CARTESIAN_POINT('Ctrl Pts',(-16.1559898083244,22.6645038154616,3.35172216142433));
#48594=CARTESIAN_POINT('Ctrl Pts',(-16.154559779912,22.6795910150878,3.3586084292314));
#48595=CARTESIAN_POINT('Ctrl Pts',(-16.1531057632547,22.6946291085995,3.36558724834429));
#48596=CARTESIAN_POINT('Ctrl Pts',(-16.1435883678908,22.793062287306,3.41126772960764));
#48597=CARTESIAN_POINT('Ctrl Pts',(-16.1330447934926,22.8893959143685,3.46090714479232));
#48598=CARTESIAN_POINT('Ctrl Pts',(-16.1213537652987,22.983602889284,3.51453450318926));
#48599=CARTESIAN_POINT('Ctrl Pts',(-16.1198977674386,22.9953354034488,3.52121324160092));
#48600=CARTESIAN_POINT('Ctrl Pts',(-16.1184239776341,23.0070349326023,3.52795382961854));
#48601=CARTESIAN_POINT('Ctrl Pts',(-16.1169320732323,23.0187013074004,3.53475650588613));
#48602=CARTESIAN_POINT('Ctrl Pts',(-16.104683326423,23.1144838997095,3.59060744320198));
#48603=CARTESIAN_POINT('Ctrl Pts',(-16.0912152664552,23.2080355812782,3.65063731207971));
#48604=CARTESIAN_POINT('Ctrl Pts',(-16.0763458930289,23.2992682237434,3.71498354339455));
#48605=CARTESIAN_POINT('Ctrl Pts',(-16.0748618388374,23.3083737981056,3.72140568987996));
#48606=CARTESIAN_POINT('Ctrl Pts',(-16.0733637723816,23.3174562066199,3.72787093347258));
#48607=CARTESIAN_POINT('Ctrl Pts',(-16.071851478507,23.3265153204774,3.73437947411941));
#48608=CARTESIAN_POINT('Ctrl Pts',(-16.0712451133794,23.3301476374644,3.73698912039648));
#48609=CARTESIAN_POINT('Ctrl Pts',(-16.0706364514506,23.3337762715684,3.73960576817669));
#48610=CARTESIAN_POINT('Ctrl Pts',(-16.0700255132432,23.3374010109535,3.74222928262171));
#48611=CARTESIAN_POINT('Ctrl Pts',(-16.0685376647248,23.3462285209347,3.74861845919112));
#48612=CARTESIAN_POINT('Ctrl Pts',(-16.0670366490278,23.3550307520345,3.7550468950703));
#48613=CARTESIAN_POINT('Ctrl Pts',(-16.0655247928919,23.363793655777,3.76150409636277));
#48614=CARTESIAN_POINT('Ctrl Pts',(-16.0648683173262,23.367598668737,3.7643079311789));
#48615=CARTESIAN_POINT('Ctrl Pts',(-16.0642096111748,23.3713973521618,3.76711798752819));
#48616=CARTESIAN_POINT('Ctrl Pts',(-16.063548842397,23.3751886669207,3.76993349913855));
#48617=CARTESIAN_POINT('Ctrl Pts',(-16.0620630117603,23.3837139662545,3.77626456917164));
#48618=CARTESIAN_POINT('Ctrl Pts',(-16.0605660425622,23.392206247396,3.78262627293113));
#48619=CARTESIAN_POINT('Ctrl Pts',(-16.0590580817749,23.4006642630481,3.78901748951433));
#48620=CARTESIAN_POINT('Ctrl Pts',(-16.0561407034788,23.4170275740167,3.80138226497942));
#48621=CARTESIAN_POINT('Ctrl Pts',(-16.053181928325,23.4332641387232,3.81385859904748));
#48622=CARTESIAN_POINT('Ctrl Pts',(-16.0501811226695,23.4493747077355,3.82644559996654));
#48623=CARTESIAN_POINT('Ctrl Pts',(-16.048700186204,23.4573254822511,3.83265744798126));
#48624=CARTESIAN_POINT('Ctrl Pts',(-16.0472090166894,23.4652455849803,3.83889623746635));
#48625=CARTESIAN_POINT('Ctrl Pts',(-16.0457075303997,23.4731350759295,3.84516188518223));
#48626=CARTESIAN_POINT('Ctrl Pts',(-16.0379996871877,23.5136355851095,3.87732643476738));
#48627=CARTESIAN_POINT('Ctrl Pts',(-16.0300200108983,23.5533296060536,3.91019866626501));
#48628=CARTESIAN_POINT('Ctrl Pts',(-16.0217569622216,23.592225091995,3.94376772179914));
#48629=CARTESIAN_POINT('Ctrl Pts',(-16.0202775371902,23.5991889812037,3.94977796123755));
#48630=CARTESIAN_POINT('Ctrl Pts',(-16.0187890414494,23.6061273175812,3.95581050241583));
#48631=CARTESIAN_POINT('Ctrl Pts',(-16.0172913967662,23.6130401043791,3.96186531572998));
#48632=CARTESIAN_POINT('Ctrl Pts',(-15.9988886073062,23.6979831896424,4.03626577659036));
#48633=CARTESIAN_POINT('Ctrl Pts',(-15.9791056210773,23.7790726584468,4.11402593979942));
#48634=CARTESIAN_POINT('Ctrl Pts',(-15.9577944161881,23.856323891952,4.19509205747428));
#48635=CARTESIAN_POINT('Ctrl Pts',(-15.9562633431416,23.8618738963764,4.20091613679774));
#48636=CARTESIAN_POINT('Ctrl Pts',(-15.9547243824016,23.8674040880027,4.20675728039115));
#48637=CARTESIAN_POINT('Ctrl Pts',(-15.9531774663352,23.8729144364266,4.21261549553058));
#48638=CARTESIAN_POINT('Ctrl Pts',(-15.9315756165195,23.9498634847105,4.294422315163));
#48639=CARTESIAN_POINT('Ctrl Pts',(-15.9084236027008,24.0229466751676,4.37955564841957));
#48640=CARTESIAN_POINT('Ctrl Pts',(-15.8835326793682,24.092086587039,4.46804091559637));
#48641=CARTESIAN_POINT('Ctrl Pts',(-15.8818310324434,24.0968132786463,4.4740901360599));
#48642=CARTESIAN_POINT('Ctrl Pts',(-15.8801212452089,24.1015215089774,4.48015504546405));
#48643=CARTESIAN_POINT('Ctrl Pts',(-15.8784032469458,24.1062112288154,4.48623566993863));
#48644=CARTESIAN_POINT('Ctrl Pts',(-15.8667154020255,24.1381162192709,4.52760322973444));
#48645=CARTESIAN_POINT('Ctrl Pts',(-15.854647612731,24.1691649603628,4.5696979166866));
#48646=CARTESIAN_POINT('Ctrl Pts',(-15.8421772586022,24.1993421971384,4.61252855893889));
#48647=CARTESIAN_POINT('Ctrl Pts',(-15.8403248125551,24.2038249650214,4.61889096477889));
#48648=CARTESIAN_POINT('Ctrl Pts',(-15.8384634783031,24.2082884910049,4.62526961845721));
#48649=CARTESIAN_POINT('Ctrl Pts',(-15.8365931763335,24.2127327135982,4.63166455724276));
#48650=CARTESIAN_POINT('Ctrl Pts',(-15.8348597372067,24.2168517218954,4.6375915344283));
#48651=CARTESIAN_POINT('Ctrl Pts',(-15.8331187534389,24.2209537913896,4.64353195877213));
#48652=CARTESIAN_POINT('Ctrl Pts',(-15.8313700238803,24.225039196167,4.64948633366989));
#48653=CARTESIAN_POINT('Ctrl Pts',(-15.8294716493301,24.2294742035238,4.6559502455501));
#48654=CARTESIAN_POINT('Ctrl Pts',(-15.8275633970074,24.2338912489374,4.66243312324216));
#48655=CARTESIAN_POINT('Ctrl Pts',(-15.8256464412423,24.2382874378699,4.6689307713959));
#48656=CARTESIAN_POINT('Ctrl Pts',(-15.8238950452432,24.2423039456306,4.67486724378985));
#48657=CARTESIAN_POINT('Ctrl Pts',(-15.8221363144475,24.2463032099063,4.68081628009433));
#48658=CARTESIAN_POINT('Ctrl Pts',(-15.8203715407341,24.2502821258543,4.68677333707624));
#48659=CARTESIAN_POINT('Ctrl Pts',(-15.8184253822281,24.2546699978282,4.6933426649334));
#48660=CARTESIAN_POINT('Ctrl Pts',(-15.8164722187656,24.2590324257771,4.69992061175821));
#48661=CARTESIAN_POINT('Ctrl Pts',(-15.8145123720079,24.263368748324,4.70650596817048));
#48662=CARTESIAN_POINT('Ctrl Pts',(-15.8090339354155,24.2754902409986,4.72491427351423));
#48663=CARTESIAN_POINT('Ctrl Pts',(-15.8035010071365,24.2874125709219,4.74338811479279));
#48664=CARTESIAN_POINT('Ctrl Pts',(-15.7979130801256,24.2991380625097,4.76192632374751));
#48665=CARTESIAN_POINT('Ctrl Pts',(-15.7958775667432,24.303409305673,4.76867923450323));
#48666=CARTESIAN_POINT('Ctrl Pts',(-15.7938347604507,24.3076544889671,4.77544066605381));
#48667=CARTESIAN_POINT('Ctrl Pts',(-15.791784633935,24.3118736919458,4.78221057381387));
#48668=CARTESIAN_POINT('Ctrl Pts',(-15.7633442780802,24.3704045353914,4.87612603918684));
#48669=CARTESIAN_POINT('Ctrl Pts',(-15.7334953011493,24.4239355410877,4.97167279196691));
#48670=CARTESIAN_POINT('Ctrl Pts',(-15.7021601295571,24.4726571112215,5.06874415074919));
#48671=CARTESIAN_POINT('Ctrl Pts',(-15.699656516845,24.4765498597256,5.0764999432175));
#48672=CARTESIAN_POINT('Ctrl Pts',(-15.6971434172225,24.4804118997891,5.08426546999268));
#48673=CARTESIAN_POINT('Ctrl Pts',(-15.6946207847607,24.4842432686933,5.09204069647819));
#48674=CARTESIAN_POINT('Ctrl Pts',(-15.6634240457132,24.5316248106776,5.18819489863686));
#48675=CARTESIAN_POINT('Ctrl Pts',(-15.6307698276384,24.5743194217589,5.2858316951789));
#48676=CARTESIAN_POINT('Ctrl Pts',(-15.5965690625268,24.6124021579424,5.3848893654224));
#48677=CARTESIAN_POINT('Ctrl Pts',(-15.5933907822553,24.6159411901455,5.39409480389885));
#48678=CARTESIAN_POINT('Ctrl Pts',(-15.5901991470769,24.6194403916291,5.40331251334931));
#48679=CARTESIAN_POINT('Ctrl Pts',(-15.5869940737593,24.6228997410832,5.41254247021877));
#48680=CARTESIAN_POINT('Ctrl Pts',(-15.5530605223862,24.6595254281681,5.51026417096084));
#48681=CARTESIAN_POINT('Ctrl Pts',(-15.5176212035088,24.6916877662491,5.60935762993737));
#48682=CARTESIAN_POINT('Ctrl Pts',(-15.4805748894808,24.7193633611184,5.70979869095014));
#48683=CARTESIAN_POINT('Ctrl Pts',(-15.476469324288,24.7224304397729,5.72092982058731));
#48684=CARTESIAN_POINT('Ctrl Pts',(-15.4723440086735,24.7254423332042,5.73207752534907));
#48685=CARTESIAN_POINT('Ctrl Pts',(-15.4681987867402,24.7283989099965,5.74324180268951));
#48686=CARTESIAN_POINT('Ctrl Pts',(-15.4519326446998,24.740000725009,5.78705121118856));
#48687=CARTESIAN_POINT('Ctrl Pts',(-15.4353600150741,24.7507511884474,5.83111573139675));
#48688=CARTESIAN_POINT('Ctrl Pts',(-15.4184713230428,24.7606424131365,5.87543547837171));
#48689=CARTESIAN_POINT('Ctrl Pts',(-15.4137902225723,24.7633840000196,5.88771974455598));
#48690=CARTESIAN_POINT('Ctrl Pts',(-15.4090848343034,24.7660595443407,5.90002362803513));
#48691=CARTESIAN_POINT('Ctrl Pts',(-15.4043549426926,24.768668821489,5.9123471481084));
#48692=CARTESIAN_POINT('Ctrl Pts',(-15.4037377466213,24.769009301935,5.9139552247411));
#48693=CARTESIAN_POINT('Ctrl Pts',(-15.4031201219804,24.7693486604333,5.91556366528412));
#48694=CARTESIAN_POINT('Ctrl Pts',(-15.4025020739784,24.7696868932433,5.91717245490538));
#48695=CARTESIAN_POINT('Ctrl Pts',(-15.3976639474252,24.7723346052877,5.9297661818648));
#48696=CARTESIAN_POINT('Ctrl Pts',(-15.3928004416522,24.7749128458777,5.94237973041235));
#48697=CARTESIAN_POINT('Ctrl Pts',(-15.3879251262603,24.7774148313734,5.95497777334009));
#48698=CARTESIAN_POINT('Ctrl Pts',(-15.3874066974078,24.7776808862571,5.95631741773523));
#48699=CARTESIAN_POINT('Ctrl Pts',(-15.3868881094435,24.7779460925336,5.95765695307419));
#48700=CARTESIAN_POINT('Ctrl Pts',(-15.3863693767468,24.7782104429972,5.95899634186062));
#48701=CARTESIAN_POINT('Ctrl Pts',(-15.3813867729795,24.7807496190012,5.97186162615066));
#48702=CARTESIAN_POINT('Ctrl Pts',(-15.3763875592422,24.7832116475652,5.98472187761016));
#48703=CARTESIAN_POINT('Ctrl Pts',(-15.3713729754319,24.7855965717697,5.99757391400886));
#48704=CARTESIAN_POINT('Ctrl Pts',(-15.3655247331818,24.7883779819573,6.01256256014777));
#48705=CARTESIAN_POINT('Ctrl Pts',(-15.3596550017188,24.7910548193452,6.02754153987971));
#48706=CARTESIAN_POINT('Ctrl Pts',(-15.353763791016,24.7936280765825,6.04251085639781));
#48707=CARTESIAN_POINT('Ctrl Pts',(-15.3485003517419,24.7959271257744,6.05588503234282));
#48708=CARTESIAN_POINT('Ctrl Pts',(-15.3432197688761,24.7981436780431,6.06925149589424));
#48709=CARTESIAN_POINT('Ctrl Pts',(-15.3379220487496,24.8002782541417,6.08261024575491));
#48710=CARTESIAN_POINT('Ctrl Pts',(-15.2991635046816,24.8158949835662,6.18034392794347));
#48711=CARTESIAN_POINT('Ctrl Pts',(-15.2594875723158,24.8271341266431,6.27766502745761));
#48712=CARTESIAN_POINT('Ctrl Pts',(-15.2188960426122,24.8342169899472,6.37457475006575));
#48713=CARTESIAN_POINT('Ctrl Pts',(-15.2124545056988,24.8353409812271,6.38995351405937));
#48714=CARTESIAN_POINT('Ctrl Pts',(-15.2059899125782,24.8363602703669,6.40532191504176));
#48715=CARTESIAN_POINT('Ctrl Pts',(-15.1995022675384,24.8372753461937,6.42067995159775));
#48716=CARTESIAN_POINT('Ctrl Pts',(-15.1595189390471,24.8429149545807,6.51533146487176));
#48717=CARTESIAN_POINT('Ctrl Pts',(-15.1186599228528,24.8446016656592,6.60958959202436));
#48718=CARTESIAN_POINT('Ctrl Pts',(-15.076925813321,24.8424503931545,6.70345493157287));
#48719=CARTESIAN_POINT('Ctrl Pts',(-15.069215981448,24.8420529736454,6.72079532758813));
#48720=CARTESIAN_POINT('Ctrl Pts',(-15.0614762860052,24.8415245576396,6.73812231536534));
#48721=CARTESIAN_POINT('Ctrl Pts',(-15.0537067262432,24.8408653570098,6.75543589059264));
#48722=CARTESIAN_POINT('Ctrl Pts',(-15.0125937514738,24.8373771672421,6.84705145225807));
#48723=CARTESIAN_POINT('Ctrl Pts',(-14.970644518116,24.8302323129595,6.93829155693857));
#48724=CARTESIAN_POINT('Ctrl Pts',(-14.9278586228369,24.8194623041218,7.02915620374142));
#48725=CARTESIAN_POINT('Ctrl Pts',(-14.9187900350446,24.8171795712252,7.04841521471614));
#48726=CARTESIAN_POINT('Ctrl Pts',(-14.9096838594696,24.8147337373671,7.06765735337678));
#48727=CARTESIAN_POINT('Ctrl Pts',(-14.9005400880507,24.8121245721257,7.08688261044366));
#48728=CARTESIAN_POINT('Ctrl Pts',(-14.8840368164733,24.8074153815087,7.12158160104474));
#48729=CARTESIAN_POINT('Ctrl Pts',(-14.8674110679554,24.8021745077348,7.15622561418776));
#48730=CARTESIAN_POINT('Ctrl Pts',(-14.8506627812048,24.7964006907752,7.19081462415348));
#48731=CARTESIAN_POINT('Ctrl Pts',(-14.8408807561578,24.79302842811,7.2110167240382));
#48732=CARTESIAN_POINT('Ctrl Pts',(-14.831056929161,24.7894742940814,7.23120006011304));
#48733=CARTESIAN_POINT('Ctrl Pts',(-14.8211912848237,24.7857377155243,7.25136462334682));
#48734=CARTESIAN_POINT('Ctrl Pts',(-14.8179315553191,24.7845031042863,7.25802724156755));
#48735=CARTESIAN_POINT('Ctrl Pts',(-14.8146674293716,24.7832486492219,7.26468746547449));
#48736=CARTESIAN_POINT('Ctrl Pts',(-14.8113987894915,24.7819742863765,7.27134553563859));
#48737=CARTESIAN_POINT('Ctrl Pts',(-14.8048178735146,24.7794085479907,7.28475056094716));
#48738=CARTESIAN_POINT('Ctrl Pts',(-14.7982186612007,24.7767621098732,7.29814685649007));
#48739=CARTESIAN_POINT('Ctrl Pts',(-14.7916001771697,24.7740343302663,7.31153637744859));
#48740=CARTESIAN_POINT('Ctrl Pts',(-14.7880142587479,24.7725564094771,7.31879086799941));
#48741=CARTESIAN_POINT('Ctrl Pts',(-14.7844216216961,24.7710541341929,7.32604549272862));
#48742=CARTESIAN_POINT('Ctrl Pts',(-14.7808248885348,24.7695286159718,7.33329498920607));
#48743=CARTESIAN_POINT('Ctrl Pts',(-14.7777839200856,24.7682388197677,7.33942429851873));
#48744=CARTESIAN_POINT('Ctrl Pts',(-14.7747407828823,24.7669327178474,7.3455484114189));
#48745=CARTESIAN_POINT('Ctrl Pts',(-14.7716970861947,24.7656110144841,7.35166411050637));
#48746=CARTESIAN_POINT('Ctrl Pts',(-14.761196250836,24.7610511023656,7.37276343669141));
#48747=CARTESIAN_POINT('Ctrl Pts',(-14.7506837912226,24.7563041603517,7.39377288964028));
#48748=CARTESIAN_POINT('Ctrl Pts',(-14.7401572275992,24.7513709251904,7.41469939794161));
#48749=CARTESIAN_POINT('Ctrl Pts',(-14.6973102122001,24.7312908296831,7.49987804270287));
#48750=CARTESIAN_POINT('Ctrl Pts',(-14.6542479183378,24.7081389531941,7.58364572268321));
#48751=CARTESIAN_POINT('Ctrl Pts',(-14.6110004483275,24.6820430612744,7.66607239067015));
#48752=CARTESIAN_POINT('Ctrl Pts',(-14.5994294499354,24.6750610222471,7.68812590830979));
#48753=CARTESIAN_POINT('Ctrl Pts',(-14.5878451889963,24.6678681797709,7.71008339601883));
#48754=CARTESIAN_POINT('Ctrl Pts',(-14.5762483668385,24.6604656595606,7.73194574887356));
#48755=CARTESIAN_POINT('Ctrl Pts',(-14.5336920324701,24.6333009655649,7.81217303747932));
#48756=CARTESIAN_POINT('Ctrl Pts',(-14.4909656746514,24.6033180861438,7.89112095375525));
#48757=CARTESIAN_POINT('Ctrl Pts',(-14.4481043018837,24.5705726924211,7.9688319145224));
#48758=CARTESIAN_POINT('Ctrl Pts',(-14.435631055481,24.5610433344449,7.99144686824979));
#48759=CARTESIAN_POINT('Ctrl Pts',(-14.4231463598431,24.551280024261,8.01395704999258));
#48760=CARTESIAN_POINT('Ctrl Pts',(-14.4106512663725,24.5412826396292,8.03636303047209));
#48761=CARTESIAN_POINT('Ctrl Pts',(-14.368350330057,24.5074374561882,8.1122163208515));
#48762=CARTESIAN_POINT('Ctrl Pts',(-14.3259294292655,24.4709147430595,8.18687686290484));
#48763=CARTESIAN_POINT('Ctrl Pts',(-14.2834297196491,24.4317100865886,8.26036533355924));
#48764=CARTESIAN_POINT('Ctrl Pts',(-14.2702374163509,24.4195405982901,8.28317683515631));
#48765=CARTESIAN_POINT('Ctrl Pts',(-14.2570374921994,24.4071127715725,8.30587540847742));
#48766=CARTESIAN_POINT('Ctrl Pts',(-14.2438314706936,24.3944246468114,8.32846112690485));
#48767=CARTESIAN_POINT('Ctrl Pts',(-14.2159565081634,24.3676428486639,8.37613453517622));
#48768=CARTESIAN_POINT('Ctrl Pts',(-14.1880541401679,24.3397031404335,8.4233055533928));
#48769=CARTESIAN_POINT('Ctrl Pts',(-14.1601384898672,24.3105891204553,8.46997506646264));
#48770=CARTESIAN_POINT('Ctrl Pts',(-14.1461806647169,24.2960321104662,8.49330982299757));
#48771=CARTESIAN_POINT('Ctrl Pts',(-14.1322195167082,24.2811815214874,8.51651920302677));
#48772=CARTESIAN_POINT('Ctrl Pts',(-14.1182570229551,24.2660341768511,8.53960295526646));
#48773=CARTESIAN_POINT('Ctrl Pts',(-14.1180026993283,24.2657582714368,8.54002342052814));
#48774=CARTESIAN_POINT('Ctrl Pts',(-14.1177483689363,24.2654822610159,8.54044385455583));
#48775=CARTESIAN_POINT('Ctrl Pts',(-14.1174940323106,24.2652061461278,8.54086425648329));
#48776=CARTESIAN_POINT('Ctrl Pts',(-14.1107667652363,24.2579028385899,8.55198399213569));
#48777=CARTESIAN_POINT('Ctrl Pts',(-14.1040377514951,24.2505288686595,8.56307686259749));
#48778=CARTESIAN_POINT('Ctrl Pts',(-14.0973217926706,24.243100392135,8.57411904861985));
#48779=CARTESIAN_POINT('Ctrl Pts',(-14.0903519247494,24.2353910684802,8.58557870466419));
#48780=CARTESIAN_POINT('Ctrl Pts',(-14.0833932795755,24.2276198183536,8.59698848455036));
#48781=CARTESIAN_POINT('Ctrl Pts',(-14.0764459696852,24.2197869328603,8.60834878828686));
#48782=CARTESIAN_POINT('Ctrl Pts',(-14.0762845790342,24.2196049696963,8.60861269573363));
#48783=CARTESIAN_POINT('Ctrl Pts',(-14.0761231961318,24.2194229749766,8.60887657380321));
#48784=CARTESIAN_POINT('Ctrl Pts',(-14.07596182105,24.2192409487787,8.60914042238491));
#48785=CARTESIAN_POINT('Ctrl Pts',(-14.0621446620437,24.2036556124843,8.63173150501409));
#48786=CARTESIAN_POINT('Ctrl Pts',(-14.0483724087833,24.1878261032494,8.65412699149244));
#48787=CARTESIAN_POINT('Ctrl Pts',(-14.0346469182352,24.171753729845,8.67632905556684));
#48788=CARTESIAN_POINT('Ctrl Pts',(-14.0071500385025,24.1395552363216,8.72080742838211));
#48789=CARTESIAN_POINT('Ctrl Pts',(-13.9798407035581,24.10638250377,8.76450982437772));
#48790=CARTESIAN_POINT('Ctrl Pts',(-13.9527353713041,24.0722403709581,8.80745000884873));
#48791=CARTESIAN_POINT('Ctrl Pts',(-13.939110440033,24.0550782786933,8.82903458330466));
#48792=CARTESIAN_POINT('Ctrl Pts',(-13.9255368723932,24.037671755944,8.85042686711888));
#48793=CARTESIAN_POINT('Ctrl Pts',(-13.9120172216432,24.0200199465187,8.87162769785873));
#48794=CARTESIAN_POINT('Ctrl Pts',(-13.8715627914303,23.9672009864928,8.93506628391983));
#48795=CARTESIAN_POINT('Ctrl Pts',(-13.8315892997756,23.9121884637842,8.99679365402703));
#48796=CARTESIAN_POINT('Ctrl Pts',(-13.792165484045,23.8549566280595,9.05683008898569));
#48797=CARTESIAN_POINT('Ctrl Pts',(-13.7789671094322,23.8357964530822,9.0769291926446));
#48798=CARTESIAN_POINT('Ctrl Pts',(-13.7658302672435,23.816387664989,9.09683881806451));
#48799=CARTESIAN_POINT('Ctrl Pts',(-13.7527583233579,23.7967271682685,9.11655844889056));
#48800=CARTESIAN_POINT('Ctrl Pts',(-13.7134944654266,23.7376734455135,9.17578979122058));
#48801=CARTESIAN_POINT('Ctrl Pts',(-13.6748140062712,23.6763543421238,9.23331031479049));
#48802=CARTESIAN_POINT('Ctrl Pts',(-13.6368080138338,23.6126902613882,9.28910475739456));
#48803=CARTESIAN_POINT('Ctrl Pts',(-13.6243655648898,23.5918478356728,9.30737081121752));
#48804=CARTESIAN_POINT('Ctrl Pts',(-13.6119956065496,23.5707535567129,9.32545155666013));
#48805=CARTESIAN_POINT('Ctrl Pts',(-13.5997020461054,23.5494028742049,9.34334544254682));
#48806=CARTESIAN_POINT('Ctrl Pts',(-13.5872408544575,23.5277610603664,9.36148332394995));
#48807=CARTESIAN_POINT('Ctrl Pts',(-13.5748580142948,23.5058562285921,9.37942942446946));
#48808=CARTESIAN_POINT('Ctrl Pts',(-13.5625576774649,23.4836835500919,9.39718198423395));
#48809=CARTESIAN_POINT('Ctrl Pts',(-13.5622002858085,23.4830393132384,9.39769779260794));
#48810=CARTESIAN_POINT('Ctrl Pts',(-13.5618429499553,23.4823948255231,9.39821345757555));
#48811=CARTESIAN_POINT('Ctrl Pts',(-13.5614856716924,23.4817500898084,9.39872897664797));
#48812=CARTESIAN_POINT('Ctrl Pts',(-13.5556947328696,23.4712999016273,9.40708475901662));
#48813=CARTESIAN_POINT('Ctrl Pts',(-13.5499210866683,23.4607881047525,9.41539904702796));
#48814=CARTESIAN_POINT('Ctrl Pts',(-13.5441763047212,23.4502351047131,9.4236557490121));
#48815=CARTESIAN_POINT('Ctrl Pts',(-13.5380770922097,23.4390310258696,9.43242185719667));
#48816=CARTESIAN_POINT('Ctrl Pts',(-13.5320084142969,23.4277769507785,9.44112595533259));
#48817=CARTESIAN_POINT('Ctrl Pts',(-13.5259706946607,23.4164726630393,9.44976807943773));
#48818=CARTESIAN_POINT('Ctrl Pts',(-13.5255027633295,23.4155965656501,9.45043785559172));
#48819=CARTESIAN_POINT('Ctrl Pts',(-13.5250350313337,23.4147201914592,9.45110724028288));
#48820=CARTESIAN_POINT('Ctrl Pts',(-13.5245675011861,23.4138435446244,9.45177623020461));
#48821=CARTESIAN_POINT('Ctrl Pts',(-13.5123698737289,23.3909722676434,9.46922984229624));
#48822=CARTESIAN_POINT('Ctrl Pts',(-13.500298009852,23.3678945493989,9.48643154991876));
#48823=CARTESIAN_POINT('Ctrl Pts',(-13.4883559012739,23.3446105257168,9.50338124461869));
#48824=CARTESIAN_POINT('Ctrl Pts',(-13.4771310581609,23.3227249842178,9.51931290882832));
#48825=CARTESIAN_POINT('Ctrl Pts',(-13.4660205123182,23.3006577021536,9.5350224652864));
#48826=CARTESIAN_POINT('Ctrl Pts',(-13.4550281249885,23.2784079358377,9.5505089073953));
#48827=CARTESIAN_POINT('Ctrl Pts',(-13.4190914907655,23.2056683489166,9.60113763696881));
#48828=CARTESIAN_POINT('Ctrl Pts',(-13.3844104675413,23.1309760363863,9.64939219710768));
#48829=CARTESIAN_POINT('Ctrl Pts',(-13.351102074414,23.0542737878051,9.69526035744458));
#48830=CARTESIAN_POINT('Ctrl Pts',(-13.3415236222338,23.0322166198911,9.7084506058815));
#48831=CARTESIAN_POINT('Ctrl Pts',(-13.3320585708577,23.0099933738321,9.72144360699642));
#48832=CARTESIAN_POINT('Ctrl Pts',(-13.3227106391527,22.9876013095394,9.7342376265637));
#48833=CARTESIAN_POINT('Ctrl Pts',(-13.2893807312244,22.9077627458071,9.77985450820822));
#48834=CARTESIAN_POINT('Ctrl Pts',(-13.2575356335838,22.8257836447286,9.82294763255116));
#48835=CARTESIAN_POINT('Ctrl Pts',(-13.2273415092598,22.7415472155431,9.86343938985887));
#48836=CARTESIAN_POINT('Ctrl Pts',(-13.2196187511697,22.7200020447678,9.87379597589437));
#48837=CARTESIAN_POINT('Ctrl Pts',(-13.2120043126901,22.6983087533948,9.88398192053575));
#48838=CARTESIAN_POINT('Ctrl Pts',(-13.2045015037799,22.6764646402634,9.89399515055105));
#48839=CARTESIAN_POINT('Ctrl Pts',(-13.2025807266856,22.6708723783987,9.89655861485929));
#48840=CARTESIAN_POINT('Ctrl Pts',(-13.2006673073772,22.6652703809769,9.89911070390188));
#48841=CARTESIAN_POINT('Ctrl Pts',(-13.198761277514,22.6596585418442,9.90165141474883));
#48842=CARTESIAN_POINT('Ctrl Pts',(-13.1940803008402,22.6458765499752,9.90789109044276));
#48843=CARTESIAN_POINT('Ctrl Pts',(-13.1894438989135,22.632035190591,9.91406213189617));
#48844=CARTESIAN_POINT('Ctrl Pts',(-13.1848526053688,22.6181327976104,9.92016440260441));
#48845=CARTESIAN_POINT('Ctrl Pts',(-13.1823499568869,22.6105548019219,9.92349066313972));
#48846=CARTESIAN_POINT('Ctrl Pts',(-13.179859834685,22.6029559187992,9.92679765089893));
#48847=CARTESIAN_POINT('Ctrl Pts',(-13.1773841523027,22.5953415704692,9.93008292268043));
#48848=CARTESIAN_POINT('Ctrl Pts',(-13.1753150145708,22.5889776137895,9.93282870293533));
#48849=CARTESIAN_POINT('Ctrl Pts',(-13.173255856113,22.5826025218678,9.93555945631742));
#48850=CARTESIAN_POINT('Ctrl Pts',(-13.1712079133685,22.5762198102661,9.93827359770395));
#48851=CARTESIAN_POINT('Ctrl Pts',(-13.1688678331854,22.5689266098223,9.94137490924681));
#48852=CARTESIAN_POINT('Ctrl Pts',(-13.1665425556495,22.5616240730917,9.94445432949206));
#48853=CARTESIAN_POINT('Ctrl Pts',(-13.1642322713302,22.5543125982023,9.947511695335));
#48854=CARTESIAN_POINT('Ctrl Pts',(-13.1599001203913,22.5406024186617,9.95324474308009));
#48855=CARTESIAN_POINT('Ctrl Pts',(-13.1556201306553,22.5268590117228,9.95890098193524));
#48856=CARTESIAN_POINT('Ctrl Pts',(-13.1513926252604,22.5130823508635,9.96448056704778));
#48857=CARTESIAN_POINT('Ctrl Pts',(-13.140516049515,22.4776375953031,9.97883578943898));
#48858=CARTESIAN_POINT('Ctrl Pts',(-13.1299870882692,22.4419725804668,9.99268335057632));
#48859=CARTESIAN_POINT('Ctrl Pts',(-13.119812808503,22.4060859326332,10.0060237791964));
#48860=CARTESIAN_POINT('Ctrl Pts',(-13.1141689397606,22.3861789186108,10.0134239716256));
#48861=CARTESIAN_POINT('Ctrl Pts',(-13.1086340371467,22.3662038533071,10.0206684376741));
#48862=CARTESIAN_POINT('Ctrl Pts',(-13.1032096331651,22.3461602255949,10.0277566190844));
#48863=CARTESIAN_POINT('Ctrl Pts',(-13.0773232529071,22.2505078791861,10.0615828901267));
#48864=CARTESIAN_POINT('Ctrl Pts',(-13.053948109445,22.1532971922261,10.0918570257584));
#48865=CARTESIAN_POINT('Ctrl Pts',(-13.0332474114134,22.0544759208489,10.1185207373871));
#48866=CARTESIAN_POINT('Ctrl Pts',(-13.0296331007545,22.0372218758926,10.1231761812276));
#48867=CARTESIAN_POINT('Ctrl Pts',(-13.0261002717855,22.0199187719173,10.1277216224077));
#48868=CARTESIAN_POINT('Ctrl Pts',(-13.022650085095,22.0025660932098,10.1321561991668));
#48869=CARTESIAN_POINT('Ctrl Pts',(-13.0020944629492,21.8991818016561,10.1585766489604));
#48870=CARTESIAN_POINT('Ctrl Pts',(-12.9844670907416,21.7940409596459,10.1810687787178));
#48871=CARTESIAN_POINT('Ctrl Pts',(-12.9700083867339,21.6870408589478,10.1994550074039));
#48872=CARTESIAN_POINT('Ctrl Pts',(-12.9681406962007,21.6732192138671,10.2018300325264));
#48873=CARTESIAN_POINT('Ctrl Pts',(-12.9663259866237,21.65936645822,10.2041363436325));
#48874=CARTESIAN_POINT('Ctrl Pts',(-12.9645648615698,21.6454823027918,10.206373398571));
#48875=CARTESIAN_POINT('Ctrl Pts',(-12.9643305992097,21.6436354521025,10.2066709684504));
#48876=CARTESIAN_POINT('Ctrl Pts',(-12.9640972861417,21.6417880600603,10.2069673114271));
#48877=CARTESIAN_POINT('Ctrl Pts',(-12.9638649230306,21.6399401205276,10.2072624271848));
#48878=CARTESIAN_POINT('Ctrl Pts',(-12.9618845878823,21.6241908925574,10.2097775773093));
#48879=CARTESIAN_POINT('Ctrl Pts',(-12.9599718992166,21.6083902294373,10.2122053056697));
#48880=CARTESIAN_POINT('Ctrl Pts',(-12.9581319554774,21.5925740951444,10.2145394523902));
#48881=CARTESIAN_POINT('Ctrl Pts',(-12.9566409127781,21.5797571100018,10.2164309843715));
#48882=CARTESIAN_POINT('Ctrl Pts',(-12.9551986494885,21.5669393234458,10.2182597889915));
#48883=CARTESIAN_POINT('Ctrl Pts',(-12.9538049100276,21.5541189441617,10.2200263443705));
#48884=CARTESIAN_POINT('Ctrl Pts',(-12.9517580067449,21.5352904061316,10.2226207804944));
#48885=CARTESIAN_POINT('Ctrl Pts',(-12.949815968165,21.5164579315467,10.2250806929422));
#48886=CARTESIAN_POINT('Ctrl Pts',(-12.9479786258968,21.4976215359301,10.2274067829201));
#48887=CARTESIAN_POINT('Ctrl Pts',(-12.946839985827,21.4859482210606,10.2288483103375));
#48888=CARTESIAN_POINT('Ctrl Pts',(-12.9457415466821,21.4742734009023,10.2302384667876));
#48889=CARTESIAN_POINT('Ctrl Pts',(-12.9446832872844,21.4625970774996,10.2315773638437));
#48890=CARTESIAN_POINT('Ctrl Pts',(-12.9400000881751,21.410924918974,10.2375024910041));
#48891=CARTESIAN_POINT('Ctrl Pts',(-12.9361036268393,21.359223297895,10.2424239343794));
#48892=CARTESIAN_POINT('Ctrl Pts',(-12.9329927241096,21.3074924518508,10.2463505307075));
#48893=CARTESIAN_POINT('Ctrl Pts',(-12.9324290289144,21.2981188288556,10.2470620294834));
#48894=CARTESIAN_POINT('Ctrl Pts',(-12.9318911062848,21.2887442482392,10.2477409236525));
#48895=CARTESIAN_POINT('Ctrl Pts',(-12.9313789674242,21.2793687105475,10.2483872117065));
#48896=CARTESIAN_POINT('Ctrl Pts',(-12.9249592111551,21.1618445945224,10.2564885531696));
#48897=CARTESIAN_POINT('Ctrl Pts',(-12.9225871454633,21.0441697906819,10.2594711806111));
#48898=CARTESIAN_POINT('Ctrl Pts',(-12.924282557788,20.9263441761685,10.2573349543856));
#48899=CARTESIAN_POINT('Ctrl Pts',(-12.9243505015238,20.9216223086244,10.2572493450101));
#48900=CARTESIAN_POINT('Ctrl Pts',(-12.9244249772314,20.9169001978544,10.2571555157621));
#48901=CARTESIAN_POINT('Ctrl Pts',(-12.9245059893016,20.9121778438395,10.2570534574116));
#48902=CARTESIAN_POINT('Ctrl Pts',(-12.9266085102063,20.7896177363176,10.2544047185896));
#48903=CARTESIAN_POINT('Ctrl Pts',(-12.9331112218386,20.6668943505176,10.246216252939));
#48904=CARTESIAN_POINT('Ctrl Pts',(-12.9440892692056,20.5440037453176,10.2323288156136));
#48905=CARTESIAN_POINT('Origin',(6.61363325216158E-15,20.5440037453176,
8.67361737988404E-16));
#48906=CARTESIAN_POINT('',(-10.3714285714286,51.,-12.8329057265981));
#48907=CARTESIAN_POINT('Origin',(6.61363325216158E-15,51.,8.67361737988404E-16));
#48908=CARTESIAN_POINT('',(-10.3714285714286,38.7323075626015,-12.8329057265981));
#48909=CARTESIAN_POINT('',(-10.3714285714286,52.,-12.8329057265981));
#48910=CARTESIAN_POINT('',(-6.12857142857143,38.7323075626015,-15.3196152773136));
#48911=CARTESIAN_POINT('Origin',(6.61363325216158E-15,38.7323075626015,
8.67361737988404E-16));
#48912=CARTESIAN_POINT('',(-4.71428571428571,40.2323075626015,-15.8121949837485));
#48913=CARTESIAN_POINT('Ctrl Pts',(-6.1285714285714,38.7323075626015,-15.3196152773135));
#48914=CARTESIAN_POINT('Ctrl Pts',(-6.08389803240923,38.732307564115,-15.3374867508708));
#48915=CARTESIAN_POINT('Ctrl Pts',(-6.03943307100923,38.7345475002831,-15.3550481877686));
#48916=CARTESIAN_POINT('Ctrl Pts',(-5.99517535721625,38.7389948597807,-15.3723086241536));
#48917=CARTESIAN_POINT('Ctrl Pts',(-5.95085559139461,38.743448454749,-15.3895932607289));
#48918=CARTESIAN_POINT('Ctrl Pts',(-5.90674351021535,38.7501152623945,-15.4065760832571));
#48919=CARTESIAN_POINT('Ctrl Pts',(-5.86284535065981,38.7590216606717,-15.4232630916498));
#48920=CARTESIAN_POINT('Ctrl Pts',(-5.84087298176195,38.7634795848872,-15.4316154487399));
#48921=CARTESIAN_POINT('Ctrl Pts',(-5.8189543016697,38.7684994073214,-15.4398936577168));
#48922=CARTESIAN_POINT('Ctrl Pts',(-5.79709081670919,38.7740900839308,-15.4480982021357));
#48923=CARTESIAN_POINT('Ctrl Pts',(-5.79402296690483,38.7748745588749,-15.4492494508975));
#48924=CARTESIAN_POINT('Ctrl Pts',(-5.79095620446294,38.7756702787681,-15.4503992490416));
#48925=CARTESIAN_POINT('Ctrl Pts',(-5.78789053458143,38.7764772771096,-15.4515475975481));
#48926=CARTESIAN_POINT('Ctrl Pts',(-5.78002619336392,38.7785474642351,-15.4544934478322));
#48927=CARTESIAN_POINT('Ctrl Pts',(-5.77216887004003,38.780691882803,-15.4574298223162));
#48928=CARTESIAN_POINT('Ctrl Pts',(-5.76431958430387,38.7829108473491,-15.4603563907826));
#48929=CARTESIAN_POINT('Ctrl Pts',(-5.76097517290875,38.7838563002938,-15.4616033384994));
#48930=CARTESIAN_POINT('Ctrl Pts',(-5.75763116042156,38.7848156307194,-15.4628488974097));
#48931=CARTESIAN_POINT('Ctrl Pts',(-5.75428915114725,38.7857883786975,-15.4640924786037));
#48932=CARTESIAN_POINT('Ctrl Pts',(-5.74672518435317,38.7879899983825,-15.4669070748795));
#48933=CARTESIAN_POINT('Ctrl Pts',(-5.73916807189642,38.7902613571697,-15.4697128057579));
#48934=CARTESIAN_POINT('Ctrl Pts',(-5.73163991938189,38.7925961353347,-15.4725015377136));
#48935=CARTESIAN_POINT('Ctrl Pts',(-5.72803537708487,38.7937140466196,-15.4738368058646));
#48936=CARTESIAN_POINT('Ctrl Pts',(-5.72443685547801,38.7948465963981,-15.4751684118958));
#48937=CARTESIAN_POINT('Ctrl Pts',(-5.72084482266767,38.7959936038935,-15.4764961982283));
#48938=CARTESIAN_POINT('Ctrl Pts',(-5.68106174251764,38.8086971323785,-15.4912019186035));
#48939=CARTESIAN_POINT('Ctrl Pts',(-5.64200959372428,38.8231914289868,-15.5054631835893));
#48940=CARTESIAN_POINT('Ctrl Pts',(-5.60367895309638,38.8394402713874,-15.5193035343287));
#48941=CARTESIAN_POINT('Ctrl Pts',(-5.59925348853597,38.8413162816762,-15.5209014721846));
#48942=CARTESIAN_POINT('Ctrl Pts',(-5.59483764214321,38.8432156804498,-15.5224937978581));
#48943=CARTESIAN_POINT('Ctrl Pts',(-5.59043142565676,38.8451384787602,-15.5240805366705));
#48944=CARTESIAN_POINT('Ctrl Pts',(-5.55305205649131,38.8614502029107,-15.5375413586752));
#48945=CARTESIAN_POINT('Ctrl Pts',(-5.51636486426997,38.87944394213,-15.5506004482821));
#48946=CARTESIAN_POINT('Ctrl Pts',(-5.48037827656239,38.8991259320294,-15.5632725975544));
#48947=CARTESIAN_POINT('Ctrl Pts',(-5.47538091537747,38.9018591173251,-15.5650323450308));
#48948=CARTESIAN_POINT('Ctrl Pts',(-5.47039706155543,38.9046248491444,-15.5667846303121));
#48949=CARTESIAN_POINT('Ctrl Pts',(-5.46542678317876,38.9074232578379,-15.5685294762621));
#48950=CARTESIAN_POINT('Ctrl Pts',(-5.43021578892617,38.927248053344,-15.580890506382));
#48951=CARTESIAN_POINT('Ctrl Pts',(-5.39568522742716,38.9487106524382,-15.592878507899));
#48952=CARTESIAN_POINT('Ctrl Pts',(-5.36185996218247,38.9718552620562,-15.6045012014465));
#48953=CARTESIAN_POINT('Ctrl Pts',(-5.35652757041948,38.9755038993926,-15.606333463659));
#48954=CARTESIAN_POINT('Ctrl Pts',(-5.35121274451998,38.9791944311442,-15.6081566340073));
#48955=CARTESIAN_POINT('Ctrl Pts',(-5.34591562608015,38.9829271390391,-15.6099707276299));
#48956=CARTESIAN_POINT('Ctrl Pts',(-5.34160108750772,38.985967454708,-15.6114483190785));
#48957=CARTESIAN_POINT('Ctrl Pts',(-5.33729719551838,38.9890365160764,-15.612920265461));
#48958=CARTESIAN_POINT('Ctrl Pts',(-5.33300532281936,38.9921335685879,-15.6143861303216));
#48959=CARTESIAN_POINT('Ctrl Pts',(-5.32762362465907,38.9960170485912,-15.6162242189084));
#48960=CARTESIAN_POINT('Ctrl Pts',(-5.32226600824693,38.9999409310175,-15.6180509684498));
#48961=CARTESIAN_POINT('Ctrl Pts',(-5.31694034680845,39.0038991173282,-15.6198638033924));
#48962=CARTESIAN_POINT('Ctrl Pts',(-5.31279156023976,39.0069826160432,-15.6212760345955));
#48963=CARTESIAN_POINT('Ctrl Pts',(-5.30866045530928,39.0100882064183,-15.6226804043607));
#48964=CARTESIAN_POINT('Ctrl Pts',(-5.30454965428839,39.0132138538924,-15.6240760675692));
#48965=CARTESIAN_POINT('Ctrl Pts',(-5.29917525738694,39.017300276469,-15.6259007357993));
#48966=CARTESIAN_POINT('Ctrl Pts',(-5.29383249930033,39.0214231565641,-15.6277115711503));
#48967=CARTESIAN_POINT('Ctrl Pts',(-5.28852147331464,39.0255821615688,-15.6295086519552));
#48968=CARTESIAN_POINT('Ctrl Pts',(-5.27523819943273,39.0359841446702,-15.634003285682));
#48969=CARTESIAN_POINT('Ctrl Pts',(-5.26215435627483,39.0466112362339,-15.6384115654574));
#48970=CARTESIAN_POINT('Ctrl Pts',(-5.24926792632382,39.0574606587315,-15.6427358936241));
#48971=CARTESIAN_POINT('Ctrl Pts',(-5.24396771194819,39.0619230478733,-15.6445144984356));
#48972=CARTESIAN_POINT('Ctrl Pts',(-5.23870084062666,39.0664229819347,-15.6462789219801));
#48973=CARTESIAN_POINT('Ctrl Pts',(-5.23346726793452,39.0709603894454,-15.6480292907943));
#48974=CARTESIAN_POINT('Ctrl Pts',(-5.20292155523454,39.0974429386287,-15.6582453069006));
#48975=CARTESIAN_POINT('Ctrl Pts',(-5.17350952617169,39.1252011529477,-15.6679828099636));
#48976=CARTESIAN_POINT('Ctrl Pts',(-5.14522556958604,39.1542216236436,-15.677265508949));
#48977=CARTESIAN_POINT('Ctrl Pts',(-5.14025296855357,39.159323711186,-15.6788974998064));
#48978=CARTESIAN_POINT('Ctrl Pts',(-5.13531522996645,39.164464805851,-15.6805154313045));
#48979=CARTESIAN_POINT('Ctrl Pts',(-5.13041246516379,39.1696450090146,-15.6821193766617));
#48980=CARTESIAN_POINT('Ctrl Pts',(-5.10245967567077,39.1991795949864,-15.6912641651092));
#48981=CARTESIAN_POINT('Ctrl Pts',(-5.0756420302649,39.2299833688396,-15.6999549216315));
#48982=CARTESIAN_POINT('Ctrl Pts',(-5.04998073674471,39.262072774733,-15.7082046892224));
#48983=CARTESIAN_POINT('Ctrl Pts',(-5.04554053096291,39.2676252448558,-15.709632156849));
#48984=CARTESIAN_POINT('Ctrl Pts',(-5.04113500250986,39.2732162744901,-15.7110463994174));
#48985=CARTESIAN_POINT('Ctrl Pts',(-5.03676437235535,39.2788460836699,-15.7124474439407));
#48986=CARTESIAN_POINT('Ctrl Pts',(-5.02935691609034,39.2883876288946,-15.7148219701908));
#48987=CARTESIAN_POINT('Ctrl Pts',(-5.02204963581774,39.2980404584332,-15.717158607631));
#48988=CARTESIAN_POINT('Ctrl Pts',(-5.01484358250578,39.3078055673202,-15.7194574924501));
#48989=CARTESIAN_POINT('Ctrl Pts',(-5.01179639128175,39.3119348948194,-15.7204296114926));
#48990=CARTESIAN_POINT('Ctrl Pts',(-5.00876656817256,39.3160853177002,-15.7213952133697));
#48991=CARTESIAN_POINT('Ctrl Pts',(-5.00575492521623,39.3202559331036,-15.7223540740142));
#48992=CARTESIAN_POINT('Ctrl Pts',(-5.00164458005159,39.3259480649749,-15.7236627444879));
#48993=CARTESIAN_POINT('Ctrl Pts',(-4.99757075494386,39.3316744395192,-15.7249580073045));
#48994=CARTESIAN_POINT('Ctrl Pts',(-4.99354092680169,39.3374239844029,-15.726237596301));
#48995=CARTESIAN_POINT('Ctrl Pts',(-4.99052725240488,39.3417237350618,-15.7271945265871));
#48996=CARTESIAN_POINT('Ctrl Pts',(-4.98753678343045,39.3460384288584,-15.7281431360081));
#48997=CARTESIAN_POINT('Ctrl Pts',(-4.98457197773345,39.3503644677928,-15.7290826877728));
#48998=CARTESIAN_POINT('Ctrl Pts',(-4.97763382745679,39.360488135681,-15.7312813989203));
#48999=CARTESIAN_POINT('Ctrl Pts',(-4.97082708885116,39.3706864848032,-15.733433415924));
#49000=CARTESIAN_POINT('Ctrl Pts',(-4.96415136662745,39.3809575748776,-15.7355394317834));
#49001=CARTESIAN_POINT('Ctrl Pts',(-4.9604608960052,39.3866356356039,-15.7367036787965));
#49002=CARTESIAN_POINT('Ctrl Pts',(-4.95681037613533,39.3923358701638,-15.7378539039165));
#49003=CARTESIAN_POINT('Ctrl Pts',(-4.95319982488722,39.3980580037776,-15.7389901876635));
#49004=CARTESIAN_POINT('Ctrl Pts',(-4.93060481845661,39.4338673960053,-15.7461011069683));
#49005=CARTESIAN_POINT('Ctrl Pts',(-4.90956865712636,39.4705390286067,-15.7526681103024));
#49006=CARTESIAN_POINT('Ctrl Pts',(-4.890065673627,39.5080554757784,-15.7587200529617));
#49007=CARTESIAN_POINT('Ctrl Pts',(-4.8872429986393,39.5134852469241,-15.7595959531629));
#49008=CARTESIAN_POINT('Ctrl Pts',(-4.88445243845779,39.5189327124889,-15.7604610623351));
#49009=CARTESIAN_POINT('Ctrl Pts',(-4.88169403147935,39.5243978910723,-15.7613154212793));
#49010=CARTESIAN_POINT('Ctrl Pts',(-4.86223767862383,39.5629463880009,-15.7673416201742));
#49011=CARTESIAN_POINT('Ctrl Pts',(-4.84437854675939,39.6023747382796,-15.7728337732031));
#49012=CARTESIAN_POINT('Ctrl Pts',(-4.82812990008951,39.6426872307578,-15.777805983972));
#49013=CARTESIAN_POINT('Ctrl Pts',(-4.82615816357802,39.6475790605146,-15.7784093504994));
#49014=CARTESIAN_POINT('Ctrl Pts',(-4.82421018319831,39.6524839344262,-15.7790050442279));
#49015=CARTESIAN_POINT('Ctrl Pts',(-4.82228603965509,39.6574018950085,-15.7795930685527));
#49016=CARTESIAN_POINT('Ctrl Pts',(-4.81512379702973,39.6757080276441,-15.7817818724487));
#49017=CARTESIAN_POINT('Ctrl Pts',(-4.80829157794962,39.6941953038606,-15.7838644898425));
#49018=CARTESIAN_POINT('Ctrl Pts',(-4.80179347933714,39.7128657246913,-15.785841104667));
#49019=CARTESIAN_POINT('Ctrl Pts',(-4.8002256680114,39.7173703804345,-15.7863180071109));
#49020=CARTESIAN_POINT('Ctrl Pts',(-4.7986773156128,39.721885702968,-15.7867887354881));
#49021=CARTESIAN_POINT('Ctrl Pts',(-4.79714850220147,39.7264117342425,-15.7872532840548));
#49022=CARTESIAN_POINT('Ctrl Pts',(-4.79465045226035,39.7338071770577,-15.7880123469405));
#49023=CARTESIAN_POINT('Ctrl Pts',(-4.7922042856598,39.7412320052383,-15.7887549965822));
#49024=CARTESIAN_POINT('Ctrl Pts',(-4.78981048689747,39.7486860660883,-15.7894811662577));
#49025=CARTESIAN_POINT('Ctrl Pts',(-4.78843576777426,39.7529668102166,-15.789898193518));
#49026=CARTESIAN_POINT('Ctrl Pts',(-4.78707968180564,39.7572530601147,-15.7903093722902));
#49027=CARTESIAN_POINT('Ctrl Pts',(-4.78574260519565,39.7615433383508,-15.7907146044043));
#49028=CARTESIAN_POINT('Ctrl Pts',(-4.78332253508594,39.7693086182488,-15.7914480628461));
#49029=CARTESIAN_POINT('Ctrl Pts',(-4.78096487665038,39.777086869378,-15.7921619986678));
#49030=CARTESIAN_POINT('Ctrl Pts',(-4.77867094065993,39.7848722502327,-15.7928561077752));
#49031=CARTESIAN_POINT('Ctrl Pts',(-4.77749058521369,39.7888782542063,-15.7932132648488));
#49032=CARTESIAN_POINT('Ctrl Pts',(-4.77632672235366,39.7928871971688,-15.7935652914508));
#49033=CARTESIAN_POINT('Ctrl Pts',(-4.77517921318359,39.7968994113442,-15.7939122395095));
#49034=CARTESIAN_POINT('Ctrl Pts',(-4.76246087899298,39.8413684945181,-15.7977576130129));
#49035=CARTESIAN_POINT('Ctrl Pts',(-4.7517677361539,39.8861804968818,-15.8009742178634));
#49036=CARTESIAN_POINT('Ctrl Pts',(-4.74304960963775,39.9313262331944,-15.8035907438948));
#49037=CARTESIAN_POINT('Ctrl Pts',(-4.73352637830731,39.9806411048806,-15.8064489018526));
#49038=CARTESIAN_POINT('Ctrl Pts',(-4.7263581061177,40.0303539996461,-15.8085914687166));
#49039=CARTESIAN_POINT('Ctrl Pts',(-4.72155073199278,40.0804653705169,-15.810027156372));
#49040=CARTESIAN_POINT('Ctrl Pts',(-4.71673391401152,40.130675182777,-15.811465664367));
#49041=CARTESIAN_POINT('Ctrl Pts',(-4.71428571809898,40.1812848466719,-15.8121949826116));
#49042=CARTESIAN_POINT('Ctrl Pts',(-4.71428571428571,40.2323075626015,-15.8121949837485));
#49043=CARTESIAN_POINT('',(-4.71428571428571,52.,-15.8121949837485));
#49044=CARTESIAN_POINT('',(3.94534942910196E-9,28.7540327056294,-16.5000000412986));
#49045=CARTESIAN_POINT('',(0.731312635855993,28.7467958750258,-16.4837854216996));
#49046=CARTESIAN_POINT('Origin',(0.470077120411344,40.0190250852893,-14.4549067130411));
#49047=CARTESIAN_POINT('',(0.3210340492655,44.2777094964746,-16.496876587379));
#49048=CARTESIAN_POINT('Ctrl Pts',(0.731312635812438,28.7467958754239,-16.4837854217016));
#49049=CARTESIAN_POINT('Ctrl Pts',(0.734616685498146,28.7471690084713,-16.483638835634));
#49050=CARTESIAN_POINT('Ctrl Pts',(0.737920010933865,28.7475475691393,-16.4834912865799));
#49051=CARTESIAN_POINT('Ctrl Pts',(0.741222612912324,28.7479315514833,-16.483342775688));
#49052=CARTESIAN_POINT('Ctrl Pts',(0.845120434181737,28.760011399194,-16.4786707146258));
#49053=CARTESIAN_POINT('Ctrl Pts',(0.948323680373575,28.7774576338618,-16.4730453966297));
#49054=CARTESIAN_POINT('Ctrl Pts',(1.05079165216144,28.8001000249142,-16.466506517891));
#49055=CARTESIAN_POINT('Ctrl Pts',(1.05587756435429,28.801223861082,-16.4661819661065));
#49056=CARTESIAN_POINT('Ctrl Pts',(1.06096252503882,28.8023607191809,-16.4658551046886));
#49057=CARTESIAN_POINT('Ctrl Pts',(1.06604599104648,28.8035104462793,-16.4655259757118));
#49058=CARTESIAN_POINT('Ctrl Pts',(1.07948376023311,28.8065496654563,-16.4646559474247));
#49059=CARTESIAN_POINT('Ctrl Pts',(1.09291006996102,28.8096785418744,-16.4637701472321));
#49060=CARTESIAN_POINT('Ctrl Pts',(1.10632404935655,28.8128965822484,-16.4628687224595));
#49061=CARTESIAN_POINT('Ctrl Pts',(1.11422078750616,28.8147910254588,-16.4623380585021));
#49062=CARTESIAN_POINT('Ctrl Pts',(1.12211200562617,28.8167160726008,-16.4618020600035));
#49063=CARTESIAN_POINT('Ctrl Pts',(1.12999383075715,28.818670716019,-16.4612610070569));
#49064=CARTESIAN_POINT('Ctrl Pts',(1.13550065267297,28.8200363734694,-16.4608829877308));
#49065=CARTESIAN_POINT('Ctrl Pts',(1.1410004192206,28.8214158328344,-16.4605026765839));
#49066=CARTESIAN_POINT('Ctrl Pts',(1.14649254658236,28.8228088410152,-16.4601201352088));
#49067=CARTESIAN_POINT('Ctrl Pts',(1.16726650596732,28.8280778913238,-16.4586731733185));
#49068=CARTESIAN_POINT('Ctrl Pts',(1.18794518936591,28.833544327345,-16.4571933294199));
#49069=CARTESIAN_POINT('Ctrl Pts',(1.20853084392565,28.8392035794322,-16.4556814869297));
#49070=CARTESIAN_POINT('Ctrl Pts',(1.21440895604015,28.8408195454514,-16.455249789233));
#49071=CARTESIAN_POINT('Ctrl Pts',(1.22027948624603,28.8424512259965,-16.4548154834927));
#49072=CARTESIAN_POINT('Ctrl Pts',(1.22614248193765,28.8440985249416,-16.4543785888375));
#49073=CARTESIAN_POINT('Ctrl Pts',(1.27220783047617,28.8570412941407,-16.4509459230761));
#49074=CARTESIAN_POINT('Ctrl Pts',(1.3178082038286,28.8709478913296,-16.447353427901));
#49075=CARTESIAN_POINT('Ctrl Pts',(1.36296608480579,28.8857718606986,-16.4436104141296));
#49076=CARTESIAN_POINT('Ctrl Pts',(1.36955965797723,28.8879363317634,-16.4430638908064));
#49077=CARTESIAN_POINT('Ctrl Pts',(1.37614381062977,28.8901203327012,-16.4425141624419));
#49078=CARTESIAN_POINT('Ctrl Pts',(1.38271860044915,28.892323744337,-16.4419612544658));
#49079=CARTESIAN_POINT('Ctrl Pts',(1.47768180782263,28.9241487975866,-16.4339753087194));
#49080=CARTESIAN_POINT('Ctrl Pts',(1.57069371812965,28.9600199707892,-16.4253258894182));
#49081=CARTESIAN_POINT('Ctrl Pts',(1.6619297639424,28.9995770867733,-16.4160893473363));
#49082=CARTESIAN_POINT('Ctrl Pts',(1.66985101459179,29.0030114950478,-16.4152874168678));
#49083=CARTESIAN_POINT('Ctrl Pts',(1.6777588721055,29.0064737005077,-16.414481058856));
#49084=CARTESIAN_POINT('Ctrl Pts',(1.68565342634818,29.0099635189963,-16.4136703161511));
#49085=CARTESIAN_POINT('Ctrl Pts',(1.77500332989141,29.0494609922869,-16.4044943981371));
#49086=CARTESIAN_POINT('Ctrl Pts',(1.86265046663758,29.0924930099575,-16.3947566911446));
#49087=CARTESIAN_POINT('Ctrl Pts',(1.94872552747264,29.1387927117366,-16.3845191817942));
#49088=CARTESIAN_POINT('Ctrl Pts',(1.9578515268182,29.1437015789977,-16.383433762827));
#49089=CARTESIAN_POINT('Ctrl Pts',(1.96695984784121,29.1486471906051,-16.3823427237235));
#49090=CARTESIAN_POINT('Ctrl Pts',(1.9760506137378,29.1536292958558,-16.3812461293587));
#49091=CARTESIAN_POINT('Ctrl Pts',(2.06029660563837,29.1997994869451,-16.3710837644901));
#49092=CARTESIAN_POINT('Ctrl Pts',(2.1430359410388,29.2491015209459,-16.3604441914389));
#49093=CARTESIAN_POINT('Ctrl Pts',(2.22436702801141,29.301335893347,-16.3493789277972));
#49094=CARTESIAN_POINT('Ctrl Pts',(2.23458821889496,29.3079003880669,-16.347988313506));
#49095=CARTESIAN_POINT('Ctrl Pts',(2.24478716184637,29.3145112072703,-16.3465909740617));
#49096=CARTESIAN_POINT('Ctrl Pts',(2.25496401208747,29.3211680380968,-16.3451870012336));
#49097=CARTESIAN_POINT('Ctrl Pts',(2.27775279060625,29.336074520923,-16.3420431182963));
#49098=CARTESIAN_POINT('Ctrl Pts',(2.30043071534413,29.3512118385305,-16.338865983534));
#49099=CARTESIAN_POINT('Ctrl Pts',(2.32299970540114,29.3665761205162,-16.3356566023839));
#49100=CARTESIAN_POINT('Ctrl Pts',(2.34556869545816,29.3819404025018,-16.3324472212339));
#49101=CARTESIAN_POINT('Ctrl Pts',(2.36804092323506,29.3975404318301,-16.329203784601));
#49102=CARTESIAN_POINT('Ctrl Pts',(2.39036258748978,29.4133328398107,-16.3259355337187));
#49103=CARTESIAN_POINT('Ctrl Pts',(2.41268425174452,29.4291252477914,-16.3226672828364));
#49104=CARTESIAN_POINT('Ctrl Pts',(2.43486066092521,29.4451132785474,-16.3193735215193));
#49105=CARTESIAN_POINT('Ctrl Pts',(2.45689550418518,29.4612920769389,-16.3160554493108));
#49106=CARTESIAN_POINT('Ctrl Pts',(2.4678508029967,29.4693358632594,-16.3144057678453));
#49107=CARTESIAN_POINT('Ctrl Pts',(2.47877011604896,29.477426086673,-16.3127502284335));
#49108=CARTESIAN_POINT('Ctrl Pts',(2.4896578027103,29.4855650408066,-16.311088376482));
#49109=CARTESIAN_POINT('Ctrl Pts',(2.50066896820931,29.4937963000026,-16.3094076772258));
#49110=CARTESIAN_POINT('Ctrl Pts',(2.51163612628462,29.5020688330178,-16.3077222797715));
#49111=CARTESIAN_POINT('Ctrl Pts',(2.52256015072484,29.5103819452868,-16.3060323219646));
#49112=CARTESIAN_POINT('Ctrl Pts',(2.53317374658008,29.5184588234012,-16.3043903877787));
#49113=CARTESIAN_POINT('Ctrl Pts',(2.54374758129008,29.5265747525576,-16.3027439980989));
#49114=CARTESIAN_POINT('Ctrl Pts',(2.55427857869813,29.5347263140629,-16.3010938572356));
#49115=CARTESIAN_POINT('Ctrl Pts',(2.57566004008263,29.5512767214742,-16.2977435171128));
#49116=CARTESIAN_POINT('Ctrl Pts',(2.59687480044613,29.5679813972322,-16.2943762062056));
#49117=CARTESIAN_POINT('Ctrl Pts',(2.61792789046617,29.5848353002105,-16.2909930194669));
#49118=CARTESIAN_POINT('Ctrl Pts',(2.66006203009866,29.6185654890218,-16.2842221529425));
#49119=CARTESIAN_POINT('Ctrl Pts',(2.70154891715646,29.6528931031441,-16.2773877442513));
#49120=CARTESIAN_POINT('Ctrl Pts',(2.74242506837524,29.687781395081,-16.2704979869811));
#49121=CARTESIAN_POINT('Ctrl Pts',(2.75343149573759,29.6971755146239,-16.2686428315744));
#49122=CARTESIAN_POINT('Ctrl Pts',(2.76439370647325,29.7066102235636,-16.2667836725572));
#49123=CARTESIAN_POINT('Ctrl Pts',(2.77531229191419,29.7160849216131,-16.2649206515303));
#49124=CARTESIAN_POINT('Ctrl Pts',(2.8456018154237,29.7770792706431,-16.2529272609048));
#49125=CARTESIAN_POINT('Ctrl Pts',(2.91408883144597,29.8397324669013,-16.2407729461803));
#49126=CARTESIAN_POINT('Ctrl Pts',(2.98093811843778,29.9038965360028,-16.2284937050254));
#49127=CARTESIAN_POINT('Ctrl Pts',(2.99179906065064,29.9143212133332,-16.2264987080015));
#49128=CARTESIAN_POINT('Ctrl Pts',(3.00261674765443,29.9247857948943,-16.2245004096329));
#49129=CARTESIAN_POINT('Ctrl Pts',(3.01339173931629,29.9352897861473,-16.22249894315));
#49130=CARTESIAN_POINT('Ctrl Pts',(3.07936347969847,29.9996022798977,-16.2102446202386));
#49131=CARTESIAN_POINT('Ctrl Pts',(3.14373670241214,30.0653901737341,-16.1978712029431));
#49132=CARTESIAN_POINT('Ctrl Pts',(3.20663867175698,30.1325397322854,-16.1854091214524));
#49133=CARTESIAN_POINT('Ctrl Pts',(3.21724458806279,30.1438618356374,-16.1833078868701));
#49134=CARTESIAN_POINT('Ctrl Pts',(3.22780865912799,30.1552226669215,-16.1812041287764));
#49135=CARTESIAN_POINT('Ctrl Pts',(3.23833137423545,30.1666217964529,-16.179097976329));
#49136=CARTESIAN_POINT('Ctrl Pts',(3.30051780922609,30.2339876065426,-16.1666511780536));
#49137=CARTESIAN_POINT('Ctrl Pts',(3.36126109250365,30.3026896174408,-16.1541205481176));
#49138=CARTESIAN_POINT('Ctrl Pts',(3.42066110077687,30.3726394183252,-16.1415326915899));
#49139=CARTESIAN_POINT('Ctrl Pts',(3.43092444856263,30.3847255973492,-16.1393577163133));
#49140=CARTESIAN_POINT('Ctrl Pts',(3.44114781103686,30.3968489132885,-16.1371810457367));
#49141=CARTESIAN_POINT('Ctrl Pts',(3.45133156533654,30.4090090427529,-16.1350027997543));
#49142=CARTESIAN_POINT('Ctrl Pts',(3.52045467376127,30.491546967637,-16.1202177677526));
#49143=CARTESIAN_POINT('Ctrl Pts',(3.58775143477868,30.5757822736924,-16.105360573047));
#49144=CARTESIAN_POINT('Ctrl Pts',(3.65334819678238,30.6616030099696,-16.0904663944269));
#49145=CARTESIAN_POINT('Ctrl Pts',(3.70914483972207,30.7346021768891,-16.0777973976509));
#49146=CARTESIAN_POINT('Ctrl Pts',(3.76371063983931,30.8087513309492,-16.0651017701954));
#49147=CARTESIAN_POINT('Ctrl Pts',(3.81710946620164,30.8839857712926,-16.0524040356279));
#49148=CARTESIAN_POINT('Ctrl Pts',(3.82648843290392,30.8971999439423,-16.0501738062799));
#49149=CARTESIAN_POINT('Ctrl Pts',(3.83583337260282,30.9104510140065,-16.0479429610118));
#49150=CARTESIAN_POINT('Ctrl Pts',(3.84514079754373,30.9237330962212,-16.0457125481931));
#49151=CARTESIAN_POINT('Ctrl Pts',(3.86071553022625,30.9459588870576,-16.0419802502007));
#49152=CARTESIAN_POINT('Ctrl Pts',(3.87619388529158,30.9682835953682,-16.0382470688338));
#49153=CARTESIAN_POINT('Ctrl Pts',(3.89154316500324,30.9906557222109,-16.0345218565835));
#49154=CARTESIAN_POINT('Ctrl Pts',(3.89773456957979,30.9996799169043,-16.0330192260622));
#49155=CARTESIAN_POINT('Ctrl Pts',(3.90390673158024,31.0087143633717,-16.0315174679896));
#49156=CARTESIAN_POINT('Ctrl Pts',(3.91005845705946,31.0177570719153,-16.0300169326915));
#49157=CARTESIAN_POINT('Ctrl Pts',(3.91915764176106,31.0311323884047,-16.0277974500644));
#49158=CARTESIAN_POINT('Ctrl Pts',(3.92821432019911,31.044528753913,-16.0255801318543));
#49159=CARTESIAN_POINT('Ctrl Pts',(3.93722860915545,31.0579453074097,-16.0233651619476));
#49160=CARTESIAN_POINT('Ctrl Pts',(3.95846129759498,31.0895473008347,-16.0181479156225));
#49161=CARTESIAN_POINT('Ctrl Pts',(3.97945901013079,31.1212615902012,-16.012943649059));
#49162=CARTESIAN_POINT('Ctrl Pts',(4.00022876823323,31.1530850595607,-16.0077534276925));
#49163=CARTESIAN_POINT('Ctrl Pts',(4.00901742940061,31.166551065664,-16.005557201008));
#49164=CARTESIAN_POINT('Ctrl Pts',(4.01776531294456,31.1800366018781,-16.0033634911397));
#49165=CARTESIAN_POINT('Ctrl Pts',(4.02647287172629,31.1935414708459,-16.0011723745607));
#49166=CARTESIAN_POINT('Ctrl Pts',(4.07643282159421,31.2710261704631,-15.9886007598075));
#49167=CARTESIAN_POINT('Ctrl Pts',(4.12506630677904,31.3491467663653,-15.9761142740004));
#49168=CARTESIAN_POINT('Ctrl Pts',(4.1724572629542,31.4278654560049,-15.963727647039));
#49169=CARTESIAN_POINT('Ctrl Pts',(4.18062581228057,31.4414338148464,-15.96159262421));
#49170=CARTESIAN_POINT('Ctrl Pts',(4.18875754981286,31.4550198912338,-15.9594605716859));
#49171=CARTESIAN_POINT('Ctrl Pts',(4.19685278850281,31.4686235486063,-15.9573315597597));
#49172=CARTESIAN_POINT('Ctrl Pts',(4.2519136616836,31.5611506848738,-15.9428507939464));
#49173=CARTESIAN_POINT('Ctrl Pts',(4.30528494322195,31.6544921398643,-15.9285110242643));
#49174=CARTESIAN_POINT('Ctrl Pts',(4.3570738298972,31.7486000042021,-15.9143317969289));
#49175=CARTESIAN_POINT('Ctrl Pts',(4.40154566221242,31.8294117271614,-15.9021558985673));
#49176=CARTESIAN_POINT('Ctrl Pts',(4.44484660746696,31.9107908818802,-15.890099467165));
#49177=CARTESIAN_POINT('Ctrl Pts',(4.48703986256301,31.9927091048758,-15.8781760058382));
#49178=CARTESIAN_POINT('Ctrl Pts',(4.54311742712378,32.101583720695,-15.8623289546729));
#49179=CARTESIAN_POINT('Ctrl Pts',(4.59723619017192,32.2114115949789,-15.8467165556072));
#49180=CARTESIAN_POINT('Ctrl Pts',(4.64949281461725,32.3221519839062,-15.8313691559524));
#49181=CARTESIAN_POINT('Ctrl Pts',(4.68921103260749,32.4063214256646,-15.8197041972693));
#49182=CARTESIAN_POINT('Ctrl Pts',(4.72785240054499,32.4910185880583,-15.8081926424038));
#49183=CARTESIAN_POINT('Ctrl Pts',(4.76545874007257,32.5762252746749,-15.7968478816819));
#49184=CARTESIAN_POINT('Ctrl Pts',(4.8145581895929,32.6874725127972,-15.7820359772696));
#49185=CARTESIAN_POINT('Ctrl Pts',(4.86189217437588,32.7995888343388,-15.767508226408));
#49186=CARTESIAN_POINT('Ctrl Pts',(4.90751726593677,32.9125521688301,-15.7532948069065));
#49187=CARTESIAN_POINT('Ctrl Pts',(4.94292643975522,33.000221874452,-15.7422639152531));
#49188=CARTESIAN_POINT('Ctrl Pts',(4.97730545013789,33.0884022086102,-15.7314226152448));
#49189=CARTESIAN_POINT('Ctrl Pts',(5.01068036844344,33.1770825485621,-15.7207850390979));
#49190=CARTESIAN_POINT('Ctrl Pts',(5.05324703184162,33.2901862315797,-15.7072177812226));
#49191=CARTESIAN_POINT('Ctrl Pts',(5.09417985157194,33.4041034930525,-15.6939817639376));
#49192=CARTESIAN_POINT('Ctrl Pts',(5.1335045001183,33.5188268327618,-15.6811080106665));
#49193=CARTESIAN_POINT('Ctrl Pts',(5.16483497343243,33.6102284514955,-15.6708513192981));
#49194=CARTESIAN_POINT('Ctrl Pts',(5.19514785591287,33.7021488152071,-15.66082350329));
#49195=CARTESIAN_POINT('Ctrl Pts',(5.2244462630085,33.7945633654866,-15.6510434554676));
#49196=CARTESIAN_POINT('Ctrl Pts',(5.22795148832419,33.8056197283844,-15.6498733825997));
#49197=CARTESIAN_POINT('Ctrl Pts',(5.23144245196559,33.8166841411844,-15.6487067609901));
#49198=CARTESIAN_POINT('Ctrl Pts',(5.2349189486445,33.8277559098327,-15.6475436910747));
#49199=CARTESIAN_POINT('Ctrl Pts',(5.2446746186188,33.8588252681381,-15.6442799093716));
#49200=CARTESIAN_POINT('Ctrl Pts',(5.25431701128392,33.8899539217391,-15.6410438820536));
#49201=CARTESIAN_POINT('Ctrl Pts',(5.2638444202153,33.9211357782144,-15.6378368672982));
#49202=CARTESIAN_POINT('Ctrl Pts',(5.26693462334182,33.9312495742175,-15.6367966760883));
#49203=CARTESIAN_POINT('Ctrl Pts',(5.27001255653563,33.9413684091124,-15.6357595952178));
#49204=CARTESIAN_POINT('Ctrl Pts',(5.27307794881816,33.9514913720823,-15.6347257393818));
#49205=CARTESIAN_POINT('Ctrl Pts',(5.27632085614409,33.9622005498154,-15.6336320135694));
#49206=CARTESIAN_POINT('Ctrl Pts',(5.27954900617633,33.9729119185877,-15.6325421418139));
#49207=CARTESIAN_POINT('Ctrl Pts',(5.28276229076912,33.9836249799428,-15.631456189949));
#49208=CARTESIAN_POINT('Ctrl Pts',(5.2952909009369,34.0253952513105,-15.6272220590513));
#49209=CARTESIAN_POINT('Ctrl Pts',(5.30759740664544,34.0672041752914,-15.6230462074124));
#49210=CARTESIAN_POINT('Ctrl Pts',(5.31968392036379,34.1090516118263,-15.6189296364195));
#49211=CARTESIAN_POINT('Ctrl Pts',(5.32266165147491,34.1193614841844,-15.6179154447508));
#49212=CARTESIAN_POINT('Ctrl Pts',(5.3256260357014,34.1296736930948,-15.6169048508008));
#49213=CARTESIAN_POINT('Ctrl Pts',(5.32857709711616,34.1399882377568,-15.6158978700675));
#49214=CARTESIAN_POINT('Ctrl Pts',(5.35573331102589,34.2349045888094,-15.6066314467867));
#49215=CARTESIAN_POINT('Ctrl Pts',(5.38176097528874,34.330018513957,-15.5976711212928));
#49216=CARTESIAN_POINT('Ctrl Pts',(5.40667913038459,34.4253275758219,-15.5890288594613));
#49217=CARTESIAN_POINT('Ctrl Pts',(5.43655671445108,34.5396058800228,-15.5786665391611));
#49218=CARTESIAN_POINT('Ctrl Pts',(5.4648418408843,34.6541642591764,-15.5687612237176));
#49219=CARTESIAN_POINT('Ctrl Pts',(5.49154896429295,34.7690018144804,-15.5593350786686));
#49220=CARTESIAN_POINT('Ctrl Pts',(5.51425047771342,34.8666157080854,-15.5513226935436));
#49221=CARTESIAN_POINT('Ctrl Pts',(5.53581096326103,34.9644314725277,-15.5436568302854));
#49222=CARTESIAN_POINT('Ctrl Pts',(5.55623902970539,35.0624484180682,-15.5363511753867));
#49223=CARTESIAN_POINT('Ctrl Pts',(5.57988683156696,35.1759141400214,-15.527894051949));
#49224=CARTESIAN_POINT('Ctrl Pts',(5.60201700179433,35.2896494727898,-15.5199195687207));
#49225=CARTESIAN_POINT('Ctrl Pts',(5.62262129551896,35.403657194424,-15.5124513197386));
#49226=CARTESIAN_POINT('Ctrl Pts',(5.64077602836221,35.5041110006062,-15.5058709405764));
#49227=CARTESIAN_POINT('Ctrl Pts',(5.65774561136324,35.6047763774753,-15.4996837693532));
#49228=CARTESIAN_POINT('Ctrl Pts',(5.67352437393353,35.7056550526876,-15.4939059368047));
#49229=CARTESIAN_POINT('Ctrl Pts',(5.69112288890293,35.8181679869503,-15.4874617513281));
#49230=CARTESIAN_POINT('Ctrl Pts',(5.70724024386807,35.9309462212848,-15.4815266881963));
#49231=CARTESIAN_POINT('Ctrl Pts',(5.72184788894286,36.0439958608173,-15.476125906358));
#49232=CARTESIAN_POINT('Ctrl Pts',(5.73521687343338,36.1474594149925,-15.4711830857827));
#49233=CARTESIAN_POINT('Ctrl Pts',(5.74732086117479,36.2511503898043,-15.4666879504269));
#49234=CARTESIAN_POINT('Ctrl Pts',(5.75813800618103,36.3550732611076,-15.4626597551001));
#49235=CARTESIAN_POINT('Ctrl Pts',(5.76973743980501,36.4665117642431,-15.4583402434091));
#49236=CARTESIAN_POINT('Ctrl Pts',(5.77985764006083,36.5782168324163,-15.4545575498512));
#49237=CARTESIAN_POINT('Ctrl Pts',(5.78844979037594,36.6901979213228,-15.4513387051517));
#49238=CARTESIAN_POINT('Ctrl Pts',(5.79663487698932,36.7968737682468,-15.4482723571836));
#49239=CARTESIAN_POINT('Ctrl Pts',(5.80343362974005,36.9038002277388,-15.4457175623473));
#49240=CARTESIAN_POINT('Ctrl Pts',(5.8088031368251,37.0109851036483,-15.4436979418038));
#49241=CARTESIAN_POINT('Ctrl Pts',(5.81430863978894,37.1208846982762,-15.4416271694383));
#49242=CARTESIAN_POINT('Ctrl Pts',(5.81830887505587,37.2310564494967,-15.4401194484732));
#49243=CARTESIAN_POINT('Ctrl Pts',(5.82073968029914,37.3415118986157,-15.4392030096826));
#49244=CARTESIAN_POINT('Ctrl Pts',(5.82074760164734,37.3418718435659,-15.4392000232522));
#49245=CARTESIAN_POINT('Ctrl Pts',(5.82075550629764,37.3422317922858,-15.4391970431108));
#49246=CARTESIAN_POINT('Ctrl Pts',(5.82076339424765,37.3425917447223,-15.4391940692593));
#49247=CARTESIAN_POINT('Ctrl Pts',(5.8213620453315,37.3699101121222,-15.4389683706475));
#49248=CARTESIAN_POINT('Ctrl Pts',(5.82186461765603,37.3972541851766,-15.4387788590838));
#49249=CARTESIAN_POINT('Ctrl Pts',(5.82226993685469,37.4245958984253,-15.4386260036546));
#49250=CARTESIAN_POINT('Ctrl Pts',(5.82267525605335,37.4519376116741,-15.4384731482255));
#49251=CARTESIAN_POINT('Ctrl Pts',(5.82298322987151,37.4792662650347,-15.4383569837344));
#49252=CARTESIAN_POINT('Ctrl Pts',(5.82319306158449,37.5065817823569,-15.4382778368426));
#49253=CARTESIAN_POINT('Ctrl Pts',(5.82319492313034,37.5068241150683,-15.4382771346819));
#49254=CARTESIAN_POINT('Ctrl Pts',(5.82319677694153,37.5070664459699,-15.4382764354387));
#49255=CARTESIAN_POINT('Ctrl Pts',(5.82319862301729,37.5073087750453,-15.4382757391131));
#49256=CARTESIAN_POINT('Ctrl Pts',(5.82361295281936,37.5616966609361,-15.4381194571051));
#49257=CARTESIAN_POINT('Ctrl Pts',(5.82363882494282,37.6160331651307,-15.4381096966784));
#49258=CARTESIAN_POINT('Ctrl Pts',(5.82327195590684,37.6703166990449,-15.4382480783256));
#49259=CARTESIAN_POINT('Ctrl Pts',(5.82326629494549,37.6711543194408,-15.4382502136194));
#49260=CARTESIAN_POINT('Ctrl Pts',(5.8232605403331,37.6719919272872,-15.4382523842383));
#49261=CARTESIAN_POINT('Ctrl Pts',(5.8232546920561,37.6728295225823,-15.4382545901876));
#49262=CARTESIAN_POINT('Ctrl Pts',(5.82249914619176,37.781039455463,-15.4385395793989));
#49263=CARTESIAN_POINT('Ctrl Pts',(5.82018359012415,37.8890402606468,-15.4394141505793));
#49264=CARTESIAN_POINT('Ctrl Pts',(5.8162661747651,37.9968265190168,-15.4408897890572));
#49265=CARTESIAN_POINT('Ctrl Pts',(5.81220429168145,38.1085877542688,-15.4424198466134));
#49266=CARTESIAN_POINT('Ctrl Pts',(5.8064178675135,38.220117964245,-15.4445970100905));
#49267=CARTESIAN_POINT('Ctrl Pts',(5.79885506465812,38.3314104977014,-15.4474360312433));
#49268=CARTESIAN_POINT('Ctrl Pts',(5.79171731437334,38.4364480515768,-15.4501154907544));
#49269=CARTESIAN_POINT('Ctrl Pts',(5.78299784892559,38.541273967809,-15.4533845335069));
#49270=CARTESIAN_POINT('Ctrl Pts',(5.77263170026572,38.6458799562132,-15.4572559204152));
#49271=CARTESIAN_POINT('Ctrl Pts',(5.76143267394023,38.7588906081323,-15.4614383574343));
#49272=CARTESIAN_POINT('Ctrl Pts',(5.74831194401947,38.8716445920318,-15.4663237377932));
#49273=CARTESIAN_POINT('Ctrl Pts',(5.73318723260849,38.9841316418235,-15.4719282623814));
#49274=CARTESIAN_POINT('Ctrl Pts',(5.71947849532972,39.0860876640547,-15.4770080918779));
#49275=CARTESIAN_POINT('Ctrl Pts',(5.70412446117446,39.1878245192004,-15.4826787537311));
#49276=CARTESIAN_POINT('Ctrl Pts',(5.68703815784452,39.2893313225491,-15.4889524181855));
#49277=CARTESIAN_POINT('Ctrl Pts',(5.669069433215,39.3960804397909,-15.4955500857337));
#49278=CARTESIAN_POINT('Ctrl Pts',(5.64918879223543,39.5025757189157,-15.5028132260879));
#49279=CARTESIAN_POINT('Ctrl Pts',(5.62728826714314,39.6088036853509,-15.5107584481952));
#49280=CARTESIAN_POINT('Ctrl Pts',(5.62579498641333,39.6160468073572,-15.5113001907798));
#49281=CARTESIAN_POINT('Ctrl Pts',(5.62429232542101,39.6232886887372,-15.5118451005988));
#49282=CARTESIAN_POINT('Ctrl Pts',(5.62278025233869,39.6305293255435,-15.5123931820307));
#49283=CARTESIAN_POINT('Ctrl Pts',(5.60211619080702,39.7294802071136,-15.5198832885376));
#49284=CARTESIAN_POINT('Ctrl Pts',(5.57969076442153,39.8281981964826,-15.5279657157206));
#49285=CARTESIAN_POINT('Ctrl Pts',(5.5553990454623,39.9266703282958,-15.5366515625495));
#49286=CARTESIAN_POINT('Ctrl Pts',(5.55338471517728,39.9348358845363,-15.5373718147617));
#49287=CARTESIAN_POINT('Ctrl Pts',(5.55135754681633,39.9429997503324,-15.5380962180081));
#49288=CARTESIAN_POINT('Ctrl Pts',(5.54931748055969,39.9511619183062,-15.5388247785975));
#49289=CARTESIAN_POINT('Ctrl Pts',(5.53815638953542,39.9958166933237,-15.5428106937748));
#49290=CARTESIAN_POINT('Ctrl Pts',(5.52660900541491,40.0404206196005,-15.5469210408861));
#49291=CARTESIAN_POINT('Ctrl Pts',(5.51466417079211,40.0849723231114,-15.551156843479));
#49292=CARTESIAN_POINT('Ctrl Pts',(5.51235605772304,40.0935810960555,-15.5519753321087));
#49293=CARTESIAN_POINT('Ctrl Pts',(5.51003293440113,40.1021885423761,-15.5527985653375));
#49294=CARTESIAN_POINT('Ctrl Pts',(5.50769484480291,40.110794174102,-15.5536265062696));
#49295=CARTESIAN_POINT('Ctrl Pts',(5.50287711171511,40.1285264443873,-15.5553325137837));
#49296=CARTESIAN_POINT('Ctrl Pts',(5.49799592481585,40.1462502263921,-15.5570584685343));
#49297=CARTESIAN_POINT('Ctrl Pts',(5.49305708097302,40.1639430592698,-15.5588021349732));
#49298=CARTESIAN_POINT('Ctrl Pts',(5.49059650190236,40.1727577972257,-15.5596708462106));
#49299=CARTESIAN_POINT('Ctrl Pts',(5.48812116123534,40.1815664747305,-15.5605441128286));
#49300=CARTESIAN_POINT('Ctrl Pts',(5.48563167606625,40.1903666381514,-15.5614216932303));
#49301=CARTESIAN_POINT('Ctrl Pts',(5.48069927406808,40.2078023490285,-15.563160438004));
#49302=CARTESIAN_POINT('Ctrl Pts',(5.47570951682564,40.225211449671,-15.56491676568));
#49303=CARTESIAN_POINT('Ctrl Pts',(5.47066250971218,40.2425923596256,-15.5666904547911));
#49304=CARTESIAN_POINT('Ctrl Pts',(5.46805116268897,40.2515853304003,-15.5676081705138));
#49305=CARTESIAN_POINT('Ctrl Pts',(5.46542444821896,40.2605708241239,-15.5685305485455));
#49306=CARTESIAN_POINT('Ctrl Pts',(5.46278232737112,40.2695488251422,-15.5694575770565));
#49307=CARTESIAN_POINT('Ctrl Pts',(5.43468911829116,40.3650103404363,-15.5793145091508));
#49308=CARTESIAN_POINT('Ctrl Pts',(5.40485794134804,40.4596263778678,-15.5896979385596));
#49309=CARTESIAN_POINT('Ctrl Pts',(5.37323020349376,40.5533733304178,-15.6005915390615));
#49310=CARTESIAN_POINT('Ctrl Pts',(5.3351536160963,40.6662351496368,-15.6137063287912));
#49311=CARTESIAN_POINT('Ctrl Pts',(5.29447121827874,40.7778361260763,-15.6275612366279));
#49312=CARTESIAN_POINT('Ctrl Pts',(5.25107269225853,40.8881316463221,-15.6421301484521));
#49313=CARTESIAN_POINT('Ctrl Pts',(5.21559399463491,40.9782992573194,-15.6540403690221));
#49314=CARTESIAN_POINT('Ctrl Pts',(5.17830112171146,41.0675948734014,-15.6664279778806));
#49315=CARTESIAN_POINT('Ctrl Pts',(5.13910957611281,41.155983365789,-15.679273903052));
#49316=CARTESIAN_POINT('Ctrl Pts',(5.09554371104179,41.254237238515,-15.6935536114479));
#49317=CARTESIAN_POINT('Ctrl Pts',(5.04963603199427,41.3513725988285,-15.7083982580537));
#49318=CARTESIAN_POINT('Ctrl Pts',(5.00126317578049,41.4473382083884,-15.7237835817552));
#49319=CARTESIAN_POINT('Ctrl Pts',(4.99592362906449,41.4579311916331,-15.7254818617634));
#49320=CARTESIAN_POINT('Ctrl Pts',(4.9905540005862,41.4685099032567,-15.7271867431753));
#49321=CARTESIAN_POINT('Ctrl Pts',(4.98515414659887,41.4790742849983,-15.7288981856539));
#49322=CARTESIAN_POINT('Ctrl Pts',(4.94163479931358,41.5642164016083,-15.7426913103871));
#49323=CARTESIAN_POINT('Ctrl Pts',(4.89615436809763,41.6484285807815,-15.7569108569489));
#49324=CARTESIAN_POINT('Ctrl Pts',(4.84860359708565,41.7316662063295,-15.771529762144));
#49325=CARTESIAN_POINT('Ctrl Pts',(4.79515275549666,41.8252319055333,-15.7879625721524));
#49326=CARTESIAN_POINT('Ctrl Pts',(4.7390875857014,41.9175670258641,-15.8048995653748));
#49327=CARTESIAN_POINT('Ctrl Pts',(4.68023107128565,42.0085977892414,-15.8223083797611));
#49328=CARTESIAN_POINT('Ctrl Pts',(4.6734321579909,42.0191133672279,-15.8243193894302));
#49329=CARTESIAN_POINT('Ctrl Pts',(4.66659499601975,42.0296129979074,-15.8263369893176));
#49330=CARTESIAN_POINT('Ctrl Pts',(4.65972037206363,42.0400950170412,-15.8283608138738));
#49331=CARTESIAN_POINT('Ctrl Pts',(4.65171701528829,42.0522980610753,-15.8307169267429));
#49332=CARTESIAN_POINT('Ctrl Pts',(4.64366667531103,42.064470958696,-15.8330802653263));
#49333=CARTESIAN_POINT('Ctrl Pts',(4.63557576166612,42.076603952368,-15.8354487521939));
#49334=CARTESIAN_POINT('Ctrl Pts',(4.62860930468073,42.08705073035,-15.8374880721778));
#49335=CARTESIAN_POINT('Ctrl Pts',(4.62161112726301,42.0974703956641,-15.8395316899087));
#49336=CARTESIAN_POINT('Ctrl Pts',(4.61458421977622,42.1078582381447,-15.8415785980626));
#49337=CARTESIAN_POINT('Ctrl Pts',(4.60643986708164,42.1198979943329,-15.8439510132352));
#49338=CARTESIAN_POINT('Ctrl Pts',(4.59825427875283,42.1318990443132,-15.8463286271726));
#49339=CARTESIAN_POINT('Ctrl Pts',(4.59002734719915,42.143861320884,-15.8487112713859));
#49340=CARTESIAN_POINT('Ctrl Pts',(4.58291897753297,42.1541971652215,-15.8507699631035));
#49341=CARTESIAN_POINT('Ctrl Pts',(4.57577995255875,42.1645037551717,-15.8528323494342));
#49342=CARTESIAN_POINT('Ctrl Pts',(4.56861020602952,42.1747810570319,-15.8548983215082));
#49343=CARTESIAN_POINT('Ctrl Pts',(4.54486512980106,42.2088178692257,-15.8617404970554));
#49344=CARTESIAN_POINT('Ctrl Pts',(4.52078312516702,42.2425334732247,-15.8686220086643));
#49345=CARTESIAN_POINT('Ctrl Pts',(4.49636147268642,42.2759263536235,-15.8755388446782));
#49346=CARTESIAN_POINT('Ctrl Pts',(4.48898761919182,42.286008972235,-15.8776273084074));
#49347=CARTESIAN_POINT('Ctrl Pts',(4.48158279691073,42.2960621611675,-15.8797189935682));
#49348=CARTESIAN_POINT('Ctrl Pts',(4.47414693197282,42.3060858788081,-15.8818137890834));
#49349=CARTESIAN_POINT('Ctrl Pts',(4.41745663849877,42.3825057034674,-15.8977843013931));
#49350=CARTESIAN_POINT('Ctrl Pts',(4.35896286596554,42.4572133051137,-15.9139357728764));
#49351=CARTESIAN_POINT('Ctrl Pts',(4.2986246258115,42.5301826611137,-15.9302174160106));
#49352=CARTESIAN_POINT('Ctrl Pts',(4.29080043326918,42.5396447582775,-15.9323286925487));
#49353=CARTESIAN_POINT('Ctrl Pts',(4.28294516445785,42.5490775657595,-15.9344421737816));
#49354=CARTESIAN_POINT('Ctrl Pts',(4.27505873967226,42.5584810363298,-15.9365577453965));
#49355=CARTESIAN_POINT('Ctrl Pts',(4.21414970207225,42.6311066376772,-15.9528968895007));
#49356=CARTESIAN_POINT('Ctrl Pts',(4.15138652022233,42.7019861374178,-15.9693615490908));
#49357=CARTESIAN_POINT('Ctrl Pts',(4.08671233631728,42.7710801369558,-15.9858954857721));
#49358=CARTESIAN_POINT('Ctrl Pts',(4.01366422126778,42.8491203397498,-16.0045702155636));
#49359=CARTESIAN_POINT('Ctrl Pts',(3.93817953530957,42.9248840324747,-16.0233330708574));
#49360=CARTESIAN_POINT('Ctrl Pts',(3.86016029203208,42.9982987128954,-16.0421060217848));
#49361=CARTESIAN_POINT('Ctrl Pts',(3.8518401275407,43.0061278354493,-16.0441080155641));
#49362=CARTESIAN_POINT('Ctrl Pts',(3.84349115471137,43.0139302653613,-16.0461101186922));
#49363=CARTESIAN_POINT('Ctrl Pts',(3.83511326420841,43.0217059258672,-16.0481122332415));
#49364=CARTESIAN_POINT('Ctrl Pts',(3.76493060726311,43.0868436253411,-16.0648842020959));
#49365=CARTESIAN_POINT('Ctrl Pts',(3.69271486095244,43.1500991909802,-16.0816562485315));
#49366=CARTESIAN_POINT('Ctrl Pts',(3.61837518308114,43.2114031096698,-16.0983651920145));
#49367=CARTESIAN_POINT('Ctrl Pts',(3.61006299158089,43.218257725219,-16.1002334801477));
#49368=CARTESIAN_POINT('Ctrl Pts',(3.60172445231722,43.2250877486212,-16.102100932142));
#49369=CARTESIAN_POINT('Ctrl Pts',(3.59335932873714,43.231893174722,-16.1039674842747));
#49370=CARTESIAN_POINT('Ctrl Pts',(3.55985259783473,43.2591524947852,-16.1114440098067));
#49371=CARTESIAN_POINT('Ctrl Pts',(3.52591396943127,43.2860208906304,-16.118907152479));
#49372=CARTESIAN_POINT('Ctrl Pts',(3.49153886080801,43.3124866299023,-16.1263497545402));
#49373=CARTESIAN_POINT('Ctrl Pts',(3.48330870851789,43.3188231063064,-16.1281316761355));
#49374=CARTESIAN_POINT('Ctrl Pts',(3.47505293205268,43.3251369536414,-16.1299125489504));
#49375=CARTESIAN_POINT('Ctrl Pts',(3.46677335588102,43.3314265638105,-16.1316918672206));
#49376=CARTESIAN_POINT('Ctrl Pts',(3.46424918367963,43.333344060409,-16.1322343232138));
#49377=CARTESIAN_POINT('Ctrl Pts',(3.46172361412074,43.3352586871739,-16.132776459702));
#49378=CARTESIAN_POINT('Ctrl Pts',(3.45919669857441,43.337170407617,-16.1333182638196));
#49379=CARTESIAN_POINT('Ctrl Pts',(3.44838120836836,43.3453527917724,-16.1356372479805));
#49380=CARTESIAN_POINT('Ctrl Pts',(3.43753889753725,43.353483581322,-16.1379506072427));
#49381=CARTESIAN_POINT('Ctrl Pts',(3.42666980412844,43.3615628623861,-16.1402581785502));
#49382=CARTESIAN_POINT('Ctrl Pts',(3.4049316173108,43.3777214245144,-16.1448733211651));
#49383=CARTESIAN_POINT('Ctrl Pts',(3.38308629026371,43.3936739435806,-16.1494653142701));
#49384=CARTESIAN_POINT('Ctrl Pts',(3.36113403095232,43.4094213680059,-16.1540328721413));
#49385=CARTESIAN_POINT('Ctrl Pts',(3.35312024544098,43.4151700465319,-16.1557002827059));
#49386=CARTESIAN_POINT('Ctrl Pts',(3.34509218035729,43.4208913270488,-16.157364442952));
#49387=CARTESIAN_POINT('Ctrl Pts',(3.33704985191415,43.4265852616513,-16.1590252888546));
#49388=CARTESIAN_POINT('Ctrl Pts',(3.25697039112238,43.4832811819894,-16.1755627438067));
#49389=CARTESIAN_POINT('Ctrl Pts',(3.17548097013196,43.5372743319747,-16.1917713019819));
#49390=CARTESIAN_POINT('Ctrl Pts',(3.09258174654553,43.5885854537716,-16.2075894156856));
#49391=CARTESIAN_POINT('Ctrl Pts',(3.00135700756265,43.6450497183369,-16.2249961323156));
#49392=CARTESIAN_POINT('Ctrl Pts',(2.90842605358659,43.698268165434,-16.2419299379221));
#49393=CARTESIAN_POINT('Ctrl Pts',(2.81377567269317,43.7482407963283,-16.2583106986815));
#49394=CARTESIAN_POINT('Ctrl Pts',(2.80721705605344,43.7517035539572,-16.2594457720861));
#49395=CARTESIAN_POINT('Ctrl Pts',(2.80065019446355,43.7551507511571,-16.2605781876481));
#49396=CARTESIAN_POINT('Ctrl Pts',(2.7940750859381,43.7585823937821,-16.2617079181173));
#49397=CARTESIAN_POINT('Ctrl Pts',(2.70576181166361,43.8046743472732,-16.2768818420762));
#49398=CARTESIAN_POINT('Ctrl Pts',(2.61595748637249,43.8479530702011,-16.2915716528802));
#49399=CARTESIAN_POINT('Ctrl Pts',(2.52463667353454,43.888389861414,-16.3057109554111));
#49400=CARTESIAN_POINT('Ctrl Pts',(2.51914011705615,43.8908237327277,-16.3065619933346));
#49401=CARTESIAN_POINT('Ctrl Pts',(2.51363806443321,43.8932473037575,-16.307411037061));
#49402=CARTESIAN_POINT('Ctrl Pts',(2.50813050985484,43.8956605680324,-16.3082580720792));
#49403=CARTESIAN_POINT('Ctrl Pts',(2.41532189681294,43.936326839617,-16.3225315838741));
#49404=CARTESIAN_POINT('Ctrl Pts',(2.32095115683523,43.9740667478834,-16.3362348517856));
#49405=CARTESIAN_POINT('Ctrl Pts',(2.22497391796444,44.0088152926355,-16.3492963499814));
#49406=CARTESIAN_POINT('Ctrl Pts',(2.22078398009584,44.0103322590043,-16.3498665566945));
#49407=CARTESIAN_POINT('Ctrl Pts',(2.21659097944139,44.011843522778,-16.3504355403514));
#49408=CARTESIAN_POINT('Ctrl Pts',(2.21239491225654,44.0133490785428,-16.3510032949731));
#49409=CARTESIAN_POINT('Ctrl Pts',(2.16568019776689,44.0301103944604,-16.3573240934465));
#49410=CARTESIAN_POINT('Ctrl Pts',(2.11858514986288,44.0461637036814,-16.3634925290769));
#49411=CARTESIAN_POINT('Ctrl Pts',(2.07110297782734,44.0614982206348,-16.3695000678039));
#49412=CARTESIAN_POINT('Ctrl Pts',(2.06766461695933,44.0626086501026,-16.369935096051));
#49413=CARTESIAN_POINT('Ctrl Pts',(2.06422431548232,44.0637152812176,-16.3703692692713));
#49414=CARTESIAN_POINT('Ctrl Pts',(2.06078205357121,44.0648181159706,-16.3708025865466));
#49415=CARTESIAN_POINT('Ctrl Pts',(2.0353054952823,44.0729803170441,-16.3740096152693));
#49416=CARTESIAN_POINT('Ctrl Pts',(2.00972154956067,44.0809345613566,-16.3771697632539));
#49417=CARTESIAN_POINT('Ctrl Pts',(1.98402190675294,44.0886811098014,-16.3802825700146));
#49418=CARTESIAN_POINT('Ctrl Pts',(1.96093443196556,44.0956402820843,-16.3830789842739));
#49419=CARTESIAN_POINT('Ctrl Pts',(1.93774050146882,44.102435507638,-16.3858387078791));
#49420=CARTESIAN_POINT('Ctrl Pts',(1.91447177282552,44.1090558359448,-16.3885569152829));
#49421=CARTESIAN_POINT('Ctrl Pts',(1.91185576698155,44.109800131768,-16.3888625119728));
#49422=CARTESIAN_POINT('Ctrl Pts',(1.90923900132739,44.1105421640974,-16.3891675621339));
#49423=CARTESIAN_POINT('Ctrl Pts',(1.90662152694395,44.1112819164273,-16.3894720583976));
#49424=CARTESIAN_POINT('Ctrl Pts',(1.80384027180714,44.140330022281,-16.4014288165477));
#49425=CARTESIAN_POINT('Ctrl Pts',(1.70067567536909,44.1656739884806,-16.412450946857));
#49426=CARTESIAN_POINT('Ctrl Pts',(1.59703092198111,44.1874452736728,-16.4225300192871));
#49427=CARTESIAN_POINT('Ctrl Pts',(1.59623408355844,44.1876126550016,-16.4226075089035));
#49428=CARTESIAN_POINT('Ctrl Pts',(1.59543721887446,44.1877798245714,-16.4226849425315));
#49429=CARTESIAN_POINT('Ctrl Pts',(1.59464032793329,44.1879467824285,-16.4227623201619));
#49430=CARTESIAN_POINT('Ctrl Pts',(1.4902358885778,44.2098207184566,-16.4328999283282));
#49431=CARTESIAN_POINT('Ctrl Pts',(1.38538072211209,44.2280603589026,-16.4420763846834));
#49432=CARTESIAN_POINT('Ctrl Pts',(1.28007904888983,44.2427191450539,-16.450270442415));
#49433=CARTESIAN_POINT('Ctrl Pts',(1.27897978977937,44.2428721702028,-16.4503559813465));
#49434=CARTESIAN_POINT('Ctrl Pts',(1.27788048201033,44.2430248051197,-16.4504414132241));
#49435=CARTESIAN_POINT('Ctrl Pts',(1.27678112558196,44.2431770498101,-16.450526738023));
#49436=CARTESIAN_POINT('Ctrl Pts',(1.17261275427984,44.2576028365959,-16.4586116003123));
#49437=CARTESIAN_POINT('Ctrl Pts',(1.06800752483145,44.268525295453,-16.4657350787401));
#49438=CARTESIAN_POINT('Ctrl Pts',(0.962964461020188,44.2759488312969,-16.471876014796));
#49439=CARTESIAN_POINT('Ctrl Pts',(0.959893094589279,44.2761658889299,-16.4720555703437));
#49440=CARTESIAN_POINT('Ctrl Pts',(0.956821353860735,44.2763799553317,-16.4722342859168));
#49441=CARTESIAN_POINT('Ctrl Pts',(0.953749238691236,44.2765910294275,-16.4724121609579));
#49442=CARTESIAN_POINT('Ctrl Pts',(0.850687348730451,44.2836720449596,-16.4783794300541));
#49443=CARTESIAN_POINT('Ctrl Pts',(0.747204104196679,44.2873859651881,-16.4834007362283));
#49444=CARTESIAN_POINT('Ctrl Pts',(0.643293723744948,44.2876920068837,-16.4874550245025));
#49445=CARTESIAN_POINT('Ctrl Pts',(0.638173013631758,44.2877070886378,-16.4876548200848));
#49446=CARTESIAN_POINT('Ctrl Pts',(0.633051265512239,44.2877138871714,-16.4878522670302));
#49447=CARTESIAN_POINT('Ctrl Pts',(0.627928478272138,44.2877123933833,-16.4880473626812));
#49448=CARTESIAN_POINT('Ctrl Pts',(0.57954225879359,44.2876982841195,-16.4898900980021));
#49449=CARTESIAN_POINT('Ctrl Pts',(0.531063351358693,44.2869444885894,-16.4915230658722));
#49450=CARTESIAN_POINT('Ctrl Pts',(0.482490764213168,44.2854433093263,-16.492944026536));
#49451=CARTESIAN_POINT('Ctrl Pts',(0.47631563182451,44.285252461335,-16.4931246761726));
#49452=CARTESIAN_POINT('Ctrl Pts',(0.470138985065216,44.2850495309885,-16.4933018991296));
#49453=CARTESIAN_POINT('Ctrl Pts',(0.463960821511663,44.2848344986047,-16.4934756906589));
#49454=CARTESIAN_POINT('Ctrl Pts',(0.443272462987042,44.2841144355938,-16.4940576534764));
#49455=CARTESIAN_POINT('Ctrl Pts',(0.422567101634483,44.2832586764287,-16.4946011385449));
#49456=CARTESIAN_POINT('Ctrl Pts',(0.401844644788766,44.282266486453,-16.4951059675728));
#49457=CARTESIAN_POINT('Ctrl Pts',(0.395134665523894,44.2819452130532,-16.495269432375));
#49458=CARTESIAN_POINT('Ctrl Pts',(0.38842289375111,44.2816096343698,-16.4954288441383));
#49459=CARTESIAN_POINT('Ctrl Pts',(0.381709326061794,44.2812597228911,-16.4955841967083));
#49460=CARTESIAN_POINT('Ctrl Pts',(0.374961908381315,44.2809080471491,-16.4957403325702));
#49461=CARTESIAN_POINT('Ctrl Pts',(0.368212082100221,44.2805418556977,-16.4958923819046));
#49462=CARTESIAN_POINT('Ctrl Pts',(0.361459979158117,44.2801611282481,-16.4960403334699));
#49463=CARTESIAN_POINT('Ctrl Pts',(0.354478999419505,44.2797674952372,-16.4961933001662));
#49464=CARTESIAN_POINT('Ctrl Pts',(0.347499905430398,44.2793586053598,-16.4963418025197));
#49465=CARTESIAN_POINT('Ctrl Pts',(0.340516126202715,44.2789339995285,-16.4964859594806));
#49466=CARTESIAN_POINT('Ctrl Pts',(0.334023738302003,44.2785392697308,-16.4966199732973));
#49467=CARTESIAN_POINT('Ctrl Pts',(0.327529005644791,44.2781310584524,-16.4967501936259));
#49468=CARTESIAN_POINT('Ctrl Pts',(0.3210340492655,44.2777094964746,-16.496876587379));
#49469=CARTESIAN_POINT('',(1.20079349241742E-9,44.2459666925969,-16.5000000000016));
#49470=CARTESIAN_POINT('Origin',(0.582847305389121,39.8653351592355,-15.2258139418661));
#49471=CARTESIAN_POINT('Ctrl Pts',(1.19175561086315E-9,44.2459666925957,
-16.5000000000016));
#49472=CARTESIAN_POINT('Ctrl Pts',(-0.000287594851848401,44.2459284389849,
-16.5000000000006));
#49473=CARTESIAN_POINT('Ctrl Pts',(-0.000575187647762856,44.2458901592331,
-16.4999999924808));
#49474=CARTESIAN_POINT('Ctrl Pts',(-0.000862777466105232,44.2458518533049,
-16.4999999774429));
#49475=CARTESIAN_POINT('Ctrl Pts',(-0.0103516191796766,44.2445879737586,
-16.4999994812757));
#49476=CARTESIAN_POINT('Ctrl Pts',(-0.0198372289636732,44.2432956404934,
-16.4999908074579));
#49477=CARTESIAN_POINT('Ctrl Pts',(-0.0293292763690019,44.2419734378186,
-16.4999739378784));
#49478=CARTESIAN_POINT('Ctrl Pts',(-0.126346576415198,44.2284593319417,
-16.4998015155357));
#49479=CARTESIAN_POINT('Ctrl Pts',(-0.22254089868835,44.2120370516237,-16.4987750615445));
#49480=CARTESIAN_POINT('Ctrl Pts',(-0.31793273935584,44.1927764300431,-16.4969366481553));
#49481=CARTESIAN_POINT('Ctrl Pts',(-0.329950839341052,44.1903498485418,
-16.4967050325814));
#49482=CARTESIAN_POINT('Ctrl Pts',(-0.341956199703173,44.1878782093579,
-16.4964605269095));
#49483=CARTESIAN_POINT('Ctrl Pts',(-0.353948844961121,44.1853615808569,
-16.4962032109953));
#49484=CARTESIAN_POINT('Ctrl Pts',(-0.446812032272869,44.1658744586372,
-16.4942107251494));
#49485=CARTESIAN_POINT('Ctrl Pts',(-0.53891338367438,44.1436920944281,-16.4914501879687));
#49486=CARTESIAN_POINT('Ctrl Pts',(-0.630262954075812,44.1188466417855,
-16.48795829109));
#49487=CARTESIAN_POINT('Ctrl Pts',(-0.644348813976517,44.1150155393123,
-16.4874198499128));
#49488=CARTESIAN_POINT('Ctrl Pts',(-0.658416797366746,44.1111211141125,
-16.4868640168006));
#49489=CARTESIAN_POINT('Ctrl Pts',(-0.672466915608358,44.1071633726003,
-16.486290922113));
#49490=CARTESIAN_POINT('Ctrl Pts',(-0.761656457698557,44.08203980089,-16.4826529418566));
#49491=CARTESIAN_POINT('Ctrl Pts',(-0.850126501765724,44.0543665861713,
-16.4783194037139));
#49492=CARTESIAN_POINT('Ctrl Pts',(-0.937878878218134,44.0241463006682,
-16.4733233808419));
#49493=CARTESIAN_POINT('Ctrl Pts',(-0.953599764081856,44.0187323201201,
-16.4724283406331));
#49494=CARTESIAN_POINT('Ctrl Pts',(-0.969297601751398,44.013236528157,-16.4715120357243));
#49495=CARTESIAN_POINT('Ctrl Pts',(-0.984972374783481,44.0076588214043,
-16.4705746539486));
#49496=CARTESIAN_POINT('Ctrl Pts',(-1.02006761572815,43.9951705409039,-16.468475890591));
#49497=CARTESIAN_POINT('Ctrl Pts',(-1.05504725157008,43.9822717635392,-16.4662714695351));
#49498=CARTESIAN_POINT('Ctrl Pts',(-1.08991105395408,43.9689613980953,-16.4639634928673));
#49499=CARTESIAN_POINT('Ctrl Pts',(-1.10629194689102,43.9627074712033,-16.4628790810674));
#49500=CARTESIAN_POINT('Ctrl Pts',(-1.122647264236,43.9563626635983,-16.4617718079304));
#49501=CARTESIAN_POINT('Ctrl Pts',(-1.13897696696911,43.9499267937656,-16.460641891158));
#49502=CARTESIAN_POINT('Ctrl Pts',(-1.14781951505116,43.9464417647129,-16.4600300402535));
#49503=CARTESIAN_POINT('Ctrl Pts',(-1.15665336778823,43.9429305052519,-16.4594116322874));
#49504=CARTESIAN_POINT('Ctrl Pts',(-1.16547967269564,43.9393925413287,-16.4587866239445));
#49505=CARTESIAN_POINT('Ctrl Pts',(-1.18214872627634,43.9327108652683,-16.4576062548471));
#49506=CARTESIAN_POINT('Ctrl Pts',(-1.19880065193612,43.92592977154,-16.4564015924395));
#49507=CARTESIAN_POINT('Ctrl Pts',(-1.21541537661102,43.919057552372,-16.4551744063969));
#49508=CARTESIAN_POINT('Ctrl Pts',(-1.22386355918631,43.9155631964098,-16.4545504122024));
#49509=CARTESIAN_POINT('Ctrl Pts',(-1.23229930086346,43.9120464177848,-16.4539208013987));
#49510=CARTESIAN_POINT('Ctrl Pts',(-1.24071965867521,43.9085084561819,-16.4532858337956));
#49511=CARTESIAN_POINT('Ctrl Pts',(-1.25762786584244,43.9014041752157,-16.4520108091447));
#49512=CARTESIAN_POINT('Ctrl Pts',(-1.27447653768259,43.8942138491217,-16.4507140885787));
#49513=CARTESIAN_POINT('Ctrl Pts',(-1.29127166034123,43.8869356668845,-16.4493956999265));
#49514=CARTESIAN_POINT('Ctrl Pts',(-1.37385183559153,43.8511494700897,-16.4429132961857));
#49515=CARTESIAN_POINT('Ctrl Pts',(-1.45507840509518,43.8132674301109,-16.4359115711727));
#49516=CARTESIAN_POINT('Ctrl Pts',(-1.53499451539265,43.7733496234825,-16.4284445958157));
#49517=CARTESIAN_POINT('Ctrl Pts',(-1.55246848750381,43.7646214379243,-16.4268119122597));
#49518=CARTESIAN_POINT('Ctrl Pts',(-1.56987994576714,43.7557961626709,-16.4251570101115));
#49519=CARTESIAN_POINT('Ctrl Pts',(-1.58722914805154,43.7468741126144,-16.4234804086485));
#49520=CARTESIAN_POINT('Ctrl Pts',(-1.68392383369332,43.6971476288631,-16.4141359760485));
#49521=CARTESIAN_POINT('Ctrl Pts',(-1.77868541818864,43.6444153556874,-16.4041175368783));
#49522=CARTESIAN_POINT('Ctrl Pts',(-1.87156724575009,43.5887474390751,-16.3935133157434));
#49523=CARTESIAN_POINT('Ctrl Pts',(-1.94591646107952,43.5441868826368,-16.3850249435693));
#49524=CARTESIAN_POINT('Ctrl Pts',(-2.01905972959809,43.497742839128,-16.3761613437901));
#49525=CARTESIAN_POINT('Ctrl Pts',(-2.09101827632614,43.4494412260899,-16.3669680322317));
#49526=CARTESIAN_POINT('Ctrl Pts',(-2.10895497999385,43.4374013537032,-16.3646764669813));
#49527=CARTESIAN_POINT('Ctrl Pts',(-2.1268178795326,43.4252457496787,-16.3623643762301));
#49528=CARTESIAN_POINT('Ctrl Pts',(-2.14460708840311,43.4129744720201,-16.3600324324806));
#49529=CARTESIAN_POINT('Ctrl Pts',(-2.2152949005473,43.3642129011028,-16.3507661406011));
#49530=CARTESIAN_POINT('Ctrl Pts',(-2.28482159990252,43.3136289353957,-16.3411860785326));
#49531=CARTESIAN_POINT('Ctrl Pts',(-2.35319652713571,43.261229959548,-16.3313338740189));
#49532=CARTESIAN_POINT('Ctrl Pts',(-2.37106047535531,43.2475399619249,-16.3287598417178));
#49533=CARTESIAN_POINT('Ctrl Pts',(-2.38884576178364,43.2337260025664,-16.3261672273417));
#49534=CARTESIAN_POINT('Ctrl Pts',(-2.40655245014132,43.2197880421058,-16.3235567627833));
#49535=CARTESIAN_POINT('Ctrl Pts',(-2.43131192910212,43.2002984214716,-16.319906518254));
#49536=CARTESIAN_POINT('Ctrl Pts',(-2.4559177628072,43.1805664117049,-16.3162213666243));
#49537=CARTESIAN_POINT('Ctrl Pts',(-2.48037013200753,43.1605919335146,-16.3125033029344));
#49538=CARTESIAN_POINT('Ctrl Pts',(-2.49812747829513,43.1460864382296,-16.3098032396432));
#49539=CARTESIAN_POINT('Ctrl Pts',(-2.51580388217014,43.1314530555792,-16.3070858189739));
#49540=CARTESIAN_POINT('Ctrl Pts',(-2.53339936203802,43.1166916692541,-16.3043518017035));
#49541=CARTESIAN_POINT('Ctrl Pts',(-2.53659528477317,43.114010511905,-16.3038552134878));
#49542=CARTESIAN_POINT('Ctrl Pts',(-2.53978839688599,43.1113252501751,-16.303358099636));
#49543=CARTESIAN_POINT('Ctrl Pts',(-2.54297873799425,43.108635851673,-16.3028604587695));
#49544=CARTESIAN_POINT('Ctrl Pts',(-2.5564235447244,43.0973021284585,-16.3007632895188));
#49545=CARTESIAN_POINT('Ctrl Pts',(-2.56982581198324,43.0858891047701,-16.2986556897146));
#49546=CARTESIAN_POINT('Ctrl Pts',(-2.5831748059359,43.0744062107563,-16.2965397397059));
#49547=CARTESIAN_POINT('Ctrl Pts',(-2.58738539041937,43.0707842377798,-16.2958723196512));
#49548=CARTESIAN_POINT('Ctrl Pts',(-2.59159015953406,43.0671557509872,-16.2952041496852));
#49549=CARTESIAN_POINT('Ctrl Pts',(-2.59578791111343,43.0635217980843,-16.2945354333241));
#49550=CARTESIAN_POINT('Ctrl Pts',(-2.59883434722028,43.0608845278398,-16.2940501255041));
#49551=CARTESIAN_POINT('Ctrl Pts',(-2.60187735140753,43.0582441402771,-16.293564487923));
#49552=CARTESIAN_POINT('Ctrl Pts',(-2.60491671719938,43.0556008159899,-16.2930785579784));
#49553=CARTESIAN_POINT('Ctrl Pts',(-2.62249340560043,43.0403144403046,-16.290268419349));
#49554=CARTESIAN_POINT('Ctrl Pts',(-2.63995009420414,43.0249295007639,-16.287448475097));
#49555=CARTESIAN_POINT('Ctrl Pts',(-2.65728973642841,43.0094452202597,-16.2846192743798));
#49556=CARTESIAN_POINT('Ctrl Pts',(-2.73864180813259,42.9367979140711,-16.2713455668467));
#49557=CARTESIAN_POINT('Ctrl Pts',(-2.81740647187134,42.8619806646524,-16.257869986989));
#49558=CARTESIAN_POINT('Ctrl Pts',(-2.89370698839488,42.7850844218323,-16.2442772420212));
#49559=CARTESIAN_POINT('Ctrl Pts',(-2.9532230042938,42.7251037268282,-16.2336746135925));
#49560=CARTESIAN_POINT('Ctrl Pts',(-3.01123780484442,42.6638563555137,-16.2230009895172));
#49561=CARTESIAN_POINT('Ctrl Pts',(-3.0678032857904,42.601379891981,-16.2122972770594));
#49562=CARTESIAN_POINT('Ctrl Pts',(-3.08375568676903,42.5837604961705,-16.2092786531525));
#49563=CARTESIAN_POINT('Ctrl Pts',(-3.09959271192341,42.5660432617362,-16.2062576035456));
#49564=CARTESIAN_POINT('Ctrl Pts',(-3.1153150843048,42.5482286686331,-16.2032349211562));
#49565=CARTESIAN_POINT('Ctrl Pts',(-3.18678728121458,42.4672454636026,-16.189494135371));
#49566=CARTESIAN_POINT('Ctrl Pts',(-3.25589359579216,42.3842532040227,-16.1757190417709));
#49567=CARTESIAN_POINT('Ctrl Pts',(-3.32271183889098,42.2993064142606,-16.1619814398496));
#49568=CARTESIAN_POINT('Ctrl Pts',(-3.37482391194637,42.2330557451528,-16.1512673761191));
#49569=CARTESIAN_POINT('Ctrl Pts',(-3.42554300779128,42.1656150910847,-16.1405763359259));
#49570=CARTESIAN_POINT('Ctrl Pts',(-3.47490173611287,42.0970065664878,-16.1299428989804));
#49571=CARTESIAN_POINT('Ctrl Pts',(-3.48883090471556,42.0776450525431,-16.1269421138898));
#49572=CARTESIAN_POINT('Ctrl Pts',(-3.50265152984663,42.0581903586756,-16.1239458580045));
#49573=CARTESIAN_POINT('Ctrl Pts',(-3.51636409988177,42.0386427804829,-16.1209548424507));
#49574=CARTESIAN_POINT('Ctrl Pts',(-3.56510545985841,41.9691608713351,-16.1103232711678));
#49575=CARTESIAN_POINT('Ctrl Pts',(-3.61247340068011,41.8985222806704,-16.099759789884));
#49576=CARTESIAN_POINT('Ctrl Pts',(-3.65851424794237,41.8267064889586,-16.0892906461908));
#49577=CARTESIAN_POINT('Ctrl Pts',(-3.67132523342633,41.8067235581516,-16.0863775797323));
#49578=CARTESIAN_POINT('Ctrl Pts',(-3.68403837676501,41.7866413785747,-16.0834706554539));
#49579=CARTESIAN_POINT('Ctrl Pts',(-3.69664022626714,41.7664823851024,-16.0805737153154));
#49580=CARTESIAN_POINT('Ctrl Pts',(-3.69855743306794,41.7634154575554,-16.0801329837121));
#49581=CARTESIAN_POINT('Ctrl Pts',(-3.70047201025498,41.7603468390133,-16.0796924955201));
#49582=CARTESIAN_POINT('Ctrl Pts',(-3.70238391075417,41.757276608805,-16.07925226425));
#49583=CARTESIAN_POINT('Ctrl Pts',(-3.71686830527126,41.7340168075681,-16.0759171098327));
#49584=CARTESIAN_POINT('Ctrl Pts',(-3.73118649436856,41.7106850658504,-16.0725996217207));
#49585=CARTESIAN_POINT('Ctrl Pts',(-3.74534174109064,41.6872813480322,-16.0693003967952));
#49586=CARTESIAN_POINT('Ctrl Pts',(-3.77366972281652,41.6404449979715,-16.0626978708744));
#49587=CARTESIAN_POINT('Ctrl Pts',(-3.80134529335873,41.5933204608883,-16.056168507382));
#49588=CARTESIAN_POINT('Ctrl Pts',(-3.82839252587146,41.5459065217004,-16.0497168407379));
#49589=CARTESIAN_POINT('Ctrl Pts',(-3.83991423543571,41.5257089049438,-16.0469685289007));
#49590=CARTESIAN_POINT('Ctrl Pts',(-3.85132220043387,41.5054588928288,-16.0442343936167));
#49591=CARTESIAN_POINT('Ctrl Pts',(-3.8626179551858,41.4851562470067,-16.0415147212928));
#49592=CARTESIAN_POINT('Ctrl Pts',(-3.91542972205789,41.3902339844763,-16.0287992627958));
#49593=CARTESIAN_POINT('Ctrl Pts',(-3.96577569488318,41.2941842813233,-16.0164031290562));
#49594=CARTESIAN_POINT('Ctrl Pts',(-4.01378102990947,41.1970584880573,-16.0043630454092));
#49595=CARTESIAN_POINT('Ctrl Pts',(-4.05205445786877,41.1196225728717,-15.994763794121));
#49596=CARTESIAN_POINT('Ctrl Pts',(-4.08883676825536,41.0415008769695,-15.9853916721705));
#49597=CARTESIAN_POINT('Ctrl Pts',(-4.12418854585123,40.9627184322293,-15.9762657976971));
#49598=CARTESIAN_POINT('Ctrl Pts',(-4.1775183427968,40.8438714585666,-15.9624989925826));
#49599=CARTESIAN_POINT('Ctrl Pts',(-4.22759059698956,40.7235199332857,-15.9492920561166));
#49600=CARTESIAN_POINT('Ctrl Pts',(-4.27455440445767,40.6017235175999,-15.9366948019296));
#49601=CARTESIAN_POINT('Ctrl Pts',(-4.30628985941116,40.5194204661253,-15.9281822980604));
#49602=CARTESIAN_POINT('Ctrl Pts',(-4.33660590845058,40.4364577805763,-15.9199481700165));
#49603=CARTESIAN_POINT('Ctrl Pts',(-4.36554553024948,40.3528526743455,-15.9120084283324));
#49604=CARTESIAN_POINT('Ctrl Pts',(-4.37221368788543,40.333588703607,-15.9101789832378));
#49605=CARTESIAN_POINT('Ctrl Pts',(-4.37880864040679,40.3142905709198,-15.9083651338701));
#49606=CARTESIAN_POINT('Ctrl Pts',(-4.38533078328216,40.2949584322355,-15.9065670430312));
#49607=CARTESIAN_POINT('Ctrl Pts',(-4.40274481558523,40.2433418862676,-15.9017661650757));
#49608=CARTESIAN_POINT('Ctrl Pts',(-4.41964036451411,40.191483202052,-15.8970774727432));
#49609=CARTESIAN_POINT('Ctrl Pts',(-4.43602545975743,40.1393855975829,-15.8925039099366));
#49610=CARTESIAN_POINT('Ctrl Pts',(-4.44421800737909,40.1133367953484,-15.8902171285334));
#49611=CARTESIAN_POINT('Ctrl Pts',(-4.45228294155174,40.0872282629743,-15.8879591292164));
#49612=CARTESIAN_POINT('Ctrl Pts',(-4.4602211938315,40.0610603695998,-15.8857302987635));
#49613=CARTESIAN_POINT('Ctrl Pts',(-4.46250714010584,40.0535249076041,-15.8850884715086));
#49614=CARTESIAN_POINT('Ctrl Pts',(-4.46478259945335,40.0459844688889,-15.8844490579797));
#49615=CARTESIAN_POINT('Ctrl Pts',(-4.4670475891545,40.0384390820634,-15.8838120687771));
#49616=CARTESIAN_POINT('Ctrl Pts',(-4.4726480772472,40.019782110224,-15.8822370283067));
#49617=CARTESIAN_POINT('Ctrl Pts',(-4.47818614257714,40.0010890903067,-15.8806763429741));
#49618=CARTESIAN_POINT('Ctrl Pts',(-4.48365551823457,39.9823832990067,-15.8791320027934));
#49619=CARTESIAN_POINT('Ctrl Pts',(-4.48594316046568,39.9745593423389,-15.8784860610922));
#49620=CARTESIAN_POINT('Ctrl Pts',(-4.48821884891952,39.9667329479437,-15.8778429610696));
#49621=CARTESIAN_POINT('Ctrl Pts',(-4.49048212941797,39.9589057970096,-15.8772028470187));
#49622=CARTESIAN_POINT('Ctrl Pts',(-4.49815744596312,39.9323620870686,-15.8750320697025));
#49623=CARTESIAN_POINT('Ctrl Pts',(-4.50569321252847,39.9057996224596,-15.8728947529067));
#49624=CARTESIAN_POINT('Ctrl Pts',(-4.51309160005012,39.8792187000441,-15.8707909131699));
#49625=CARTESIAN_POINT('Ctrl Pts',(-4.52789012262557,39.8260505766805,-15.86658273676));
#49626=CARTESIAN_POINT('Ctrl Pts',(-4.54213908424658,39.7728086148232,-15.8625085085832));
#49627=CARTESIAN_POINT('Ctrl Pts',(-4.55585476778786,39.7194950587087,-15.8585682624515));
#49628=CARTESIAN_POINT('Ctrl Pts',(-4.56041739946515,39.7017598784514,-15.857257508105));
#49629=CARTESIAN_POINT('Ctrl Pts',(-4.56492117524414,39.6840167959074,-15.8559615946077));
#49630=CARTESIAN_POINT('Ctrl Pts',(-4.56936658116792,39.6662658793576,-15.8546805129273));
#49631=CARTESIAN_POINT('Ctrl Pts',(-4.59582617304182,39.5606102844924,-15.8470553603542));
#49632=CARTESIAN_POINT('Ctrl Pts',(-4.62021701530607,39.4546766082389,-15.8399559209133));
#49633=CARTESIAN_POINT('Ctrl Pts',(-4.64264870943165,39.3484787986427,-15.8333781662229));
#49634=CARTESIAN_POINT('Ctrl Pts',(-4.66178195243537,39.2578967638623,-15.8277676323861));
#49635=CARTESIAN_POINT('Ctrl Pts',(-4.67948651884887,39.1671220345694,-15.8225376116097));
#49636=CARTESIAN_POINT('Ctrl Pts',(-4.69582718945552,39.0761629007493,-15.817686525125));
#49637=CARTESIAN_POINT('Ctrl Pts',(-4.71780191836416,38.9538421982777,-15.8111628448563));
#49638=CARTESIAN_POINT('Ctrl Pts',(-4.73730857665041,38.8311878214691,-15.8053242615517));
#49639=CARTESIAN_POINT('Ctrl Pts',(-4.75445938729691,38.7082138782734,-15.8001631138445));
#49640=CARTESIAN_POINT('Ctrl Pts',(-4.76754387615524,38.6143960860551,-15.7962256335083));
#49641=CARTESIAN_POINT('Ctrl Pts',(-4.77925615587046,38.5203921558907,-15.7926827509398));
#49642=CARTESIAN_POINT('Ctrl Pts',(-4.78964569348943,38.4262084972978,-15.7895311561511));
#49643=CARTESIAN_POINT('Ctrl Pts',(-4.80300125257063,38.3051371404239,-15.7854798391489));
#49644=CARTESIAN_POINT('Ctrl Pts',(-4.81417020258914,38.1837686885202,-15.7820749892995));
#49645=CARTESIAN_POINT('Ctrl Pts',(-4.82322444707439,38.0621123276519,-15.7793072293277));
#49646=CARTESIAN_POINT('Ctrl Pts',(-4.83045479780361,37.964962514771,-15.777097008987));
#49647=CARTESIAN_POINT('Ctrl Pts',(-4.83633583316492,37.8676289962459,-15.7752932949556));
#49648=CARTESIAN_POINT('Ctrl Pts',(-4.84090392814595,37.7701165801615,-15.773891376532));
#49649=CARTESIAN_POINT('Ctrl Pts',(-4.84650627563929,37.6505265886908,-15.7721720527879));
#49650=CARTESIAN_POINT('Ctrl Pts',(-4.85013347106028,37.530667475693,-15.7710569786778));
#49651=CARTESIAN_POINT('Ctrl Pts',(-4.85182630775392,37.4105445950497,-15.7705360637344));
#49652=CARTESIAN_POINT('Ctrl Pts',(-4.85324388282397,37.3099541473224,-15.7700998515232));
#49653=CARTESIAN_POINT('Ctrl Pts',(-4.85330572152953,37.209171080088,-15.770080067804));
#49654=CARTESIAN_POINT('Ctrl Pts',(-4.8520335653668,37.1082211610075,-15.7704714666542));
#49655=CARTESIAN_POINT('Ctrl Pts',(-4.85192676926515,37.099746527047,-15.7705043241544));
#49656=CARTESIAN_POINT('Ctrl Pts',(-4.8518105219929,37.0912699173234,-15.770540088642));
#49657=CARTESIAN_POINT('Ctrl Pts',(-4.85168485778478,37.0827921015805,-15.7705787486076));
#49658=CARTESIAN_POINT('Ctrl Pts',(-4.85127921342682,37.0554256925192,-15.7707035430673));
#49659=CARTESIAN_POINT('Ctrl Pts',(-4.85077526171592,37.0280351670598,-15.770858564662));
#49660=CARTESIAN_POINT('Ctrl Pts',(-4.85017447792787,37.0006622449712,-15.7710433266669));
#49661=CARTESIAN_POINT('Ctrl Pts',(-4.84974491910744,36.981090678032,-15.771175431012));
#49662=CARTESIAN_POINT('Ctrl Pts',(-4.84926584985124,36.9615265823381,-15.7713227417006));
#49663=CARTESIAN_POINT('Ctrl Pts',(-4.84873760633707,36.9419757558118,-15.771485143286));
#49664=CARTESIAN_POINT('Ctrl Pts',(-4.84852704500225,36.9341826679273,-15.7715498776248));
#49665=CARTESIAN_POINT('Ctrl Pts',(-4.84830867043275,36.9263909650895,-15.7716170097219));
#49666=CARTESIAN_POINT('Ctrl Pts',(-4.84808249521163,36.9186004218509,-15.7716865344286));
#49667=CARTESIAN_POINT('Ctrl Pts',(-4.84670202473089,36.8710504961042,-15.7721108815558));
#49668=CARTESIAN_POINT('Ctrl Pts',(-4.84503135746484,36.8235578278631,-15.7726242373588));
#49669=CARTESIAN_POINT('Ctrl Pts',(-4.84307509951819,36.7761213163914,-15.7732248947521));
#49670=CARTESIAN_POINT('Ctrl Pts',(-4.84278217273655,36.7690182527789,-15.7733148361821));
#49671=CARTESIAN_POINT('Ctrl Pts',(-4.84248284554652,36.7619164477046,-15.7734067348033));
#49672=CARTESIAN_POINT('Ctrl Pts',(-4.84217713097072,36.7548158979564,-15.7735005850902));
#49673=CARTESIAN_POINT('Ctrl Pts',(-4.83773173738744,36.6515668519931,-15.7748652614787));
#49674=CARTESIAN_POINT('Ctrl Pts',(-4.83193543756466,36.5485837374455,-15.7766427083583));
#49675=CARTESIAN_POINT('Ctrl Pts',(-4.82482921851815,36.4458582091488,-15.7788156403514));
#49676=CARTESIAN_POINT('Ctrl Pts',(-4.81692578793011,36.331608412288,-15.7812323428295));
#49677=CARTESIAN_POINT('Ctrl Pts',(-4.80740475334953,36.2176767076784,-15.7841380325327));
#49678=CARTESIAN_POINT('Ctrl Pts',(-4.79630431060394,36.1040551082918,-15.7875103516748));
#49679=CARTESIAN_POINT('Ctrl Pts',(-4.78608080239418,35.9994096107421,-15.7906162577387));
#49680=CARTESIAN_POINT('Ctrl Pts',(-4.77451712190974,35.8950272726645,-15.7941181161817));
#49681=CARTESIAN_POINT('Ctrl Pts',(-4.76164247051096,35.79090180384,-15.7979986385364));
#49682=CARTESIAN_POINT('Ctrl Pts',(-4.74796918719025,35.6803172923034,-15.8021198749058));
#49683=CARTESIAN_POINT('Ctrl Pts',(-4.73281698420083,35.570022559524,-15.8066682685036));
#49684=CARTESIAN_POINT('Ctrl Pts',(-4.71620044368527,35.4600140912944,-15.811624538894));
#49685=CARTESIAN_POINT('Ctrl Pts',(-4.70020316056091,35.35410536675,-15.8163961013383));
#49686=CARTESIAN_POINT('Ctrl Pts',(-4.68284862312618,35.2484619634817,-15.8215457136102));
#49687=CARTESIAN_POINT('Ctrl Pts',(-4.66415019672067,35.1430804795454,-15.8270560415562));
#49688=CARTESIAN_POINT('Ctrl Pts',(-4.64513855063192,35.0359337371696,-15.8326586736959));
#49689=CARTESIAN_POINT('Ctrl Pts',(-4.62473763649585,34.9290577615093,-15.8386342613376));
#49690=CARTESIAN_POINT('Ctrl Pts',(-4.60294317012863,34.8224525312729,-15.8449655287671));
#49691=CARTESIAN_POINT('Ctrl Pts',(-4.5810634426253,34.715430255586,-15.8513215644586));
#49692=CARTESIAN_POINT('Ctrl Pts',(-4.55777905932879,34.608680891025,-15.8580361206368));
#49693=CARTESIAN_POINT('Ctrl Pts',(-4.53308543856788,34.5022042629151,-15.8650917553867));
#49694=CARTESIAN_POINT('Ctrl Pts',(-4.50898951620644,34.3983048554899,-15.8719766115523));
#49695=CARTESIAN_POINT('Ctrl Pts',(-4.48355205009227,34.2946650869156,-15.8791862918112));
#49696=CARTESIAN_POINT('Ctrl Pts',(-4.45675032829542,34.1912883713624,-15.8867050896647));
#49697=CARTESIAN_POINT('Ctrl Pts',(-4.42875904625923,34.0833234121347,-15.8945575997715));
#49698=CARTESIAN_POINT('Ctrl Pts',(-4.39927978459254,33.9756453684566,-15.9027472583645));
#49699=CARTESIAN_POINT('Ctrl Pts',(-4.36828648579626,33.8682579088737,-15.9112561785133));
#49700=CARTESIAN_POINT('Ctrl Pts',(-4.33919134807026,33.7674473127784,-15.9192439763033));
#49701=CARTESIAN_POINT('Ctrl Pts',(-4.30876259816216,33.666892675998,-15.9275131965253));
#49702=CARTESIAN_POINT('Ctrl Pts',(-4.27695790139735,33.566601036888,-15.9360490739371));
#49703=CARTESIAN_POINT('Ctrl Pts',(-4.24411573854768,33.4630378943601,-15.9448633908317));
#49704=CARTESIAN_POINT('Ctrl Pts',(-4.20980950791299,33.3597545148029,-15.9539612235864));
#49705=CARTESIAN_POINT('Ctrl Pts',(-4.17398692835289,33.2567596124214,-15.9633277669116));
#49706=CARTESIAN_POINT('Ctrl Pts',(-4.17220721605076,33.2516426918345,-15.9637931089554));
#49707=CARTESIAN_POINT('Ctrl Pts',(-4.17042372259689,33.2465263637597,-15.9642591242467));
#49708=CARTESIAN_POINT('Ctrl Pts',(-4.16863646163622,33.2414106840141,-15.9647258056854));
#49709=CARTESIAN_POINT('Ctrl Pts',(-4.16143009229477,33.22078388217,-15.9666075000131));
#49710=CARTESIAN_POINT('Ctrl Pts',(-4.15416326324634,33.2001706046279,-15.9684997646203));
#49711=CARTESIAN_POINT('Ctrl Pts',(-4.14684307676731,33.1795915530405,-15.9704005109544));
#49712=CARTESIAN_POINT('Ctrl Pts',(-4.14494846185095,33.1742652709555,-15.9708924632247));
#49713=CARTESIAN_POINT('Ctrl Pts',(-4.1430501332869,33.1689408886548,-15.97138501989));
#49714=CARTESIAN_POINT('Ctrl Pts',(-4.14114820751058,33.1636187511498,-15.9718781463994));
#49715=CARTESIAN_POINT('Ctrl Pts',(-4.13387920555399,33.1432779847438,-15.9737628348592));
#49716=CARTESIAN_POINT('Ctrl Pts',(-4.12655565032035,33.1229642452263,-15.9756563719269));
#49717=CARTESIAN_POINT('Ctrl Pts',(-4.1191783081669,33.1026802646875,-15.9775583262229));
#49718=CARTESIAN_POINT('Ctrl Pts',(-4.11716917926544,33.0971561706859,-15.9780763002122));
#49719=CARTESIAN_POINT('Ctrl Pts',(-4.11515603619164,33.0916342148207,-15.9785949049451));
#49720=CARTESIAN_POINT('Ctrl Pts',(-4.11313887522014,33.0861143985711,-15.9791141366833));
#49721=CARTESIAN_POINT('Ctrl Pts',(-4.09646638643248,33.0404913294002,-15.9834057551793));
#49722=CARTESIAN_POINT('Ctrl Pts',(-4.07951944770782,32.9950144102283,-15.9877402079902));
#49723=CARTESIAN_POINT('Ctrl Pts',(-4.06229559308002,32.9496846741593,-15.9921153863065));
#49724=CARTESIAN_POINT('Ctrl Pts',(-4.06005348916727,32.9437839056728,-15.9926849222573));
#49725=CARTESIAN_POINT('Ctrl Pts',(-4.05780669057546,32.9378856329019,-15.9932551488779));
#49726=CARTESIAN_POINT('Ctrl Pts',(-4.05555519190291,32.9319898580281,-15.9938260614973));
#49727=CARTESIAN_POINT('Ctrl Pts',(-4.01648191768603,32.8296725743555,-16.0037338733933));
#49728=CARTESIAN_POINT('Ctrl Pts',(-3.97599387963302,32.728107175804,-16.0138483082294));
#49729=CARTESIAN_POINT('Ctrl Pts',(-3.93405403406182,32.6273098280652,-16.0241448713244));
#49730=CARTESIAN_POINT('Ctrl Pts',(-3.89516634421934,32.5338479675737,-16.0336921060991));
#49731=CARTESIAN_POINT('Ctrl Pts',(-3.85503360934473,32.4410447381093,-16.0433960887567));
#49732=CARTESIAN_POINT('Ctrl Pts',(-3.81361034359909,32.3489216104306,-16.0532367038211));
#49733=CARTESIAN_POINT('Ctrl Pts',(-3.76578719610018,32.2425654880018,-16.0645976908711));
#49734=CARTESIAN_POINT('Ctrl Pts',(-3.71624379047546,32.1371160266171,-16.0761408369553));
#49735=CARTESIAN_POINT('Ctrl Pts',(-3.66490807451357,32.0326063090271,-16.08783542948));
#49736=CARTESIAN_POINT('Ctrl Pts',(-3.62105896674335,31.9433378965044,-16.0978245265119));
#49737=CARTESIAN_POINT('Ctrl Pts',(-3.57590347039246,31.8547544475763,-16.1079243360576));
#49738=CARTESIAN_POINT('Ctrl Pts',(-3.52937024609825,31.7668908548368,-16.1181138393795));
#49739=CARTESIAN_POINT('Ctrl Pts',(-3.47886458044885,31.6715265360095,-16.1291731987021));
#49740=CARTESIAN_POINT('Ctrl Pts',(-3.42674093229675,31.5770072074372,-16.1403371547359));
#49741=CARTESIAN_POINT('Ctrl Pts',(-3.37289884216362,31.4833818651279,-16.1515805667539));
#49742=CARTESIAN_POINT('Ctrl Pts',(-3.36814188911558,31.4751100585103,-16.1525739231213));
#49743=CARTESIAN_POINT('Ctrl Pts',(-3.36337150087235,31.4668452394032,-16.1535679037735));
#49744=CARTESIAN_POINT('Ctrl Pts',(-3.35858762166542,31.458587434145,-16.1545624882756));
#49745=CARTESIAN_POINT('Ctrl Pts',(-3.30922464408307,31.3733783730022,-16.1648252165673));
#49746=CARTESIAN_POINT('Ctrl Pts',(-3.25842773463224,31.2889149064325,-16.1751525710054));
#49747=CARTESIAN_POINT('Ctrl Pts',(-3.2060976538235,31.2052454585662,-16.1855186131939));
#49748=CARTESIAN_POINT('Ctrl Pts',(-3.14869614503902,31.1134674128902,-16.1968892522708));
#49749=CARTESIAN_POINT('Ctrl Pts',(-3.08945202646307,31.0226435126636,-16.2083061104488));
#49750=CARTESIAN_POINT('Ctrl Pts',(-3.02820866784305,30.9328511554004,-16.2197396641263));
#49751=CARTESIAN_POINT('Ctrl Pts',(-3.02242456920364,30.9243707607392,-16.2208195004344));
#49752=CARTESIAN_POINT('Ctrl Pts',(-3.01662265581845,30.9158995510215,-16.2218994815536));
#49753=CARTESIAN_POINT('Ctrl Pts',(-3.01080281003991,30.9074375841179,-16.2229795795674));
#49754=CARTESIAN_POINT('Ctrl Pts',(-2.98581172706806,30.8711009310451,-16.2276176438924));
#49755=CARTESIAN_POINT('Ctrl Pts',(-2.96048834229123,30.8349355875039,-16.2322576875713));
#49756=CARTESIAN_POINT('Ctrl Pts',(-2.93482032948862,30.7989477238023,-16.2368971724292));
#49757=CARTESIAN_POINT('Ctrl Pts',(-2.92878548427683,30.7904865628775,-16.2379879687131));
#49758=CARTESIAN_POINT('Ctrl Pts',(-2.92273189589887,30.7820356435058,-16.2390786786312));
#49759=CARTESIAN_POINT('Ctrl Pts',(-2.91665928180757,30.7735948754177,-16.2401692920316));
#49760=CARTESIAN_POINT('Ctrl Pts',(-2.90681011979196,30.7599048086383,-16.2419381559698));
#49761=CARTESIAN_POINT('Ctrl Pts',(-2.89690782743331,30.7462374756054,-16.2437072886243));
#49762=CARTESIAN_POINT('Ctrl Pts',(-2.88695587177166,30.7325987650693,-16.245475820514));
#49763=CARTESIAN_POINT('Ctrl Pts',(-2.87316387298446,30.7136974470201,-16.2479267548334));
#49764=CARTESIAN_POINT('Ctrl Pts',(-2.85926885064398,30.6948407452796,-16.2503778818989));
#49765=CARTESIAN_POINT('Ctrl Pts',(-2.84529346740514,30.6760627734517,-16.2528244967358));
#49766=CARTESIAN_POINT('Ctrl Pts',(-2.83670886235749,30.6645281007359,-16.2543273694456));
#49767=CARTESIAN_POINT('Ctrl Pts',(-2.8280939989724,30.6530231651964,-16.2558285338661));
#49768=CARTESIAN_POINT('Ctrl Pts',(-2.81944868233181,30.6415484901895,-16.25732785939));
#49769=CARTESIAN_POINT('Ctrl Pts',(-2.76008246856886,30.5627534572668,-16.2676235238816));
#49770=CARTESIAN_POINT('Ctrl Pts',(-2.69925511842709,30.485339208081,-16.2778382567112));
#49771=CARTESIAN_POINT('Ctrl Pts',(-2.6368786599195,30.4094009767723,-16.2879363792964));
#49772=CARTESIAN_POINT('Ctrl Pts',(-2.63023927738889,30.401318072125,-16.2890112286913));
#49773=CARTESIAN_POINT('Ctrl Pts',(-2.62358231505887,30.3932518634772,-16.2900847614957));
#49774=CARTESIAN_POINT('Ctrl Pts',(-2.61690765823121,30.3852024536947,-16.2911569358438));
#49775=CARTESIAN_POINT('Ctrl Pts',(-2.55421731869184,30.3096000301712,-16.3012271125835));
#49776=CARTESIAN_POINT('Ctrl Pts',(-2.48996657427221,30.235479034662,-16.3111775693049));
#49777=CARTESIAN_POINT('Ctrl Pts',(-2.42403719691135,30.1629475728087,-16.3209694678104));
#49778=CARTESIAN_POINT('Ctrl Pts',(-2.41710390456308,30.1553199893307,-16.3219992074758));
#49779=CARTESIAN_POINT('Ctrl Pts',(-2.4101520341043,30.1477100003574,-16.3230271951822));
#49780=CARTESIAN_POINT('Ctrl Pts',(-2.4031814467617,30.1401177313289,-16.3240533855394));
#49781=CARTESIAN_POINT('Ctrl Pts',(-2.33681073803165,30.0678276571174,-16.3338242955004));
#49782=CARTESIAN_POINT('Ctrl Pts',(-2.26874390704782,29.9971433717163,-16.3434324167189));
#49783=CARTESIAN_POINT('Ctrl Pts',(-2.19883107131641,29.9282027371753,-16.3528328671236));
#49784=CARTESIAN_POINT('Ctrl Pts',(-2.19169909020464,29.921169932709,-16.3537918302958));
#49785=CARTESIAN_POINT('Ctrl Pts',(-2.18454788062778,29.9141552916404,-16.3547486341427));
#49786=CARTESIAN_POINT('Ctrl Pts',(-2.17737728168134,29.907158960102,-16.3557032307762));
#49787=CARTESIAN_POINT('Ctrl Pts',(-2.10687412725336,29.8383692471976,-16.3650890679102));
#49788=CARTESIAN_POINT('Ctrl Pts',(-2.03449764061465,29.7713485484957,-16.3742617525935));
#49789=CARTESIAN_POINT('Ctrl Pts',(-1.96005442350431,29.7062754434188,-16.3831678162274));
#49790=CARTESIAN_POINT('Ctrl Pts',(-1.95284479178456,29.6999732826488,-16.3840303452981));
#49791=CARTESIAN_POINT('Ctrl Pts',(-1.94561575396493,29.6936894074568,-16.3848903754564));
#49792=CARTESIAN_POINT('Ctrl Pts',(-1.93836713178303,29.6874239810535,-16.3857478578924));
#49793=CARTESIAN_POINT('Ctrl Pts',(-1.9043867100566,29.6580526293483,-16.3897676031715));
#49794=CARTESIAN_POINT('Ctrl Pts',(-1.86997530945131,29.6290872976276,-16.3937312402185));
#49795=CARTESIAN_POINT('Ctrl Pts',(-1.8351109162149,29.6005483948712,-16.3976330052129));
#49796=CARTESIAN_POINT('Ctrl Pts',(-1.82791828155379,29.5946607289145,-16.3984379516793));
#49797=CARTESIAN_POINT('Ctrl Pts',(-1.82070636560761,29.5887912119688,-16.3992402648017));
#49798=CARTESIAN_POINT('Ctrl Pts',(-1.8134749722379,29.5829400248555,-16.4000398940084));
#49799=CARTESIAN_POINT('Ctrl Pts',(-1.79944159999906,29.5715851057407,-16.4015916688514));
#49800=CARTESIAN_POINT('Ctrl Pts',(-1.78533484467896,29.5602992475422,-16.4031333296018));
#49801=CARTESIAN_POINT('Ctrl Pts',(-1.77115313127047,29.5490839118721,-16.4046644777802));
#49802=CARTESIAN_POINT('Ctrl Pts',(-1.76398520072988,29.5434152916738,-16.4054383732521));
#49803=CARTESIAN_POINT('Ctrl Pts',(-1.75679804992629,29.5377646410318,-16.4062095906596));
#49804=CARTESIAN_POINT('Ctrl Pts',(-1.74959177812074,29.5321323688344,-16.406978046244));
#49805=CARTESIAN_POINT('Ctrl Pts',(-1.74599580265247,29.5293218291823,-16.4073615104685));
#49806=CARTESIAN_POINT('Ctrl Pts',(-1.74239474124608,29.5265156339911,-16.407744318411));
#49807=CARTESIAN_POINT('Ctrl Pts',(-1.73878901023859,29.5237141339682,-16.4081264187999));
#49808=CARTESIAN_POINT('Ctrl Pts',(-1.72795745749596,29.5152984770063,-16.4092742416704));
#49809=CARTESIAN_POINT('Ctrl Pts',(-1.71707771413516,29.5069205819797,-16.4104163140041));
#49810=CARTESIAN_POINT('Ctrl Pts',(-1.70617071975849,29.4985974823528,-16.4115502304429));
#49811=CARTESIAN_POINT('Ctrl Pts',(-1.69904772283669,29.4931619415451,-16.4122907537277));
#49812=CARTESIAN_POINT('Ctrl Pts',(-1.69191078376265,29.4877479656186,-16.4130280427508));
#49813=CARTESIAN_POINT('Ctrl Pts',(-1.68476277503216,29.4823580137381,-16.413761738001));
#49814=CARTESIAN_POINT('Ctrl Pts',(-1.60434843675212,29.4217216281141,-16.422015731563));
#49815=CARTESIAN_POINT('Ctrl Pts',(-1.52231566709107,29.3639460194625,-16.4298395576141));
#49816=CARTESIAN_POINT('Ctrl Pts',(-1.43855993631844,29.309244218134,-16.4371696403728));
#49817=CARTESIAN_POINT('Ctrl Pts',(-1.43185569577448,29.3048656039077,-16.4377563779914));
#49818=CARTESIAN_POINT('Ctrl Pts',(-1.42514038609923,29.3005066777212,-16.4383399545619));
#49819=CARTESIAN_POINT('Ctrl Pts',(-1.41841394664406,29.2961675441765,-16.4389203379045));
#49820=CARTESIAN_POINT('Ctrl Pts',(-1.33363764949706,29.2414795213092,-16.446235166357));
#49821=CARTESIAN_POINT('Ctrl Pts',(-1.24709418954388,29.1899341559574,-16.4530430363004));
#49822=CARTESIAN_POINT('Ctrl Pts',(-1.1586319078417,29.1417972150289,-16.4592701105399));
#49823=CARTESIAN_POINT('Ctrl Pts',(-1.15256807669246,29.1384975682617,-16.4596969582994));
#49824=CARTESIAN_POINT('Ctrl Pts',(-1.14649522370832,29.135213947848,-16.4601210769962));
#49825=CARTESIAN_POINT('Ctrl Pts',(-1.14041329917068,29.1319464398898,-16.4605424426742));
#49826=CARTESIAN_POINT('Ctrl Pts',(-1.05072914523714,29.08376371666,-16.4667559075235));
#49827=CARTESIAN_POINT('Ctrl Pts',(-0.959073575743241,29.0390825445539,
-16.4723711392616));
#49828=CARTESIAN_POINT('Ctrl Pts',(-0.865245924595666,28.9982558106099,
-16.4772980159103));
#49829=CARTESIAN_POINT('Ctrl Pts',(-0.860089178972269,28.9960119829215,
-16.4775687958913));
#49830=CARTESIAN_POINT('Ctrl Pts',(-0.854925867180395,28.993779805817,-16.4778374964889));
#49831=CARTESIAN_POINT('Ctrl Pts',(-0.849755955267688,28.9915593384622,
-16.4781041026111));
#49832=CARTESIAN_POINT('Ctrl Pts',(-0.804702679736403,28.9722090421252,
-16.4804274456939));
#49833=CARTESIAN_POINT('Ctrl Pts',(-0.75914754240204,28.9537492095873,-16.4825915232));
#49834=CARTESIAN_POINT('Ctrl Pts',(-0.713063751488599,28.9362270883398,
-16.4845849257675));
#49835=CARTESIAN_POINT('Ctrl Pts',(-0.708478823168634,28.9344837927397,
-16.4847832516367));
#49836=CARTESIAN_POINT('Ctrl Pts',(-0.70388866133402,28.9327497797321,-16.4849798880179));
#49837=CARTESIAN_POINT('Ctrl Pts',(-0.69929323933093,28.9310250960911,-16.4851748236235));
#49838=CARTESIAN_POINT('Ctrl Pts',(-0.678143895164944,28.9230876470659,
-16.4860719686978));
#49839=CARTESIAN_POINT('Ctrl Pts',(-0.656883093495827,28.9153478825059,
-16.4869330756139));
#49840=CARTESIAN_POINT('Ctrl Pts',(-0.635507985977491,28.9078108306764,
-16.4877569613718));
#49841=CARTESIAN_POINT('Ctrl Pts',(-0.63124304224397,28.9063069738213,-16.4879213500841));
#49842=CARTESIAN_POINT('Ctrl Pts',(-0.626972842998408,28.9048109407091,
-16.4880842839842));
#49843=CARTESIAN_POINT('Ctrl Pts',(-0.62269785080394,28.9033229476927,-16.4882457340556));
#49844=CARTESIAN_POINT('Ctrl Pts',(-0.613932398969694,28.9002719640835,
-16.4885767715781));
#49845=CARTESIAN_POINT('Ctrl Pts',(-0.605154698954826,28.8972576033564,
-16.4889012600577));
#49846=CARTESIAN_POINT('Ctrl Pts',(-0.596371069871043,28.8942821068495,
-16.4892189364782));
#49847=CARTESIAN_POINT('Ctrl Pts',(-0.583303583379525,28.8898554330865,
-16.4896915466365));
#49848=CARTESIAN_POINT('Ctrl Pts',(-0.570221669843387,28.8855142735489,
-16.4901491375182));
#49849=CARTESIAN_POINT('Ctrl Pts',(-0.557125252287434,28.8812589290143,
-16.4905916000266));
#49850=CARTESIAN_POINT('Ctrl Pts',(-0.553224477579142,28.8799914724549,
-16.4907233877124));
#49851=CARTESIAN_POINT('Ctrl Pts',(-0.549322575762975,28.878731683996,-16.4908538273979));
#49852=CARTESIAN_POINT('Ctrl Pts',(-0.54541973243481,28.8774796356626,-16.4909829093196));
#49853=CARTESIAN_POINT('Ctrl Pts',(-0.444495674024695,28.84510277897,-16.4943208530454));
#49854=CARTESIAN_POINT('Ctrl Pts',(-0.342684747792481,28.8178087937562,
-16.4967606885858));
#49855=CARTESIAN_POINT('Ctrl Pts',(-0.240003537932831,28.7957518568242,
-16.4982544020511));
#49856=CARTESIAN_POINT('Ctrl Pts',(-0.237697811381644,28.7952565640126,
-16.4982879436777));
#49857=CARTESIAN_POINT('Ctrl Pts',(-0.235391639040659,28.794763909971,-16.4983210084487));
#49858=CARTESIAN_POINT('Ctrl Pts',(-0.233085020630584,28.7942738963076,
-16.4983535958337));
#49859=CARTESIAN_POINT('Ctrl Pts',(-0.155894242168747,28.7778756329573,
-16.4994441297518));
#49860=CARTESIAN_POINT('Ctrl Pts',(-0.0782039614584423,28.7644340236271,
-16.5000000902602));
#49861=CARTESIAN_POINT('Ctrl Pts',(3.88757237512749E-9,28.7540327056371,
-16.5000000412986));
#49862=CARTESIAN_POINT('',(-14.1696709099308,34.2228423342584,-8.45401836163377));
#49863=CARTESIAN_POINT('',(-14.1707043820172,35.7980733340469,8.45228604811576));
#49864=CARTESIAN_POINT('Ctrl Pts',(-14.1696709108715,34.2228423340475,-8.45401836462826));
#49865=CARTESIAN_POINT('Ctrl Pts',(-14.1695741904026,34.2248260380075,-8.45418047729493));
#49866=CARTESIAN_POINT('Ctrl Pts',(-14.169477830921,34.2268099148952,-8.45434197865485));
#49867=CARTESIAN_POINT('Ctrl Pts',(-14.167608911444,34.2654359276817,-8.45747422402139));
#49868=CARTESIAN_POINT('Ctrl Pts',(-14.1626664930993,34.3753969946356,-8.46575106737457));
#49869=CARTESIAN_POINT('Ctrl Pts',(-14.1563166525676,34.5588412605337,-8.47636383845025));
#49870=CARTESIAN_POINT('Ctrl Pts',(-14.1524973100839,34.7425201713618,-8.48273692051302));
#49871=CARTESIAN_POINT('Ctrl Pts',(-14.1511586618951,34.8712188614352,-8.48496958670444));
#49872=CARTESIAN_POINT('Ctrl Pts',(-14.1507878943851,34.9424970014783,-8.48558789977024));
#49873=CARTESIAN_POINT('Ctrl Pts',(-14.1507205812306,34.9769967825266,-8.4857001495824));
#49874=CARTESIAN_POINT('Ctrl Pts',(-14.1507126030543,34.9953992459202,-8.48571345413946));
#49875=CARTESIAN_POINT('Ctrl Pts',(-14.1507121043863,34.997705283278,-8.48571428571428));
#49876=CARTESIAN_POINT('Ctrl Pts',(-14.1507121010036,35.1468618614601,-8.48571420142721));
#49877=CARTESIAN_POINT('Ctrl Pts',(-14.1547776737579,35.4396107102406,-8.47893997864034));
#49878=CARTESIAN_POINT('Ctrl Pts',(-14.1728180804027,35.8758599754905,-8.44878247473178));
#49879=CARTESIAN_POINT('Ctrl Pts',(-14.2025224731818,36.3092714765184,-8.39880582800272));
#49880=CARTESIAN_POINT('Ctrl Pts',(-14.2299007195476,36.5963355642442,-8.35229744786236));
#49881=CARTESIAN_POINT('Ctrl Pts',(-14.2531943877412,36.810931871133,-8.31244167087513));
#49882=CARTESIAN_POINT('Ctrl Pts',(-14.2614188842623,36.8823469768069,-8.29832695019776));
#49883=CARTESIAN_POINT('Ctrl Pts',(-14.2744349428304,36.9892940609228,-8.27590368202145));
#49884=CARTESIAN_POINT('Ctrl Pts',(-14.2788886842903,37.0249272832859,-8.26821750742406));
#49885=CARTESIAN_POINT('Ctrl Pts',(-14.2879999806155,37.0959766543479,-8.25246271795894));
#49886=CARTESIAN_POINT('Ctrl Pts',(-14.3112981066859,37.2731437910936,-8.21210092185544));
#49887=CARTESIAN_POINT('Ctrl Pts',(-14.3578215203792,37.5879814951676,-8.13074614008949));
#49888=CARTESIAN_POINT('Ctrl Pts',(-14.4288904455033,37.9993760199721,-8.00406949270557));
#49889=CARTESIAN_POINT('Ctrl Pts',(-14.5082755714546,38.4025980690195,-7.85939563929309));
#49890=CARTESIAN_POINT('Ctrl Pts',(-14.5952758192465,38.7978060707092,-7.69678192603311));
#49891=CARTESIAN_POINT('Ctrl Pts',(-14.657896478309,39.0560030253266,-7.57635264543442));
#49892=CARTESIAN_POINT('Ctrl Pts',(-14.7064265059084,39.24768357466,-7.48146252884525));
#49893=CARTESIAN_POINT('Ctrl Pts',(-14.7228639638505,39.3112490789017,-7.44907072917455));
#49894=CARTESIAN_POINT('Ctrl Pts',(-14.7437193986859,39.3902959250722,-7.40761934898492));
#49895=CARTESIAN_POINT('Ctrl Pts',(-14.7479070967605,39.4060891979786,-7.39927862261931));
#49896=CARTESIAN_POINT('Ctrl Pts',(-14.7563048500418,39.43760451593,-7.38251685050611));
#49897=CARTESIAN_POINT('Ctrl Pts',(-14.7689360904756,39.4847752253455,-7.35725166419566));
#49898=CARTESIAN_POINT('Ctrl Pts',(-14.8156233275035,39.6566118128767,-7.26326438367064));
#49899=CARTESIAN_POINT('Ctrl Pts',(-14.8939488036773,39.9317377406937,-7.10215132097504));
#49900=CARTESIAN_POINT('Ctrl Pts',(-15.0016811570264,40.2860018252939,-6.87185639159196));
#49901=CARTESIAN_POINT('Ctrl Pts',(-15.1119376754938,40.6279408023941,-6.62607667302398));
#49902=CARTESIAN_POINT('Ctrl Pts',(-15.2239734404578,40.9576909989467,-6.36467091771852));
#49903=CARTESIAN_POINT('Ctrl Pts',(-15.3370614584757,41.2752810389499,-6.08736076314172));
#49904=CARTESIAN_POINT('Ctrl Pts',(-15.4126756708071,41.4788475427847,-5.89160359585481));
#49905=CARTESIAN_POINT('Ctrl Pts',(-15.4551351348553,41.5910215779799,-5.77831974861222));
#49906=CARTESIAN_POINT('Ctrl Pts',(-15.4645714783246,41.6158920116934,-5.75304936459231));
#49907=CARTESIAN_POINT('Ctrl Pts',(-15.4833976826855,41.6652775253122,-5.7022525407896));
#49908=CARTESIAN_POINT('Ctrl Pts',(-15.5162167852146,41.750772105944,-5.61268646577723));
#49909=CARTESIAN_POINT('Ctrl Pts',(-15.5813109712958,41.9180543172635,-5.43086629761845));
#49910=CARTESIAN_POINT('Ctrl Pts',(-15.6725353902666,42.1465300010458,-5.16344533267769));
#49911=CARTESIAN_POINT('Ctrl Pts',(-15.7785163448955,42.4040407988642,-4.83016097008632));
#49912=CARTESIAN_POINT('Ctrl Pts',(-15.8803551407113,42.6448820262437,-4.48430381136062));
#49913=CARTESIAN_POINT('Ctrl Pts',(-15.9773923092272,42.8688955481545,-4.1255771403933));
#49914=CARTESIAN_POINT('Ctrl Pts',(-16.0689491798707,43.0757670031137,-3.75357202254097));
#49915=CARTESIAN_POINT('Ctrl Pts',(-16.1258601163662,43.20193282153,-3.49636194469719));
#49916=CARTESIAN_POINT('Ctrl Pts',(-16.15656884454,43.26947017561,-3.34896447224242));
#49917=CARTESIAN_POINT('Ctrl Pts',(-16.1599628057576,43.2769266297891,-3.33254920768214));
#49918=CARTESIAN_POINT('Ctrl Pts',(-16.1667141577056,43.2917440522527,-3.29964186034883));
#49919=CARTESIAN_POINT('Ctrl Pts',(-16.1767895284817,43.3138339314586,-3.25014873591082));
#49920=CARTESIAN_POINT('Ctrl Pts',(-16.1998163579052,43.3641659816838,-3.13431622756455));
#49921=CARTESIAN_POINT('Ctrl Pts',(-16.2439213376448,43.4599998483849,-2.90125815378974));
#49922=CARTESIAN_POINT('Ctrl Pts',(-16.3012520736682,43.583202117882,-2.56434909920735));
#49923=CARTESIAN_POINT('Ctrl Pts',(-16.3606131885796,43.7092439393456,-2.15369772581687));
#49924=CARTESIAN_POINT('Ctrl Pts',(-16.4101690918599,43.8134316244425,-1.73663080953923));
#49925=CARTESIAN_POINT('Ctrl Pts',(-16.4495298899743,43.8955368530516,-1.3130485431318));
#49926=CARTESIAN_POINT('Ctrl Pts',(-16.4782739255189,43.9551426541823,-0.882801768751853));
#49927=CARTESIAN_POINT('Ctrl Pts',(-16.4900529536379,43.979471812853,-0.591393704480866));
#49928=CARTESIAN_POINT('Ctrl Pts',(-16.4950012451008,43.9896869433472,-0.40777871706539));
#49929=CARTESIAN_POINT('Ctrl Pts',(-16.4958675714987,43.9914748615063,-0.37107635173854));
#49930=CARTESIAN_POINT('Ctrl Pts',(-16.497353950166,43.9945419809135,-0.297753965897757));
#49931=CARTESIAN_POINT('Ctrl Pts',(-16.4992147466688,43.9983812928445,-0.187873401187913));
#49932=CARTESIAN_POINT('Ctrl Pts',(-16.5009893405106,44.002039303395,0.0677974336874361));
#49933=CARTESIAN_POINT('Ctrl Pts',(-16.4962759179933,43.9923237789446,0.431019295927046));
#49934=CARTESIAN_POINT('Ctrl Pts',(-16.4792634221366,43.9571888216067,0.863709911301573));
#49935=CARTESIAN_POINT('Ctrl Pts',(-16.4511064396992,43.8988136250866,1.29326197944579));
#49936=CARTESIAN_POINT('Ctrl Pts',(-16.4119922180881,43.8172491800175,1.71969094578633));
#49937=CARTESIAN_POINT('Ctrl Pts',(-16.3787219461102,43.7473246837639,2.00189093332564));
#49938=CARTESIAN_POINT('Ctrl Pts',(-16.3580119895428,43.7035584097628,2.16003652998315));
#49939=CARTESIAN_POINT('Ctrl Pts',(-16.3556824478205,43.6986323471244,2.17760524249224));
#49940=CARTESIAN_POINT('Ctrl Pts',(-16.3509756164775,43.6886727745913,2.21267018387781));
#49941=CARTESIAN_POINT('Ctrl Pts',(-16.3438414997254,43.6735675177399,2.26517652860798));
#49942=CARTESIAN_POINT('Ctrl Pts',(-16.326683133664,43.6371667634837,2.38705769395721));
#49943=CARTESIAN_POINT('Ctrl Pts',(-16.2903559198775,43.5597844011501,2.62831145762857));
#49944=CARTESIAN_POINT('Ctrl Pts',(-16.232934747708,43.4363948317854,2.96594942969864));
#49945=CARTESIAN_POINT('Ctrl Pts',(-16.1558369125918,43.2683468686933,3.36029215003981));
#49946=CARTESIAN_POINT('Ctrl Pts',(-16.0711547872304,43.0806970112392,3.74411043194686));
#49947=CARTESIAN_POINT('Ctrl Pts',(-16.0100316917562,42.9426649113339,3.99311497871483));
#49948=CARTESIAN_POINT('Ctrl Pts',(-15.9625807951282,42.834300206208,4.17732388737971));
#49949=CARTESIAN_POINT('Ctrl Pts',(-15.9464957088409,42.7973714327389,4.23830257009782));
#49950=CARTESIAN_POINT('Ctrl Pts',(-15.9138128435039,42.7218957411724,4.35941450767284));
#49951=CARTESIAN_POINT('Ctrl Pts',(-15.8972125272316,42.6833429047006,4.41955673988955));
#49952=CARTESIAN_POINT('Ctrl Pts',(-15.8466933704575,42.5652823224171,4.59866294426839));
#49953=CARTESIAN_POINT('Ctrl Pts',(-15.7779234599878,42.402642077536,4.83217499176075));
#49954=CARTESIAN_POINT('Ctrl Pts',(-15.6712884768364,42.143462768174,5.16724219532538));
#49955=CARTESIAN_POINT('Ctrl Pts',(-15.5618951178217,41.8693647418838,5.48763911494565));
#49956=CARTESIAN_POINT('Ctrl Pts',(-15.4504486904824,41.5805039812304,5.7937581096588));
#49957=CARTESIAN_POINT('Ctrl Pts',(-15.3376532680843,41.2769000449641,6.08586586123047));
#49958=CARTESIAN_POINT('Ctrl Pts',(-15.2620320937449,41.0645933577144,6.27136226359692));
#49959=CARTESIAN_POINT('Ctrl Pts',(-15.2053415900942,40.90158680001,6.40702654875819));
#49960=CARTESIAN_POINT('Ctrl Pts',(-15.1864463821522,40.846613607407,6.45167758566546));
#49961=CARTESIAN_POINT('Ctrl Pts',(-15.1487072597771,40.7354250324889,6.53979899832712));
#49962=CARTESIAN_POINT('Ctrl Pts',(-15.0923703091726,40.5673516835224,6.66975320244555));
#49963=CARTESIAN_POINT('Ctrl Pts',(-15.0000554476411,40.2808283698595,6.87540602054584));
#49964=CARTESIAN_POINT('Ctrl Pts',(-14.8925110399882,39.9268221531973,7.10514982298711));
#49965=CARTESIAN_POINT('Ctrl Pts',(-14.7889128746132,39.5626135550613,7.318157904284));
#49966=CARTESIAN_POINT('Ctrl Pts',(-14.6899912137661,39.1880940439612,7.51458827196825));
#49967=CARTESIAN_POINT('Ctrl Pts',(-14.5965014824253,38.8030707992935,7.69445703548796));
#49968=CARTESIAN_POINT('Ctrl Pts',(-14.538322404446,38.5391996458362,7.80324419207337));
#49969=CARTESIAN_POINT('Ctrl Pts',(-14.4964515165695,38.3385070734916,7.88059344160958));
#49970=CARTESIAN_POINT('Ctrl Pts',(-14.4759570917779,38.2374631441761,7.91820724260092));
#49971=CARTESIAN_POINT('Ctrl Pts',(-14.4561651015489,38.135351554819,7.95421100845906));
#49972=CARTESIAN_POINT('Ctrl Pts',(-14.4431311948623,38.0670373384614,7.9778533139139));
#49973=CARTESIAN_POINT('Ctrl Pts',(-14.4367073731516,38.0328270049686,7.98947122579105));
#49974=CARTESIAN_POINT('Ctrl Pts',(-14.4050727916094,37.8615760883448,8.04652731310212));
#49975=CARTESIAN_POINT('Ctrl Pts',(-14.3575320825755,37.586160463065,8.13125547960728));
#49976=CARTESIAN_POINT('Ctrl Pts',(-14.2959116329745,37.1688066236194,8.23900264520774));
#49977=CARTESIAN_POINT('Ctrl Pts',(-14.2444368705164,36.7472097164333,8.32759190579159));
#49978=CARTESIAN_POINT('Ctrl Pts',(-14.2035511453535,36.3213337431343,8.39706625486179));
#49979=CARTESIAN_POINT('Ctrl Pts',(-14.1815181263396,36.0039451620904,8.43414643534559));
#49980=CARTESIAN_POINT('Ctrl Pts',(-14.1722466100885,35.8288769445023,8.44970037933995));
#49981=CARTESIAN_POINT('Ctrl Pts',(-14.170704401996,35.7980733355909,8.4522860773754));
#49982=CARTESIAN_POINT('Ctrl Pts',(-14.170704401996,35.7980733355909,8.4522860773754));
#49983=CARTESIAN_POINT('Ctrl Pts',(-14.1650142937913,35.684420795022,8.46182623066452));
#49984=CARTESIAN_POINT('Ctrl Pts',(-14.1605133003307,35.5703099692951,8.46935085018393));
#49985=CARTESIAN_POINT('Ctrl Pts',(-14.1551506650199,35.382916204612,8.47830915393529));
#49986=CARTESIAN_POINT('Ctrl Pts',(-14.1527653559365,35.2734091961459,8.4822897541675));
#49987=CARTESIAN_POINT('Ctrl Pts',(-14.1512998321667,35.1451489583981,8.48473414715993));
#49988=CARTESIAN_POINT('Ctrl Pts',(-14.1509563381337,35.0900718984593,8.4853069916253));
#49989=CARTESIAN_POINT('Ctrl Pts',(-14.1507908381907,35.0533296802779,8.48558298996998));
#49990=CARTESIAN_POINT('Ctrl Pts',(-14.1507398452452,35.0349424468843,8.48566802518057));
#49991=CARTESIAN_POINT('Ctrl Pts',(-14.1505677273441,34.8695234717906,8.48595504833412));
#49992=CARTESIAN_POINT('Ctrl Pts',(-14.154337784268,34.5758999514473,8.47967359793947));
#49993=CARTESIAN_POINT('Ctrl Pts',(-14.1661751055454,34.2831792944904,8.45988898246179));
#49994=CARTESIAN_POINT('Ctrl Pts',(-14.1760617772299,34.1005103374036,8.44329837255236));
#49995=CARTESIAN_POINT('Ctrl Pts',(-14.1781635049883,34.0639906238477,8.43976886981633));
#49996=CARTESIAN_POINT('Ctrl Pts',(-14.1826148355227,33.9909793560335,8.43228648572353));
#49997=CARTESIAN_POINT('Ctrl Pts',(-14.1849621036091,33.9545270470129,8.42833752540023));
#49998=CARTESIAN_POINT('Ctrl Pts',(-14.1923590999347,33.8454073291104,8.41588040125304));
#49999=CARTESIAN_POINT('Ctrl Pts',(-14.2085801409186,33.628016870901,8.38851135454656));
#50000=CARTESIAN_POINT('Ctrl Pts',(-14.242558876821,33.2698693265225,8.33080238485682));
#50001=CARTESIAN_POINT('Ctrl Pts',(-14.2938388156815,32.8465728575125,8.24259551333885));
#50002=CARTESIAN_POINT('Ctrl Pts',(-14.3550258803295,32.4296068752297,8.13567231318596));
#50003=CARTESIAN_POINT('Ctrl Pts',(-14.4255263377446,32.0188604564641,8.01012491229647));
#50004=CARTESIAN_POINT('Ctrl Pts',(-14.4783420074819,31.7491274305981,7.9139754325281));
#50005=CARTESIAN_POINT('Ctrl Pts',(-14.5199872681947,31.5483560263418,7.83714350637601));
#50006=CARTESIAN_POINT('Ctrl Pts',(-14.5413182793014,31.4483525564814,7.79754705060685));
#50007=CARTESIAN_POINT('Ctrl Pts',(-14.5670619058874,31.332350650325,7.74926761389229));
#50008=CARTESIAN_POINT('Ctrl Pts',(-14.5782751718068,31.2827789482509,7.72812768378482));
#50009=CARTESIAN_POINT('Ctrl Pts',(-14.5857903611018,31.2497630278683,7.71393440624095));
#50010=CARTESIAN_POINT('Ctrl Pts',(-14.5895683675641,31.2332685890218,7.70678667876997));
#50011=CARTESIAN_POINT('Ctrl Pts',(-14.6237041832346,31.0851485338514,7.64208780254395));
#50012=CARTESIAN_POINT('Ctrl Pts',(-14.6864314643324,30.8258800442836,7.52155237866732));
#50013=CARTESIAN_POINT('Ctrl Pts',(-14.7857914081875,30.4487285699288,7.3244688139282));
#50014=CARTESIAN_POINT('Ctrl Pts',(-14.8896130143424,30.083018389305,7.11122176429787));
#50015=CARTESIAN_POINT('Ctrl Pts',(-14.9971260006425,29.728539153092,6.88178661466567));
#50016=CARTESIAN_POINT('Ctrl Pts',(-15.107586973597,29.3851765976609,6.63599805956354));
#50017=CARTESIAN_POINT('Ctrl Pts',(-15.1827094430498,29.1636664722939,6.46103123524353));
#50018=CARTESIAN_POINT('Ctrl Pts',(-15.2299741428703,29.0275513750395,6.34810893285796));
#50019=CARTESIAN_POINT('Ctrl Pts',(-15.2441770407058,28.9868916238194,6.31396444350626));
#50020=CARTESIAN_POINT('Ctrl Pts',(-15.2584109480816,28.9464949026306,6.279414905448));
#50021=CARTESIAN_POINT('Ctrl Pts',(-15.2679066407198,28.9196223154397,6.25629147543193));
#50022=CARTESIAN_POINT('Ctrl Pts',(-15.2726590658456,28.9062114640805,6.24468119189695));
#50023=CARTESIAN_POINT('Ctrl Pts',(-15.2964106057722,28.8393748682971,6.18646540617525));
#50024=CARTESIAN_POINT('Ctrl Pts',(-15.3533459015535,28.6809698697406,6.04508845262122));
#50025=CARTESIAN_POINT('Ctrl Pts',(-15.4476616968562,28.4268496179288,5.80119143439749));
#50026=CARTESIAN_POINT('Ctrl Pts',(-15.5592063981134,28.137488294186,5.49524715128581));
#50027=CARTESIAN_POINT('Ctrl Pts',(-15.6684242436608,27.863613730649,5.17588769171355));
#50028=CARTESIAN_POINT('Ctrl Pts',(-15.7746293906152,27.605268899128,4.84285419679768));
#50029=CARTESIAN_POINT('Ctrl Pts',(-15.8771294623924,27.3626395384143,4.49576900414588));
#50030=CARTESIAN_POINT('Ctrl Pts',(-15.9425189610858,27.2115867611153,4.25467413754807));
#50031=CARTESIAN_POINT('Ctrl Pts',(-15.9823115556383,27.1206276984159,4.10082034672238));
#50032=CARTESIAN_POINT('Ctrl Pts',(-15.9941685918194,27.0935988642727,4.05442630335374));
#50033=CARTESIAN_POINT('Ctrl Pts',(-16.0058999460955,27.0669620086443,4.00767092629643));
#50034=CARTESIAN_POINT('Ctrl Pts',(-16.0136924049493,27.0492916411347,3.97641985931698));
#50035=CARTESIAN_POINT('Ctrl Pts',(-16.017575969199,27.0404967069963,3.96074757211319));
#50036=CARTESIAN_POINT('Ctrl Pts',(-16.0368989816428,26.9967922022051,3.88227417674093));
#50037=CARTESIAN_POINT('Ctrl Pts',(-16.0823546071933,26.8945220845182,3.69290418132499));
#50038=CARTESIAN_POINT('Ctrl Pts',(-16.1533708020943,26.7370711648309,3.37213089324311));
#50039=CARTESIAN_POINT('Ctrl Pts',(-16.2305392874646,26.5687922048503,2.97892631034643));
#50040=CARTESIAN_POINT('Ctrl Pts',(-16.2991865268191,26.4212105852304,2.5773593843556));
#50041=CARTESIAN_POINT('Ctrl Pts',(-16.358824265294,26.2945334961653,2.16728320804858));
#50042=CARTESIAN_POINT('Ctrl Pts',(-16.4089359242923,26.1891478876751,1.74848541072101));
#50043=CARTESIAN_POINT('Ctrl Pts',(-16.4356234117713,26.1334700430816,1.46328384430231));
#50044=CARTESIAN_POINT('Ctrl Pts',(-16.4500763362448,26.1033937085539,1.28308059592088));
#50045=CARTESIAN_POINT('Ctrl Pts',(-16.4542451349426,26.0947252636253,1.22887309433461));
#50046=CARTESIAN_POINT('Ctrl Pts',(-16.4581595150294,26.0865940893665,1.17444330933025));
#50047=CARTESIAN_POINT('Ctrl Pts',(-16.4607121333396,26.0812933526595,1.1381071005436));
#50048=CARTESIAN_POINT('Ctrl Pts',(-16.4619601679387,26.0787025731161,1.11991054911913));
#50049=CARTESIAN_POINT('Ctrl Pts',(-16.4680452940168,26.0660740197497,1.02898093092931));
#50050=CARTESIAN_POINT('Ctrl Pts',(-16.4811896615495,26.0388350482944,0.810850535778437));
#50051=CARTESIAN_POINT('Ctrl Pts',(-16.4958379451374,26.0085796010159,0.447797325416032));
#50052=CARTESIAN_POINT('Ctrl Pts',(-16.5019014985441,25.9960803480265,0.0129168588320056));
#50053=CARTESIAN_POINT('Ctrl Pts',(-16.4965250309543,26.0071624248857,-0.421187209207354));
#50054=CARTESIAN_POINT('Ctrl Pts',(-16.4797585463819,26.0417870836736,-0.854516554641816));
#50055=CARTESIAN_POINT('Ctrl Pts',(-16.4610052678583,26.0806622765574,-1.14288393942141));
#50056=CARTESIAN_POINT('Ctrl Pts',(-16.4441004623375,26.1158254145706,-1.35896266188989));
#50057=CARTESIAN_POINT('Ctrl Pts',(-16.4379921612025,26.1285480939795,-1.43095608567496));
#50058=CARTESIAN_POINT('Ctrl Pts',(-16.4281192689933,26.1491499157046,-1.53889658081771));
#50059=CARTESIAN_POINT('Ctrl Pts',(-16.4247074826621,26.1562752423396,-1.57489137072349));
#50060=CARTESIAN_POINT('Ctrl Pts',(-16.4176713964204,26.170983711353,-1.64662271617671));
#50061=CARTESIAN_POINT('Ctrl Pts',(-16.3995385050462,26.2089239746975,-1.82543046804099));
#50062=CARTESIAN_POINT('Ctrl Pts',(-16.3620990851254,26.2876142555016,-2.14265858582978));
#50063=CARTESIAN_POINT('Ctrl Pts',(-16.3025550756539,26.4140141772911,-2.55612272970656));
#50064=CARTESIAN_POINT('Ctrl Pts',(-16.2339549247019,26.5613987045783,-2.96035789316663));
#50065=CARTESIAN_POINT('Ctrl Pts',(-16.1568331540347,26.7294614056885,-3.35556685486244));
#50066=CARTESIAN_POINT('Ctrl Pts',(-16.1000779699745,26.8552023071255,-3.61311125493434));
#50067=CARTESIAN_POINT('Ctrl Pts',(-16.0556336481855,26.954656254176,-3.80406349187298));
#50068=CARTESIAN_POINT('Ctrl Pts',(-16.0405058631815,26.9886660670731,-3.86734639076527));
#50069=CARTESIAN_POINT('Ctrl Pts',(-16.0096449541652,27.0584100439092,-3.99317729314595));
#50070=CARTESIAN_POINT('Ctrl Pts',(-15.9939769145489,27.0939972209781,-4.05546016699478));
#50071=CARTESIAN_POINT('Ctrl Pts',(-15.946310486811,27.2028616000745,-4.24044728136714));
#50072=CARTESIAN_POINT('Ctrl Pts',(-15.8809887484904,27.3536214270733,-4.48214461280834));
#50073=CARTESIAN_POINT('Ctrl Pts',(-15.7784458744819,27.5961148460772,-4.83043553146742));
#50074=CARTESIAN_POINT('Ctrl Pts',(-15.672049918236,27.8546596157552,-5.1649326097885));
#50075=CARTESIAN_POINT('Ctrl Pts',(-15.5624916037538,28.129105638327,-5.48597264019887));
#50076=CARTESIAN_POINT('Ctrl Pts',(-15.4878021056829,28.3226667451366,-5.69117614490112));
#50077=CARTESIAN_POINT('Ctrl Pts',(-15.4313404408399,28.4718461710231,-5.84179828419061));
#50078=CARTESIAN_POINT('Ctrl Pts',(-15.4029985230074,28.5474385488685,-5.91628884328912));
#50079=CARTESIAN_POINT('Ctrl Pts',(-15.3745234531469,28.624546812136,-5.98954995183328));
#50080=CARTESIAN_POINT('Ctrl Pts',(-15.3602665579123,28.6633548051861,-6.025975545843));
#50081=CARTESIAN_POINT('Ctrl Pts',(-15.3555101033097,28.6763356770808,-6.03808558623429));
#50082=CARTESIAN_POINT('Ctrl Pts',(-15.3460025377012,28.7023511935678,-6.0622087309629));
#50083=CARTESIAN_POINT('Ctrl Pts',(-15.3032311621593,28.8196938948245,-6.17035454234009));
#50084=CARTESIAN_POINT('Ctrl Pts',(-15.2226957929703,29.0459577602373,-6.36774026416183));
#50085=CARTESIAN_POINT('Ctrl Pts',(-15.1103581436995,29.3768176414454,-6.62967969820033));
#50086=CARTESIAN_POINT('Ctrl Pts',(-15.0000982739845,29.7190541567933,-6.87530387810371));
#50087=CARTESIAN_POINT('Ctrl Pts',(-14.8926447051201,30.0727157868756,-7.10487256923306));
#50088=CARTESIAN_POINT('Ctrl Pts',(-14.7887465869561,30.4379496584912,-7.31850526348433));
#50089=CARTESIAN_POINT('Ctrl Pts',(-14.722370697791,30.6893179835201,-7.4502913611161));
#50090=CARTESIAN_POINT('Ctrl Pts',(-14.6738777071513,30.880887120718,-7.54510259159816));
#50091=CARTESIAN_POINT('Ctrl Pts',(-14.6499536034456,30.9774327980255,-7.59150060955208));
#50092=CARTESIAN_POINT('Ctrl Pts',(-14.622653427221,31.0914254884024,-7.643853266848));
#50093=CARTESIAN_POINT('Ctrl Pts',(-14.6110895157115,31.1405729393151,-7.66590707737604));
#50094=CARTESIAN_POINT('Ctrl Pts',(-14.603411082087,31.1734034467758,-7.68052426092624));
#50095=CARTESIAN_POINT('Ctrl Pts',(-14.5995879179982,31.1898488485157,-7.68778896006205));
#50096=CARTESIAN_POINT('Ctrl Pts',(-14.5653679358988,31.3379480621503,-7.75269682466588));
#50097=CARTESIAN_POINT('Ctrl Pts',(-14.5070489009751,31.6032252348347,-7.86166211779646));
#50098=CARTESIAN_POINT('Ctrl Pts',(-14.4276988699282,32.0070952985095,-8.00621338887606));
#50099=CARTESIAN_POINT('Ctrl Pts',(-14.3570548434617,32.4169446945395,-8.1320931910977));
#50100=CARTESIAN_POINT('Ctrl Pts',(-14.2956946457161,32.8328361476157,-8.23937842578888));
#50101=CARTESIAN_POINT('Ctrl Pts',(-14.244197923,33.2548692668906,-8.32800172692067));
#50102=CARTESIAN_POINT('Ctrl Pts',(-14.2031474640429,33.6831811080674,-8.39774998726108));
#50103=CARTESIAN_POINT('Ctrl Pts',(-14.1831359783168,33.9730252763557,-8.43142350436688));
#50104=CARTESIAN_POINT('Ctrl Pts',(-14.1731601462849,34.1535912512886,-8.44816816605938));
#50105=CARTESIAN_POINT('Ctrl Pts',(-14.1713604525151,34.1881904088942,-8.45118653281004));
#50106=CARTESIAN_POINT('Ctrl Pts',(-14.1696709108715,34.2228423340475,-8.45401836462826));
#50107=CARTESIAN_POINT('Origin',(3.06151588455592E-17,0.499999999999993,
3.46944695195362E-15));
#50108=CARTESIAN_POINT('',(-2.38806125833734E-15,0.,19.5));
#50109=CARTESIAN_POINT('Origin',(0.,0.,0.));
#50110=CARTESIAN_POINT('Origin',(-2.35744609949178E-15,0.5,19.5));
#50111=CARTESIAN_POINT('Origin',(33.,21.,6.));
#50112=CARTESIAN_POINT('',(17.4999100362558,20.3177785969023,1.04675962888699));
#50113=CARTESIAN_POINT('',(17.5000000502851,20.9999999999962,0.999999421609969));
#50114=CARTESIAN_POINT('Ctrl Pts',(17.4999100362569,20.3177788181702,1.04676123540741));
#50115=CARTESIAN_POINT('Ctrl Pts',(17.4999659873509,20.4233535518093,1.03222017995305));
#50116=CARTESIAN_POINT('Ctrl Pts',(17.5000024591585,20.6351868947168,1.00991574296543));
#50117=CARTESIAN_POINT('Ctrl Pts',(17.4999997636355,20.8632212238551,1.00054557418263));
#50118=CARTESIAN_POINT('Ctrl Pts',(17.5000000120934,20.9851040242355,0.999999990573371));
#50119=CARTESIAN_POINT('Ctrl Pts',(17.5000000502852,21.,0.999999889154119));
#50120=CARTESIAN_POINT('',(17.3583581903393,24.8843450507804,2.85168847095763));
#50121=CARTESIAN_POINT('Ctrl Pts',(17.500000050285,20.9999999999924,0.99999895406582));
#50122=CARTESIAN_POINT('Ctrl Pts',(17.5000002619754,21.0825658826246,0.99999828024815));
#50123=CARTESIAN_POINT('Ctrl Pts',(17.5000004475595,21.1653409669682,1.0020439175894));
#50124=CARTESIAN_POINT('Ctrl Pts',(17.4999984197852,21.2483205520721,1.00617011669214));
#50125=CARTESIAN_POINT('Ctrl Pts',(17.4999981845068,21.2579484979676,1.00664887085397));
#50126=CARTESIAN_POINT('Ctrl Pts',(17.4999979042424,21.2675796394476,1.00715570195213));
#50127=CARTESIAN_POINT('Ctrl Pts',(17.4999975660631,21.2772135619585,1.00769065856536));
#50128=CARTESIAN_POINT('Ctrl Pts',(17.499997093731,21.290669177815,1.00843782781851));
#50129=CARTESIAN_POINT('Ctrl Pts',(17.4999965176582,21.3041303303614,1.00923986594952));
#50130=CARTESIAN_POINT('Ctrl Pts',(17.4999958055237,21.3175970413969,1.01009698967317));
#50131=CARTESIAN_POINT('Ctrl Pts',(17.4999953686873,21.3258577686798,1.01062276506926));
#50132=CARTESIAN_POINT('Ctrl Pts',(17.4999948801857,21.3341206497865,1.01116927435963));
#50133=CARTESIAN_POINT('Ctrl Pts',(17.4999943324047,21.3423847863016,1.01173650875285));
#50134=CARTESIAN_POINT('Ctrl Pts',(17.4999939871881,21.3475929185825,1.01209398490886));
#50135=CARTESIAN_POINT('Ctrl Pts',(17.4999936185644,21.3527990326318,1.0124595168517));
#50136=CARTESIAN_POINT('Ctrl Pts',(17.4999932241172,21.3580029700491,1.01283307974399));
#50137=CARTESIAN_POINT('Ctrl Pts',(17.4999912418066,21.3841555660329,1.01471043502578));
#50138=CARTESIAN_POINT('Ctrl Pts',(17.4999886059075,21.4102591246994,1.01679104223432));
#50139=CARTESIAN_POINT('Ctrl Pts',(17.4999850036602,21.4363140115829,1.01907337101856));
#50140=CARTESIAN_POINT('Ctrl Pts',(17.4999774808885,21.4907258700469,1.02383968419932));
#50141=CARTESIAN_POINT('Ctrl Pts',(17.4999657632806,21.5449255028529,1.02948549995329));
#50142=CARTESIAN_POINT('Ctrl Pts',(17.4999465256887,21.5989157358221,1.0359995859063));
#50143=CARTESIAN_POINT('Ctrl Pts',(17.4999436734614,21.6069205014265,1.03696538524283));
#50144=CARTESIAN_POINT('Ctrl Pts',(17.4999406460128,21.614920660968,1.03795027054161));
#50145=CARTESIAN_POINT('Ctrl Pts',(17.4999374319906,21.6229162233955,1.03895420514678));
#50146=CARTESIAN_POINT('Ctrl Pts',(17.4998979018249,21.7212559003615,1.05130187995543));
#50147=CARTESIAN_POINT('Ctrl Pts',(17.4998312965506,21.8189008936684,1.06652816328134));
#50148=CARTESIAN_POINT('Ctrl Pts',(17.49970544906,21.9158605146828,1.0845951504899));
#50149=CARTESIAN_POINT('Ctrl Pts',(17.4996728061027,21.9410103905533,1.08928145681923));
#50150=CARTESIAN_POINT('Ctrl Pts',(17.4996360623702,21.9661141374527,1.09415888464573));
#50151=CARTESIAN_POINT('Ctrl Pts',(17.4995946625124,21.9911719148272,1.09922677169631));
#50152=CARTESIAN_POINT('Ctrl Pts',(17.4994634776476,22.070573181148,1.11528552436911));
#50153=CARTESIAN_POINT('Ctrl Pts',(17.4992855829644,22.1495128532391,1.13325673599016));
#50154=CARTESIAN_POINT('Ctrl Pts',(17.4990350181115,22.2279909063928,1.15314037837427));
#50155=CARTESIAN_POINT('Ctrl Pts',(17.4989016549127,22.2697608676562,1.16372345146011));
#50156=CARTESIAN_POINT('Ctrl Pts',(17.4987473922076,22.3114000537755,1.17484829718504));
#50157=CARTESIAN_POINT('Ctrl Pts',(17.4985682696136,22.3529084437789,1.18651490676946));
#50158=CARTESIAN_POINT('Ctrl Pts',(17.4983046477483,22.4139979967894,1.20368512138396));
#50159=CARTESIAN_POINT('Ctrl Pts',(17.4979872508062,22.4748042561263,1.22202875240462));
#50160=CARTESIAN_POINT('Ctrl Pts',(17.4975990986111,22.535324706586,1.24155587502242));
#50161=CARTESIAN_POINT('Ctrl Pts',(17.4972279975313,22.593186557663,1.26022519179538));
#50162=CARTESIAN_POINT('Ctrl Pts',(17.4967921349267,22.650787135868,1.27997629693771));
#50163=CARTESIAN_POINT('Ctrl Pts',(17.4962762711174,22.7081242847861,1.30081800440496));
#50164=CARTESIAN_POINT('Ctrl Pts',(17.495885950497,22.7515075792346,1.31658757001683));
#50165=CARTESIAN_POINT('Ctrl Pts',(17.495449538331,22.794739902557,1.3329821562078));
#50166=CARTESIAN_POINT('Ctrl Pts',(17.4949590239254,22.8378195794127,1.3500086351081));
#50167=CARTESIAN_POINT('Ctrl Pts',(17.4947863574794,22.8529840977527,1.35600214226495));
#50168=CARTESIAN_POINT('Ctrl Pts',(17.4946069918883,22.8681297006789,1.36207394804995));
#50169=CARTESIAN_POINT('Ctrl Pts',(17.4944205806443,22.8832563145523,1.36822435196836));
#50170=CARTESIAN_POINT('Ctrl Pts',(17.4942996292821,22.8930710902833,1.37221498963649));
#50171=CARTESIAN_POINT('Ctrl Pts',(17.4941757073595,22.9028778694443,1.3762387260773));
#50172=CARTESIAN_POINT('Ctrl Pts',(17.4940487108157,22.9126766271726,1.38029566268096));
#50173=CARTESIAN_POINT('Ctrl Pts',(17.4937998298968,22.9318796995827,1.38824622636712));
#50174=CARTESIAN_POINT('Ctrl Pts',(17.4935391475876,22.9510520670398,1.39632434040982));
#50175=CARTESIAN_POINT('Ctrl Pts',(17.4932658729586,22.9701936608776,1.40453082497143));
#50176=CARTESIAN_POINT('Ctrl Pts',(17.4931847915148,22.9758730321039,1.40696571480785));
#50177=CARTESIAN_POINT('Ctrl Pts',(17.493102633921,22.9815473996187,1.40941092376088));
#50178=CARTESIAN_POINT('Ctrl Pts',(17.4930193820319,22.9872167194344,1.41186642563823));
#50179=CARTESIAN_POINT('Ctrl Pts',(17.4926788650094,23.0104053812626,1.42190992371267));
#50180=CARTESIAN_POINT('Ctrl Pts',(17.4923200195917,23.0335083877323,1.4321250930782));
#50181=CARTESIAN_POINT('Ctrl Pts',(17.4919416369125,23.0565230929821,1.44251025585013));
#50182=CARTESIAN_POINT('Ctrl Pts',(17.4915114173892,23.0826907165728,1.45431814247713));
#50183=CARTESIAN_POINT('Ctrl Pts',(17.4910560346414,23.108746152075,1.46634627633265));
#50184=CARTESIAN_POINT('Ctrl Pts',(17.490573424049,23.1346902308314,1.47859492778473));
#50185=CARTESIAN_POINT('Ctrl Pts',(17.4889430025631,23.222338086273,1.51997500691212));
#50186=CARTESIAN_POINT('Ctrl Pts',(17.4870025099075,23.3087082899385,1.56386879428171));
#50187=CARTESIAN_POINT('Ctrl Pts',(17.484670372646,23.3938013031274,1.61027161191652));
#50188=CARTESIAN_POINT('Ctrl Pts',(17.4844075785837,23.4033899062411,1.61550045721163));
#50189=CARTESIAN_POINT('Ctrl Pts',(17.4841397939398,23.4129622705904,1.62076120310948));
#50190=CARTESIAN_POINT('Ctrl Pts',(17.4838668892062,23.4225183818683,1.62605387207502));
#50191=CARTESIAN_POINT('Ctrl Pts',(17.4833550818764,23.4404399757191,1.63597977821284));
#50192=CARTESIAN_POINT('Ctrl Pts',(17.4828252468312,23.4583057324984,1.64601871842096));
#50193=CARTESIAN_POINT('Ctrl Pts',(17.4822766627014,23.4761117276956,1.65616865981558));
#50194=CARTESIAN_POINT('Ctrl Pts',(17.4821031455161,23.4817437647882,1.65937908674141));
#50195=CARTESIAN_POINT('Ctrl Pts',(17.4819277230214,23.4873706571504,1.66260112059914));
#50196=CARTESIAN_POINT('Ctrl Pts',(17.4817503962822,23.4929915942163,1.66583428205444));
#50197=CARTESIAN_POINT('Ctrl Pts',(17.4810681208541,23.5146184919007,1.6782740676581));
#50198=CARTESIAN_POINT('Ctrl Pts',(17.4803571578544,23.536172216311,1.6908873144974));
#50199=CARTESIAN_POINT('Ctrl Pts',(17.479617865247,23.5575963138373,1.70364094896084));
#50200=CARTESIAN_POINT('Ctrl Pts',(17.477958282088,23.6056896818678,1.7322706373397));
#50201=CARTESIAN_POINT('Ctrl Pts',(17.476155627395,23.6531491234516,1.76161615556983));
#50202=CARTESIAN_POINT('Ctrl Pts',(17.4741950847171,23.6999895710379,1.7916682113668));
#50203=CARTESIAN_POINT('Ctrl Pts',(17.4739538183649,23.7057538035907,1.79536644755433));
#50204=CARTESIAN_POINT('Ctrl Pts',(17.4737101575725,23.7115086337641,1.7990753667281));
#50205=CARTESIAN_POINT('Ctrl Pts',(17.4734640749961,23.7172540790852,1.80279494547923));
#50206=CARTESIAN_POINT('Ctrl Pts',(17.4698561915424,23.8014896126001,1.85732869926873));
#50207=CARTESIAN_POINT('Ctrl Pts',(17.4657284690486,23.8837098705248,1.91415136870024));
#50208=CARTESIAN_POINT('Ctrl Pts',(17.4609881344011,23.963949431093,1.97321360480535));
#50209=CARTESIAN_POINT('Ctrl Pts',(17.459820095904,23.9837207980343,1.98776678947066));
#50210=CARTESIAN_POINT('Ctrl Pts',(17.4586147877116,24.003371890527,2.00245593874073));
#50211=CARTESIAN_POINT('Ctrl Pts',(17.4573708344984,24.0229032147701,2.01728030685903));
#50212=CARTESIAN_POINT('Ctrl Pts',(17.4532220254637,24.0880437149274,2.06672225670958));
#50213=CARTESIAN_POINT('Ctrl Pts',(17.448643463063,24.1518518885441,2.11766841991422));
#50214=CARTESIAN_POINT('Ctrl Pts',(17.4435781789489,24.2143325102693,2.17010759160733));
#50215=CARTESIAN_POINT('Ctrl Pts',(17.4409485699867,24.2467689144586,2.19733104299799));
#50216=CARTESIAN_POINT('Ctrl Pts',(17.4381875267547,24.2788475170732,2.22495686166756));
#50217=CARTESIAN_POINT('Ctrl Pts',(17.4352871220445,24.3105689414372,2.25298341557022));
#50218=CARTESIAN_POINT('Ctrl Pts',(17.4309254795207,24.3582717716431,2.2951298818427));
#50219=CARTESIAN_POINT('Ctrl Pts',(17.4262487958785,24.4051668825869,2.33818257262917));
#50220=CARTESIAN_POINT('Ctrl Pts',(17.4212265144655,24.4512499209496,2.382143488929));
#50221=CARTESIAN_POINT('Ctrl Pts',(17.4164593011656,24.4949925262151,2.42387174898166));
#50222=CARTESIAN_POINT('Ctrl Pts',(17.4113805934181,24.5380034276377,2.46641830448673));
#50223=CARTESIAN_POINT('Ctrl Pts',(17.4059640464874,24.5802788710682,2.50978464770685));
#50224=CARTESIAN_POINT('Ctrl Pts',(17.4018796228843,24.6121572654009,2.54248565041084));
#50225=CARTESIAN_POINT('Ctrl Pts',(17.3976028472266,24.6436170609292,2.57565326805482));
#50226=CARTESIAN_POINT('Ctrl Pts',(17.39312120798,24.6746548098942,2.60929026496544));
#50227=CARTESIAN_POINT('Ctrl Pts',(17.3914919032077,24.685938616941,2.62151903140077));
#50228=CARTESIAN_POINT('Ctrl Pts',(17.389836221474,24.6971619188012,2.63380468104589));
#50229=CARTESIAN_POINT('Ctrl Pts',(17.3881529018836,24.7083293585338,2.64615245298229));
#50230=CARTESIAN_POINT('Ctrl Pts',(17.3849944327058,24.7292832014004,2.66932099287183));
#50231=CARTESIAN_POINT('Ctrl Pts',(17.3817386979368,24.750040460829,2.69270814089779));
#50232=CARTESIAN_POINT('Ctrl Pts',(17.3783762324105,24.7706297433287,2.71635091114708));
#50233=CARTESIAN_POINT('Ctrl Pts',(17.3750221597084,24.7911676343043,2.73993466826672));
#50234=CARTESIAN_POINT('Ctrl Pts',(17.3715683734,24.8114975528878,2.76372648568205));
#50235=CARTESIAN_POINT('Ctrl Pts',(17.3680128472532,24.8316081557027,2.78771437428848));
#50236=CARTESIAN_POINT('Ctrl Pts',(17.36487758354,24.8493416895462,2.80886689956845));
#50237=CARTESIAN_POINT('Ctrl Pts',(17.3616616180351,24.8669148270245,2.83018311470772));
#50238=CARTESIAN_POINT('Ctrl Pts',(17.3583581903393,24.8843453549118,2.85168822445354));
#50239=CARTESIAN_POINT('',(33.,24.8843448987171,2.85168859421269));
#50240=CARTESIAN_POINT('',(33.,24.8843448987171,2.85168859421269));
#50241=CARTESIAN_POINT('',(33.,25.9586702584784,5.35844776698921));
#50242=CARTESIAN_POINT('Origin',(33.,21.,6.));
#50243=CARTESIAN_POINT('',(16.7001695682977,25.9586702584784,5.35844776698921));
#50244=CARTESIAN_POINT('',(33.,25.9586702584784,5.35844776698921));
#50245=CARTESIAN_POINT('',(12.737739127596,21.0000000000011,11.0000004411269));
#50246=CARTESIAN_POINT('Ctrl Pts',(16.7001695682977,25.9586702584784,5.35844776698921));
#50247=CARTESIAN_POINT('Ctrl Pts',(16.6815168127983,25.965091756189,5.40808065434213));
#50248=CARTESIAN_POINT('Ctrl Pts',(16.6625310547284,25.9707499598162,5.45766867161315));
#50249=CARTESIAN_POINT('Ctrl Pts',(16.6335513874865,25.9781098541553,5.53198088911604));
#50250=CARTESIAN_POINT('Ctrl Pts',(16.6238025350965,25.9803762903565,5.55675364744136));
#50251=CARTESIAN_POINT('Ctrl Pts',(16.6041712694858,25.9845290389781,5.60619093181352));
#50252=CARTESIAN_POINT('Ctrl Pts',(16.5547571761654,25.9939617620173,5.72952013772157));
#50253=CARTESIAN_POINT('Ctrl Pts',(16.4628091547597,26.0025509939011,5.94916276413537));
#50254=CARTESIAN_POINT('Ctrl Pts',(16.3339658850875,25.9970981926254,6.23718843853165));
#50255=CARTESIAN_POINT('Ctrl Pts',(16.1990238439482,25.975504867229,6.52053499024951));
#50256=CARTESIAN_POINT('Ctrl Pts',(16.0581197695729,25.9383420850026,6.79932915724524));
#50257=CARTESIAN_POINT('Ctrl Pts',(15.9113820390098,25.8860095180281,7.07367568619639));
#50258=CARTESIAN_POINT('Ctrl Pts',(15.8097490999726,25.8411687118891,7.25366498784544));
#50259=CARTESIAN_POINT('Ctrl Pts',(15.7450631195531,25.8100512278595,7.36526337579501));
#50260=CARTESIAN_POINT('Ctrl Pts',(15.7255699171593,25.8004838956332,7.3986757512472));
#50261=CARTESIAN_POINT('Ctrl Pts',(15.7059462832927,25.790568372936,7.43198774341748));
#50262=CARTESIAN_POINT('Ctrl Pts',(15.6928349513558,25.7838806180605,7.45417346462433));
#50263=CARTESIAN_POINT('Ctrl Pts',(15.6862625186708,25.7804968261681,7.46525906337382));
#50264=CARTESIAN_POINT('Ctrl Pts',(15.6533687738807,25.7634054144588,7.52056348185176));
#50265=CARTESIAN_POINT('Ctrl Pts',(15.5740790820797,25.7207100606511,7.65217921830482));
#50266=CARTESIAN_POINT('Ctrl Pts',(15.4402879227455,25.6413656133805,7.86612271289071));
#50267=CARTESIAN_POINT('Ctrl Pts',(15.2773765226392,25.533506502716,8.11460835176959));
#50268=CARTESIAN_POINT('Ctrl Pts',(15.1123752770098,25.4132859504897,8.35518462851695));
#50269=CARTESIAN_POINT('Ctrl Pts',(14.9455696744292,25.2808344510266,8.58811755602106));
#50270=CARTESIAN_POINT('Ctrl Pts',(14.7772652512398,25.1361316840594,8.81360820573344));
#50271=CARTESIAN_POINT('Ctrl Pts',(14.6642854201341,25.0313784073232,8.95906654165782));
#50272=CARTESIAN_POINT('Ctrl Pts',(14.5935078612877,24.963246272516,9.04847246989379));
#50273=CARTESIAN_POINT('Ctrl Pts',(14.579344128161,24.9494866302156,9.06627832687579));
#50274=CARTESIAN_POINT('Ctrl Pts',(14.551002317804,24.9216984912121,9.10173957065142));
#50275=CARTESIAN_POINT('Ctrl Pts',(14.5368336488764,24.9076791503186,9.11938314343649));
#50276=CARTESIAN_POINT('Ctrl Pts',(14.4943710470597,24.8652768326577,9.17201279261008));
#50277=CARTESIAN_POINT('Ctrl Pts',(14.4095784208147,24.7790539703943,9.27611920728886));
#50278=CARTESIAN_POINT('Ctrl Pts',(14.3252656298858,24.6885446605887,9.37680712616705));
#50279=CARTESIAN_POINT('Ctrl Pts',(14.2413978267288,24.5950949713964,9.47524663394747));
#50280=CARTESIAN_POINT('Ctrl Pts',(14.2135162363307,24.5634545580881,9.50768481340854));
#50281=CARTESIAN_POINT('Ctrl Pts',(14.1718228401221,24.5152434370381,9.55578104820933));
#50282=CARTESIAN_POINT('Ctrl Pts',(14.1579527172013,24.4990549602159,9.57171244470796));
#50283=CARTESIAN_POINT('Ctrl Pts',(14.1303016537839,24.4664766756373,9.60333940388022));
#50284=CARTESIAN_POINT('Ctrl Pts',(14.061374362152,24.3845007066736,9.68184323456448));
#50285=CARTESIAN_POINT('Ctrl Pts',(13.9391682278281,24.2321564517178,9.81811300931258));
#50286=CARTESIAN_POINT('Ctrl Pts',(13.7808174685474,24.0185079321785,9.98920461970393));
#50287=CARTESIAN_POINT('Ctrl Pts',(13.6277824334408,23.7938596003848,10.1497041947624));
#50288=CARTESIAN_POINT('Ctrl Pts',(13.4809224217402,23.5575429373767,10.2994762499161));
#50289=CARTESIAN_POINT('Ctrl Pts',(13.3878214814433,23.3916173563925,10.3919699226421));
#50290=CARTESIAN_POINT('Ctrl Pts',(13.3201119848075,23.2637316738084,10.4584557028409));
#50291=CARTESIAN_POINT('Ctrl Pts',(13.2978955899498,23.2205285879578,10.4801362425612));
#50292=CARTESIAN_POINT('Ctrl Pts',(13.2651473194537,23.1548159997265,10.5119131194855));
#50293=CARTESIAN_POINT('Ctrl Pts',(13.2543248737765,23.1327546033335,10.5223836950478));
#50294=CARTESIAN_POINT('Ctrl Pts',(13.2329531891877,23.0884738040637,10.5430027132959));
#50295=CARTESIAN_POINT('Ctrl Pts',(13.1801617752673,22.9772854867132,10.5937887952691));
#50296=CARTESIAN_POINT('Ctrl Pts',(13.0910034662183,22.7727198735396,10.6783376891869));
#50297=CARTESIAN_POINT('Ctrl Pts',(12.9859558878995,22.4899170949042,10.7760329787102));
#50298=CARTESIAN_POINT('Ctrl Pts',(12.9261760314419,22.2941648401573,10.8307048734092));
#50299=CARTESIAN_POINT('Ctrl Pts',(12.8856443769417,22.144397524114,10.8675453114143));
#50300=CARTESIAN_POINT('Ctrl Pts',(12.8728519361475,22.0939822410721,10.8791305610273));
#50301=CARTESIAN_POINT('Ctrl Pts',(12.857813812923,22.0303162836497,10.8927106869919));
#50302=CARTESIAN_POINT('Ctrl Pts',(12.8518901929655,22.0047689223521,10.898055842651));
#50303=CARTESIAN_POINT('Ctrl Pts',(12.840473575693,21.9536069121313,10.9083423930165));
#50304=CARTESIAN_POINT('Ctrl Pts',(12.8108590803388,21.8126363177099,10.9349671019215));
#50305=CARTESIAN_POINT('Ctrl Pts',(12.7721821385458,21.5804510522391,10.9694847597745));
#50306=CARTESIAN_POINT('Ctrl Pts',(12.7436588266166,21.2837440777459,10.994766558077));
#50307=CARTESIAN_POINT('Ctrl Pts',(12.7377390466039,21.0894198334434,11.0000007967532));
#50308=CARTESIAN_POINT('Ctrl Pts',(12.737739163667,21.,11.0000002000205));
#50309=CARTESIAN_POINT('',(12.7903686062596,20.3177772724646,10.9532413704546));
#50310=CARTESIAN_POINT('Ctrl Pts',(12.7377390915251,21.0000000000022,11.0000006822333));
#50311=CARTESIAN_POINT('Ctrl Pts',(12.7377390793161,20.983622178571,11.0000007571318));
#50312=CARTESIAN_POINT('Ctrl Pts',(12.7378300444133,20.9672306291789,10.9999203240877));
#50313=CARTESIAN_POINT('Ctrl Pts',(12.7380124482716,20.9508252921112,10.9997589559963));
#50314=CARTESIAN_POINT('Ctrl Pts',(12.7385858332176,20.8992552573562,10.9992516968007));
#50315=CARTESIAN_POINT('Ctrl Pts',(12.7400627630646,20.8475489236218,10.9979446845314));
#50316=CARTESIAN_POINT('Ctrl Pts',(12.7424576654204,20.7957039100975,10.9958245673412));
#50317=CARTESIAN_POINT('Ctrl Pts',(12.7430870890103,20.782078104247,10.9952673622554));
#50318=CARTESIAN_POINT('Ctrl Pts',(12.7437799852258,20.7684417515929,10.9946538807978));
#50319=CARTESIAN_POINT('Ctrl Pts',(12.7445364645497,20.7547976107433,10.993983959556));
#50320=CARTESIAN_POINT('Ctrl Pts',(12.745292797437,20.7411561110799,10.9933141679953));
#50321=CARTESIAN_POINT('Ctrl Pts',(12.7461136211149,20.7274927801926,10.9925871539787));
#50322=CARTESIAN_POINT('Ctrl Pts',(12.7469962187263,20.7138522699735,10.9918052322382));
#50323=CARTESIAN_POINT('Ctrl Pts',(12.7487625516298,20.6865536667273,10.9902403808492));
#50324=CARTESIAN_POINT('Ctrl Pts',(12.7507757360796,20.6593467323395,10.9884561487339));
#50325=CARTESIAN_POINT('Ctrl Pts',(12.7530310509817,20.632228541024,10.9864560715966));
#50326=CARTESIAN_POINT('Ctrl Pts',(12.7575489874744,20.5779043018474,10.9824494375437));
#50327=CARTESIAN_POINT('Ctrl Pts',(12.7630383131326,20.5239378683579,10.9775769882869));
#50328=CARTESIAN_POINT('Ctrl Pts',(12.7694621804001,20.470317030689,10.9718644341959));
#50329=CARTESIAN_POINT('Ctrl Pts',(12.7755909244548,20.4191596240379,10.9664143243999));
#50330=CARTESIAN_POINT('Ctrl Pts',(12.7825699912624,20.3683166034407,10.9602002537898));
#50331=CARTESIAN_POINT('Ctrl Pts',(12.7903700169684,20.317778655448,10.9532395922585));
#50332=CARTESIAN_POINT('Ctrl Pts',(12.7903679797893,20.317776478529,10.9532422454443));
#50333=CARTESIAN_POINT('Ctrl Pts',(12.8434562899674,20.2488326393836,10.9437474142331));
#50334=CARTESIAN_POINT('Ctrl Pts',(12.8972986059335,20.1807439610254,10.9329018818484));
#50335=CARTESIAN_POINT('Ctrl Pts',(12.9518162533638,20.113435242677,10.9207733379228));
#50336=CARTESIAN_POINT('Ctrl Pts',(12.9656958022631,20.0962992382508,10.9176855539405));
#50337=CARTESIAN_POINT('Ctrl Pts',(12.9796187325711,20.0792144661478,10.9145147041637));
#50338=CARTESIAN_POINT('Ctrl Pts',(12.9935840678944,20.0621793443964,10.9112617948878));
#50339=CARTESIAN_POINT('Ctrl Pts',(13.0224694241203,20.0269445613606,10.9045336039041));
#50340=CARTESIAN_POINT('Ctrl Pts',(13.0515370653648,19.9919228033594,10.8974532203922));
#50341=CARTESIAN_POINT('Ctrl Pts',(13.0807805059536,19.9571014126526,10.8900268441503));
#50342=CARTESIAN_POINT('Ctrl Pts',(13.0929332878657,19.9426305857383,10.8869406433118));
#50343=CARTESIAN_POINT('Ctrl Pts',(13.1051207143587,19.928189481138,10.8837934389284));
#50344=CARTESIAN_POINT('Ctrl Pts',(13.1173327522049,19.9137883319846,10.880588317183));
#50345=CARTESIAN_POINT('Ctrl Pts',(13.131284118433,19.8973360650924,10.8769266983903));
#50346=CARTESIAN_POINT('Ctrl Pts',(13.1452710623287,19.880932077011,10.8731886307276));
#50347=CARTESIAN_POINT('Ctrl Pts',(13.1592791699167,19.8645910234659,10.8693784137979));
#50348=CARTESIAN_POINT('Ctrl Pts',(13.1626110417999,19.8607042531433,10.8684721418709));
#50349=CARTESIAN_POINT('Ctrl Pts',(13.1659443845299,19.8568207251754,10.8675617136884));
#50350=CARTESIAN_POINT('Ctrl Pts',(13.1692789570691,19.8529406974006,10.8666471986698));
#50351=CARTESIAN_POINT('Ctrl Pts',(13.1799638464198,19.8405080191595,10.8637168405299));
#50352=CARTESIAN_POINT('Ctrl Pts',(13.1906639107593,19.8281081042167,10.8607439641051));
#50353=CARTESIAN_POINT('Ctrl Pts',(13.2013775403923,19.8157419081973,10.8577292831553));
#50354=CARTESIAN_POINT('Ctrl Pts',(13.2501987616835,19.7593900635776,10.8439916040666));
#50355=CARTESIAN_POINT('Ctrl Pts',(13.2993110129335,19.7037274173886,10.8293833334505));
#50356=CARTESIAN_POINT('Ctrl Pts',(13.3486810035835,19.6487052195288,10.8139383477846));
#50357=CARTESIAN_POINT('Ctrl Pts',(13.3846020902726,19.6086716462361,10.8027007384249));
#50358=CARTESIAN_POINT('Ctrl Pts',(13.4206589640815,19.5689762942216,10.7910211694164));
#50359=CARTESIAN_POINT('Ctrl Pts',(13.4568416858135,19.529604654064,10.7789081502023));
#50360=CARTESIAN_POINT('Ctrl Pts',(13.5422974377372,19.4366173675064,10.7502998223748));
#50361=CARTESIAN_POINT('Ctrl Pts',(13.628455197024,19.345434656823,10.7192738351645));
#50362=CARTESIAN_POINT('Ctrl Pts',(13.7151819439768,19.2558755449294,10.6859395947052));
#50363=CARTESIAN_POINT('Ctrl Pts',(13.7447086494671,19.2253845417066,10.6745907278865));
#50364=CARTESIAN_POINT('Ctrl Pts',(13.7743014848463,19.1950819542101,10.6629740955655));
#50365=CARTESIAN_POINT('Ctrl Pts',(13.8039566392106,19.1649627370347,10.6510916278707));
#50366=CARTESIAN_POINT('Ctrl Pts',(13.8986692758511,19.0687679765156,10.613141400691));
#50367=CARTESIAN_POINT('Ctrl Pts',(13.994016243042,18.9744428419228,10.572479736561));
#50368=CARTESIAN_POINT('Ctrl Pts',(14.0898699742255,18.8818316359896,10.5291680010468));
#50369=CARTESIAN_POINT('Ctrl Pts',(14.1121821389326,18.8602742437526,10.5190861965661));
#50370=CARTESIAN_POINT('Ctrl Pts',(14.1345218256674,18.838809790576,10.5088607420322));
#50371=CARTESIAN_POINT('Ctrl Pts',(14.1568878251665,18.8174369505239,10.4984916258405));
#50372=CARTESIAN_POINT('Ctrl Pts',(14.2609862095409,18.7179610420582,10.450230503283));
#50373=CARTESIAN_POINT('Ctrl Pts',(14.3656526004953,18.6204691146559,10.3988575188189));
#50374=CARTESIAN_POINT('Ctrl Pts',(14.4707618766135,18.5248348974924,10.3443708077614));
#50375=CARTESIAN_POINT('Ctrl Pts',(14.4852538760654,18.5116492770229,10.3368584224046));
#50376=CARTESIAN_POINT('Ctrl Pts',(14.4997543126103,18.4984989874017,10.3292868382026));
#50377=CARTESIAN_POINT('Ctrl Pts',(14.5142629317204,18.4853838352381,10.3216558607537));
#50378=CARTESIAN_POINT('Ctrl Pts',(14.6278157552833,18.3827370879263,10.2619314287243));
#50379=CARTESIAN_POINT('Ctrl Pts',(14.7418676902513,18.2822422550503,10.1985691542882));
#50380=CARTESIAN_POINT('Ctrl Pts',(14.8562915152025,18.1838121582644,10.1314750441048));
#50381=CARTESIAN_POINT('Ctrl Pts',(14.8625245743167,18.178450332507,10.1278201972653));
#50382=CARTESIAN_POINT('Ctrl Pts',(14.868758744578,18.1730946498962,10.1241542524972));
#50383=CARTESIAN_POINT('Ctrl Pts',(14.8749940081487,18.1677451025513,10.1204771851252));
#50384=CARTESIAN_POINT('Ctrl Pts',(14.9010586359397,18.1453829427465,10.1051063204738));
#50385=CARTESIAN_POINT('Ctrl Pts',(14.9271433201623,18.123127177324,10.0895405213415));
#50386=CARTESIAN_POINT('Ctrl Pts',(14.9532438663626,18.1009796955978,10.0737797282947));
#50387=CARTESIAN_POINT('Ctrl Pts',(14.9573597919726,18.0974871484866,10.0712943300492));
#50388=CARTESIAN_POINT('Ctrl Pts',(14.9614763622577,18.0939970892013,10.0688039201571));
#50389=CARTESIAN_POINT('Ctrl Pts',(14.9655933074002,18.0905097361136,10.0663086581148));
#50390=CARTESIAN_POINT('Ctrl Pts',(14.9807052856805,18.0777087872804,10.057149355651));
#50391=CARTESIAN_POINT('Ctrl Pts',(14.9958282965693,18.0649392443808,10.0479210261676));
#50392=CARTESIAN_POINT('Ctrl Pts',(15.0109416992674,18.0522180989575,10.038635963182));
#50393=CARTESIAN_POINT('Ctrl Pts',(15.0240720819448,18.0411660869891,10.0305691874453));
#50394=CARTESIAN_POINT('Ctrl Pts',(15.0371962079393,18.0301497486976,10.0224590067606));
#50395=CARTESIAN_POINT('Ctrl Pts',(15.0503109391063,18.0191714817655,10.0143070815373));
#50396=CARTESIAN_POINT('Ctrl Pts',(15.0522915953529,18.0175134856771,10.0130759345614));
#50397=CARTESIAN_POINT('Ctrl Pts',(15.0542721295603,18.0158562786814,10.0118437808848));
#50398=CARTESIAN_POINT('Ctrl Pts',(15.0562525592192,18.0141998452599,10.0106106089146));
#50399=CARTESIAN_POINT('Ctrl Pts',(15.1166272012074,17.9637024320632,9.97301658689186));
#50400=CARTESIAN_POINT('Ctrl Pts',(15.1768397098642,17.9139782963696,9.93451667600521));
#50401=CARTESIAN_POINT('Ctrl Pts',(15.2368747587599,17.8650116797352,9.8951056799024));
#50402=CARTESIAN_POINT('Ctrl Pts',(15.2391019521154,17.8631951054971,9.89364360216164));
#50403=CARTESIAN_POINT('Ctrl Pts',(15.241328901194,17.8613795738775,9.89218027050538));
#50404=CARTESIAN_POINT('Ctrl Pts',(15.243555605196,17.8595650840876,9.89071568466755));
#50405=CARTESIAN_POINT('Ctrl Pts',(15.3613726174717,17.7635587151838,9.8132230644168));
#50406=CARTESIAN_POINT('Ctrl Pts',(15.4785036808088,17.6704633082561,9.73222462895501));
#50407=CARTESIAN_POINT('Ctrl Pts',(15.5948327357961,17.5802272850139,9.64762340806036));
#50408=CARTESIAN_POINT('Ctrl Pts',(15.6051090011199,17.5722560235203,9.64014991321654));
#50409=CARTESIAN_POINT('Ctrl Pts',(15.6153790028259,17.5643070789325,9.63264830144001));
#50410=CARTESIAN_POINT('Ctrl Pts',(15.6256426604821,17.5563804167023,9.62511850365309));
#50411=CARTESIAN_POINT('Ctrl Pts',(15.7337612215943,17.4728800366758,9.54579873973864));
#50412=CARTESIAN_POINT('Ctrl Pts',(15.8411765311664,17.3918521632454,9.46335197543339));
#50413=CARTESIAN_POINT('Ctrl Pts',(15.9477914636026,17.3133225071355,9.37763444589511));
#50414=CARTESIAN_POINT('Ctrl Pts',(15.9655564119421,17.3002373299278,9.36335157341897));
#50415=CARTESIAN_POINT('Ctrl Pts',(15.9832991118044,17.2872215143357,9.34897786889269));
#50416=CARTESIAN_POINT('Ctrl Pts',(16.0010191155428,17.2742751867206,9.33451265040545));
#50417=CARTESIAN_POINT('Ctrl Pts',(16.0997396259617,17.20214946434,9.25392498386404));
#50418=CARTESIAN_POINT('Ctrl Pts',(16.1977563839487,17.1321797945169,9.17049816457455));
#50419=CARTESIAN_POINT('Ctrl Pts',(16.2949836148963,17.064443368653,9.08405651776282));
#50420=CARTESIAN_POINT('Ctrl Pts',(16.3195919152759,17.0472992178009,9.06217805851518));
#50421=CARTESIAN_POINT('Ctrl Pts',(16.3441495460092,17.0302980831823,9.04010636353868));
#50422=CARTESIAN_POINT('Ctrl Pts',(16.3686551330205,17.0134412463967,9.01783851524058));
#50423=CARTESIAN_POINT('Ctrl Pts',(16.4583500788431,16.9517421301287,8.93633410378674));
#50424=CARTESIAN_POINT('Ctrl Pts',(16.5473485126092,16.8919749501211,8.85220358032272));
#50425=CARTESIAN_POINT('Ctrl Pts',(16.635570684301,16.8342545430765,8.76524563934774));
#50426=CARTESIAN_POINT('Ctrl Pts',(16.6662877415817,16.8141575423401,8.73496875993396));
#50427=CARTESIAN_POINT('Ctrl Pts',(16.6969105331036,16.7943085637301,8.70434886696863));
#50428=CARTESIAN_POINT('Ctrl Pts',(16.7274356688887,16.7747124983035,8.67337717653297));
#50429=CARTESIAN_POINT('Ctrl Pts',(16.7527223169831,16.7584793580493,8.64772060804303));
#50430=CARTESIAN_POINT('Ctrl Pts',(16.7779418190892,16.7424202743778,8.62182205621368));
#50431=CARTESIAN_POINT('Ctrl Pts',(16.8030919759031,16.7265389769528,8.59567542647205));
#50432=CARTESIAN_POINT('Ctrl Pts',(16.8072638582608,16.7239046035358,8.59133825020162));
#50433=CARTESIAN_POINT('Ctrl Pts',(16.8114338076789,16.7212751382847,8.58699427440255));
#50434=CARTESIAN_POINT('Ctrl Pts',(16.8156018425759,16.7186505802289,8.58264344148119));
#50435=CARTESIAN_POINT('Ctrl Pts',(16.8302381928505,16.7094342583963,8.56736518297412));
#50436=CARTESIAN_POINT('Ctrl Pts',(16.8448559912736,16.700275319775,8.55199696169292));
#50437=CARTESIAN_POINT('Ctrl Pts',(16.8594321226321,16.6911886462506,8.53656159353562));
#50438=CARTESIAN_POINT('Ctrl Pts',(16.8683206815264,16.685647571545,8.52714907003764));
#50439=CARTESIAN_POINT('Ctrl Pts',(16.8771946790775,16.6801327697938,8.51771063244034));
#50440=CARTESIAN_POINT('Ctrl Pts',(16.8860542917329,16.6746441928681,8.50824583081303));
#50441=CARTESIAN_POINT('Ctrl Pts',(16.8917136312949,16.6711382020599,8.50219990889979));
#50442=CARTESIAN_POINT('Ctrl Pts',(16.8973670214266,16.6676429512188,8.49614329638282));
#50443=CARTESIAN_POINT('Ctrl Pts',(16.903014440287,16.6641584744563,8.49007595574342));
#50444=CARTESIAN_POINT('Ctrl Pts',(16.9248346863519,16.6506953079649,8.4666332345669));
#50445=CARTESIAN_POINT('Ctrl Pts',(16.9465658296515,16.6373928781379,8.44303043631483));
#50446=CARTESIAN_POINT('Ctrl Pts',(16.9682064917946,16.6242534690107,8.41926515768809));
#50447=CARTESIAN_POINT('Ctrl Pts',(17.0039371670362,16.6025591254048,8.38002654996788));
#50448=CARTESIAN_POINT('Ctrl Pts',(17.0394206154598,16.5813090648392,8.34034481226247));
#50449=CARTESIAN_POINT('Ctrl Pts',(17.074649411893,16.5605132459453,8.30020811244834));
#50450=CARTESIAN_POINT('Ctrl Pts',(17.1310442702686,16.5272229442584,8.23595659860588));
#50451=CARTESIAN_POINT('Ctrl Pts',(17.1867866595652,16.4950965230529,8.17053934117279));
#50452=CARTESIAN_POINT('Ctrl Pts',(17.2418413741485,16.4641860460157,8.10389918362116));
#50453=CARTESIAN_POINT('Ctrl Pts',(17.2572778129006,16.4555192553658,8.08521437672919));
#50454=CARTESIAN_POINT('Ctrl Pts',(17.2726601629871,16.4469481174321,8.06643338374958));
#50455=CARTESIAN_POINT('Ctrl Pts',(17.2879875566528,16.4384739888046,8.04755478218108));
#50456=CARTESIAN_POINT('Ctrl Pts',(17.2999282500352,16.4318722811803,8.03284754638253));
#50457=CARTESIAN_POINT('Ctrl Pts',(17.311836394645,16.4253290073801,8.01808007900446));
#50458=CARTESIAN_POINT('Ctrl Pts',(17.3237108911201,16.4188451997394,8.00325252927566));
#50459=CARTESIAN_POINT('Ctrl Pts',(17.3377275293162,16.4111917227248,7.9857501113569));
#50460=CARTESIAN_POINT('Ctrl Pts',(17.351686709864,16.4036269138078,7.96817708826843));
#50461=CARTESIAN_POINT('Ctrl Pts',(17.365583475195,16.396153869281,7.95053850355612));
#50462=CARTESIAN_POINT('Ctrl Pts',(17.3785269138484,16.3891934802204,7.9341099366402));
#50463=CARTESIAN_POINT('Ctrl Pts',(17.3914178358721,16.3823118167066,7.9176224294128));
#50464=CARTESIAN_POINT('Ctrl Pts',(17.4042530587183,16.375510948613,7.90107890777878));
#50465=CARTESIAN_POINT('Ctrl Pts',(17.4168729288614,16.3688241872509,7.8848129576482));
#50466=CARTESIAN_POINT('Ctrl Pts',(17.4294407899082,16.3622143856895,7.86849077308424));
#50467=CARTESIAN_POINT('Ctrl Pts',(17.441956129715,16.3556822722113,7.85211180631862));
#50468=CARTESIAN_POINT('Ctrl Pts',(17.4924446268172,16.3293308828358,7.78603693908791));
#50469=CARTESIAN_POINT('Ctrl Pts',(17.5420754033658,16.3042456250383,7.71904290139493));
#50470=CARTESIAN_POINT('Ctrl Pts',(17.5908169186686,16.2804753070405,7.65109511034566));
#50471=CARTESIAN_POINT('Ctrl Pts',(17.6314450423743,16.2606617371477,7.59445773985922));
#50472=CARTESIAN_POINT('Ctrl Pts',(17.6714540634022,16.2417617277864,7.53715751102069));
#50473=CARTESIAN_POINT('Ctrl Pts',(17.7108251039144,16.2238041307208,7.47917308598077));
#50474=CARTESIAN_POINT('Ctrl Pts',(17.76592085136,16.198674308908,7.39802980919113));
#50475=CARTESIAN_POINT('Ctrl Pts',(17.8197679834448,16.1753887037899,7.3155473825936));
#50476=CARTESIAN_POINT('Ctrl Pts',(17.8722954333774,16.1540653486999,7.2316474353794));
#50477=CARTESIAN_POINT('Ctrl Pts',(17.9127635566461,16.1376374397992,7.16700935737528));
#50478=CARTESIAN_POINT('Ctrl Pts',(17.9524489416381,16.122374319192,7.10153009056992));
#50479=CARTESIAN_POINT('Ctrl Pts',(17.991316201208,16.1083313302537,7.03517033642935));
#50480=CARTESIAN_POINT('Ctrl Pts',(17.9956991543682,16.1067477413044,7.0276871308384));
#50481=CARTESIAN_POINT('Ctrl Pts',(18.0000716863008,16.1051797034,7.02019271084871));
#50482=CARTESIAN_POINT('Ctrl Pts',(18.0044337337432,16.1036273207594,7.01268700758106));
#50483=CARTESIAN_POINT('Ctrl Pts',(18.0442379656541,16.089461633784,6.94419652061061));
#50484=CARTESIAN_POINT('Ctrl Pts',(18.0831706474733,16.0765994460961,6.87476732283058));
#50485=CARTESIAN_POINT('Ctrl Pts',(18.1211854166012,16.0651213575359,6.80434618427197));
#50486=CARTESIAN_POINT('Ctrl Pts',(18.1242794581716,16.0641871500169,6.79861457166108));
#50487=CARTESIAN_POINT('Ctrl Pts',(18.1273674142371,16.0632621207789,6.79287638315313));
#50488=CARTESIAN_POINT('Ctrl Pts',(18.1304492568663,16.0623463189541,6.78713158711253));
#50489=CARTESIAN_POINT('Ctrl Pts',(18.1378420857906,16.0601494623868,6.77335077496775));
#50490=CARTESIAN_POINT('Ctrl Pts',(18.1452001315689,16.058005590398,6.75953118786803));
#50491=CARTESIAN_POINT('Ctrl Pts',(18.1525217962607,16.0559157320938,6.74567469572302));
#50492=CARTESIAN_POINT('Ctrl Pts',(18.1553382746071,16.0551118110036,6.74034441746996));
#50493=CARTESIAN_POINT('Ctrl Pts',(18.1581498491877,16.0543157555517,6.7350077464228));
#50494=CARTESIAN_POINT('Ctrl Pts',(18.1609559414313,16.0535277526109,6.72966573930445));
#50495=CARTESIAN_POINT('Ctrl Pts',(18.1684739225411,16.0514165635587,6.71535362654485));
#50496=CARTESIAN_POINT('Ctrl Pts',(18.175956429109,16.0493620961228,6.70099578061985));
#50497=CARTESIAN_POINT('Ctrl Pts',(18.1833902087664,16.0473685907007,6.6866164312204));
#50498=CARTESIAN_POINT('Ctrl Pts',(18.1859440579559,16.0466837288349,6.68167645566257));
#50499=CARTESIAN_POINT('Ctrl Pts',(18.1884920381816,16.0460060826363,6.67673419643011));
#50500=CARTESIAN_POINT('Ctrl Pts',(18.1910340109504,16.0453356984825,6.67178991047233));
#50501=CARTESIAN_POINT('Ctrl Pts',(18.2087823458192,16.0406550022149,6.63726835935955));
#50502=CARTESIAN_POINT('Ctrl Pts',(18.2262468855533,16.0363259299848,6.60263043249703));
#50503=CARTESIAN_POINT('Ctrl Pts',(18.2434252739949,16.0323528947381,6.5678751954291));
#50504=CARTESIAN_POINT('Ctrl Pts',(18.2454907744798,16.0318751836736,6.56369628427789));
#50505=CARTESIAN_POINT('Ctrl Pts',(18.2475521447674,16.0314026076911,6.55951567913326));
#50506=CARTESIAN_POINT('Ctrl Pts',(18.2496093793473,16.0309351770026,6.55533337795959));
#50507=CARTESIAN_POINT('Ctrl Pts',(18.287943133361,16.022225245133,6.47740191308712));
#50508=CARTESIAN_POINT('Ctrl Pts',(18.3248397905502,16.0153016529865,6.39888133669614));
#50509=CARTESIAN_POINT('Ctrl Pts',(18.360268028959,16.0102313688368,6.31975807490028));
#50510=CARTESIAN_POINT('Ctrl Pts',(18.3948840682106,16.0052773219231,6.24244872904943));
#50511=CARTESIAN_POINT('Ctrl Pts',(18.4280981536683,16.0020925640988,6.16456420270466));
#50512=CARTESIAN_POINT('Ctrl Pts',(18.4598736351268,16.0007411940976,6.08608943957913));
#50513=CARTESIAN_POINT('Ctrl Pts',(18.4606191860281,16.000709486785,6.08424817934664));
#50514=CARTESIAN_POINT('Ctrl Pts',(18.4613639439046,16.0006787906653,6.08240659389164));
#50515=CARTESIAN_POINT('Ctrl Pts',(18.4621079081254,16.0006491068532,6.08056468297652));
#50516=CARTESIAN_POINT('Ctrl Pts',(18.4941108519774,15.9993722048916,6.00133160974362));
#50517=CARTESIAN_POINT('Ctrl Pts',(18.5246472231963,15.9999683001596,5.92149668907681));
#50518=CARTESIAN_POINT('Ctrl Pts',(18.5536700389979,16.0025274553343,5.84104036577652));
#50519=CARTESIAN_POINT('Ctrl Pts',(18.5540771166406,16.0025633503647,5.83991187532773));
#50520=CARTESIAN_POINT('Ctrl Pts',(18.5544838965089,16.0025996316004,5.83878326262644));
#50521=CARTESIAN_POINT('Ctrl Pts',(18.5548903784453,16.0026362993422,5.83765452761047));
#50522=CARTESIAN_POINT('Ctrl Pts',(18.584011904991,16.0052632810575,5.75678872820492));
#50523=CARTESIAN_POINT('Ctrl Pts',(18.6116044017851,16.0098737819706,5.67529517231536));
#50524=CARTESIAN_POINT('Ctrl Pts',(18.6376092606612,16.0165802278325,5.59314944467261));
#50525=CARTESIAN_POINT('Ctrl Pts',(18.6378461675061,16.0166413242198,5.59240108894217));
#50526=CARTESIAN_POINT('Ctrl Pts',(18.6380829425191,16.016702594683,5.5916526790656));
#50527=CARTESIAN_POINT('Ctrl Pts',(18.6383195856488,16.0167640393203,5.59090421502239));
#50528=CARTESIAN_POINT('Ctrl Pts',(18.6512091581932,16.0201108303726,5.55013657644722));
#50529=CARTESIAN_POINT('Ctrl Pts',(18.6637074866172,16.0239743412651,5.50920822384317));
#50530=CARTESIAN_POINT('Ctrl Pts',(18.6758062333863,16.0283705817719,5.46811568192982));
#50531=CARTESIAN_POINT('Ctrl Pts',(18.6760096423787,16.0284444931339,5.46742481760278));
#50532=CARTESIAN_POINT('Ctrl Pts',(18.6762129384104,16.0285185551061,5.46673390686183));
#50533=CARTESIAN_POINT('Ctrl Pts',(18.6764161214387,16.0285927677704,5.46604294968955));
#50534=CARTESIAN_POINT('Ctrl Pts',(18.6823562788628,16.0307624121175,5.44584247128597));
#50535=CARTESIAN_POINT('Ctrl Pts',(18.6881997052906,16.0330607907699,5.42560283441333));
#50536=CARTESIAN_POINT('Ctrl Pts',(18.6939457824567,16.0354901416101,5.4053220485423));
#50537=CARTESIAN_POINT('Ctrl Pts',(18.6941432017144,16.03557360736,5.40462525704836));
#50538=CARTESIAN_POINT('Ctrl Pts',(18.694340503366,16.0356572270006,5.40392842553738));
#50539=CARTESIAN_POINT('Ctrl Pts',(18.6945376867791,16.0357410002752,5.40323155627735));
#50540=CARTESIAN_POINT('Ctrl Pts',(18.6975058848257,16.037002037733,5.39274159698352));
#50541=CARTESIAN_POINT('Ctrl Pts',(18.7004488043604,16.0382985767024,5.38223761241355));
#50542=CARTESIAN_POINT('Ctrl Pts',(18.7033601450231,16.0396278667465,5.37174224549491));
#50543=CARTESIAN_POINT('Ctrl Pts',(18.7060716230313,16.0408659014319,5.3619673823358));
#50544=CARTESIAN_POINT('Ctrl Pts',(18.70875684925,16.0421328325993,5.35219584814628));
#50545=CARTESIAN_POINT('Ctrl Pts',(18.7114155016037,16.0434285560388,5.34242907537816));
#50546=CARTESIAN_POINT('Ctrl Pts',(18.7116114704868,16.0435240636274,5.3417091679602));
#50547=CARTESIAN_POINT('Ctrl Pts',(18.7118073008575,16.0436197300059,5.34098926593463));
#50548=CARTESIAN_POINT('Ctrl Pts',(18.7120029932956,16.0437155554672,5.3402693672978));
#50549=CARTESIAN_POINT('Ctrl Pts',(18.7345571381285,16.054759729455,5.2572988740171));
#50550=CARTESIAN_POINT('Ctrl Pts',(18.7552130822774,16.0678862964141,5.17460458828852));
#50551=CARTESIAN_POINT('Ctrl Pts',(18.7740029111635,16.0831019318703,5.09219308902043));
#50552=CARTESIAN_POINT('Ctrl Pts',(18.7929175112079,16.098418604567,5.00923434803509));
#50553=CARTESIAN_POINT('Ctrl Pts',(18.809941093651,16.1158521667379,4.92656215336943));
#50554=CARTESIAN_POINT('Ctrl Pts',(18.8250960540203,16.1354245241954,4.8441862432899));
#50555=CARTESIAN_POINT('Ctrl Pts',(18.8253306499371,16.1357275005826,4.84291107980051));
#50556=CARTESIAN_POINT('Ctrl Pts',(18.8255647980929,16.1360309894662,4.84163598730577));
#50557=CARTESIAN_POINT('Ctrl Pts',(18.8257984985327,16.1363349909853,4.84036096585361));
#50558=CARTESIAN_POINT('Ctrl Pts',(18.8406319390535,16.1556305834727,4.75943277040838));
#50559=CARTESIAN_POINT('Ctrl Pts',(18.8536617059308,16.1769914395526,4.67879066555096));
#50560=CARTESIAN_POINT('Ctrl Pts',(18.8648995113531,16.2004534307869,4.59844631570716));
#50561=CARTESIAN_POINT('Ctrl Pts',(18.8651500703535,16.200976541203,4.59665495171533));
#50562=CARTESIAN_POINT('Ctrl Pts',(18.8653997385574,16.2015006960943,4.59486373573569));
#50563=CARTESIAN_POINT('Ctrl Pts',(18.8656485159865,16.202025896035,4.59307266793432));
#50564=CARTESIAN_POINT('Ctrl Pts',(18.8767111630417,16.2253805130466,4.51342737610455));
#50565=CARTESIAN_POINT('Ctrl Pts',(18.8860125020265,16.2508015753402,4.43407509786736));
#50566=CARTESIAN_POINT('Ctrl Pts',(18.8935544873796,16.2783399164094,4.35503007473463));
#50567=CARTESIAN_POINT('Ctrl Pts',(18.8937890310808,16.2791963148427,4.35257190073641));
#50568=CARTESIAN_POINT('Ctrl Pts',(18.8940218733296,16.2800547608349,4.35011402387073));
#50569=CARTESIAN_POINT('Ctrl Pts',(18.8942530138872,16.2809152564325,4.34765644467619));
#50570=CARTESIAN_POINT('Ctrl Pts',(18.901606715701,16.3082917934736,4.26946893501563));
#50571=CARTESIAN_POINT('Ctrl Pts',(18.9072381443165,16.337742838823,4.19158273815674));
#50572=CARTESIAN_POINT('Ctrl Pts',(18.9111396520592,16.3693348180566,4.1140148535215));
#50573=CARTESIAN_POINT('Ctrl Pts',(18.9113041187057,16.3706665665043,4.11074500742583));
#50574=CARTESIAN_POINT('Ctrl Pts',(18.9114655101248,16.3720021214958,4.10747572742533));
#50575=CARTESIAN_POINT('Ctrl Pts',(18.9116238251696,16.3733414890653,4.10420701502236));
#50576=CARTESIAN_POINT('Ctrl Pts',(18.9126022985127,16.3816195113147,4.08400458917904));
#50577=CARTESIAN_POINT('Ctrl Pts',(18.9134632533505,16.3900431716412,4.06382384207223));
#50578=CARTESIAN_POINT('Ctrl Pts',(18.9142064386167,16.3986138967783,4.04366512975419));
#50579=CARTESIAN_POINT('Ctrl Pts',(18.9145780312498,16.4028992593469,4.03358577359519));
#50580=CARTESIAN_POINT('Ctrl Pts',(18.91492018149,16.4072213881557,4.02351192619641));
#50581=CARTESIAN_POINT('Ctrl Pts',(18.9152328520037,16.4115804628294,4.01344363010595));
#50582=CARTESIAN_POINT('Ctrl Pts',(18.9154296528748,16.4143241487711,4.00710644973905));
#50583=CARTESIAN_POINT('Ctrl Pts',(18.9156147704606,16.4170826604257,4.00077103457804));
#50584=CARTESIAN_POINT('Ctrl Pts',(18.9157881985968,16.4198557820706,3.99443799822387));
#50585=CARTESIAN_POINT('Ctrl Pts',(18.9158903071701,16.4214885015411,3.9907093223537));
#50586=CARTESIAN_POINT('Ctrl Pts',(18.9159883080047,16.4231254054345,3.98698348363271));
#50587=CARTESIAN_POINT('Ctrl Pts',(18.9160822139542,16.4247664278847,3.98326061358969));
#50588=CARTESIAN_POINT('Ctrl Pts',(18.9169896933056,16.4406247839996,3.94728389742244));
#50589=CARTESIAN_POINT('Ctrl Pts',(18.9175139091381,16.4568624855893,3.91159614557049));
#50590=CARTESIAN_POINT('Ctrl Pts',(18.9176665865239,16.4734724011024,3.87619494858443));
#50591=CARTESIAN_POINT('Ctrl Pts',(18.917684442095,16.4754149253757,3.8720547899908));
#50592=CARTESIAN_POINT('Ctrl Pts',(18.9176972199449,16.4773625657582,3.86791848680186));
#50593=CARTESIAN_POINT('Ctrl Pts',(18.9177049364349,16.4793153223438,3.86378601729374));
#50594=CARTESIAN_POINT('Ctrl Pts',(18.9178429119191,16.5142317846435,3.78989497687927));
#50595=CARTESIAN_POINT('Ctrl Pts',(18.9163622303388,16.5507758632562,3.71724670105414));
#50596=CARTESIAN_POINT('Ctrl Pts',(18.9133556878514,16.5889052577576,3.64580307217914));
#50597=CARTESIAN_POINT('Ctrl Pts',(18.9131504207254,16.591508484308,3.6409253668292));
#50598=CARTESIAN_POINT('Ctrl Pts',(18.9129380401024,16.5941191010895,3.63605327719103));
#50599=CARTESIAN_POINT('Ctrl Pts',(18.9127185708611,16.5967370991315,3.63118679449738));
#50600=CARTESIAN_POINT('Ctrl Pts',(18.909541534267,16.6346352370783,3.56073959420162));
#50601=CARTESIAN_POINT('Ctrl Pts',(18.9048793505736,16.6740801868338,3.49146721648767));
#50602=CARTESIAN_POINT('Ctrl Pts',(18.8988071542983,16.7150448322063,3.42334340472042));
#50603=CARTESIAN_POINT('Ctrl Pts',(18.8983159692325,16.7183584968378,3.41783281226775));
#50604=CARTESIAN_POINT('Ctrl Pts',(18.8978155569235,16.7216821058912,3.41232973573631));
#50605=CARTESIAN_POINT('Ctrl Pts',(18.8973059507854,16.7250156515976,3.40683416612139));
#50606=CARTESIAN_POINT('Ctrl Pts',(18.8910764557557,16.7657653695806,3.3396555726092));
#50607=CARTESIAN_POINT('Ctrl Pts',(18.8834734392306,16.8079999201565,3.27359867681901));
#50608=CARTESIAN_POINT('Ctrl Pts',(18.874557502219,16.8517052118323,3.20864721855841));
#50609=CARTESIAN_POINT('Ctrl Pts',(18.873727329819,16.8557746581322,3.20259951903838));
#50610=CARTESIAN_POINT('Ctrl Pts',(18.8728857949329,16.8598568293621,3.19656138454947));
#50611=CARTESIAN_POINT('Ctrl Pts',(18.872032934654,16.8639517278831,3.1905328120563));
#50612=CARTESIAN_POINT('Ctrl Pts',(18.8620204726742,16.912025271423,3.11975820293151));
#50613=CARTESIAN_POINT('Ctrl Pts',(18.8504454165462,16.9618529594079,3.0503014032411));
#50614=CARTESIAN_POINT('Ctrl Pts',(18.8373731568207,17.0134386315685,2.98215779784787));
#50615=CARTESIAN_POINT('Ctrl Pts',(18.8256639840523,17.0596452982343,2.92111974739844));
#50616=CARTESIAN_POINT('Ctrl Pts',(18.8127529386748,17.1072623184515,2.86113547100402));
#50617=CARTESIAN_POINT('Ctrl Pts',(18.7986799351308,17.1562927705811,2.80220158006905));
#50618=CARTESIAN_POINT('Ctrl Pts',(18.7970416701605,17.1620004982847,2.79534097431564));
#50619=CARTESIAN_POINT('Ctrl Pts',(18.7953876267584,17.1677274192279,2.78849463178943));
#50620=CARTESIAN_POINT('Ctrl Pts',(18.7937178488403,17.173473563644,2.7816625657979));
#50621=CARTESIAN_POINT('Ctrl Pts',(18.7857111070413,17.2010268653014,2.74890216828991));
#50622=CARTESIAN_POINT('Ctrl Pts',(18.777343128714,17.2290221456169,2.71647005900353));
#50623=CARTESIAN_POINT('Ctrl Pts',(18.768619532796,17.2574626897857,2.68436776726638));
#50624=CARTESIAN_POINT('Ctrl Pts',(18.764257734837,17.2716829618701,2.66831662139781));
#50625=CARTESIAN_POINT('Ctrl Pts',(18.7598051746857,17.2860204098879,2.65234150641107));
#50626=CARTESIAN_POINT('Ctrl Pts',(18.7552687457753,17.3004555867387,2.63646439120962));
#50627=CARTESIAN_POINT('Ctrl Pts',(18.7527806301356,17.3083729133391,2.62775619817379));
#50628=CARTESIAN_POINT('Ctrl Pts',(18.7502684011593,17.3163161197489,2.61908129049594));
#50629=CARTESIAN_POINT('Ctrl Pts',(18.7477317115031,17.3242869956653,2.61043750466746));
#50630=CARTESIAN_POINT('Ctrl Pts',(18.7456434102184,17.3308489297889,2.6033216050123));
#50631=CARTESIAN_POINT('Ctrl Pts',(18.743537844844,17.3374316642756,2.59622471924828));
#50632=CARTESIAN_POINT('Ctrl Pts',(18.7414166468313,17.344030582907,2.5891515796704));
#50633=CARTESIAN_POINT('Ctrl Pts',(18.738865117639,17.3519682357925,2.58064349979919));
#50634=CARTESIAN_POINT('Ctrl Pts',(18.7362901984525,17.3599316998598,2.57216721755547));
#50635=CARTESIAN_POINT('Ctrl Pts',(18.7336951875099,17.3679113629952,2.56373281991339));
#50636=CARTESIAN_POINT('Ctrl Pts',(18.7289379676969,17.3825398221459,2.54827073344745));
#50637=CARTESIAN_POINT('Ctrl Pts',(18.724110082699,17.3972328178983,2.53293818335603));
#50638=CARTESIAN_POINT('Ctrl Pts',(18.7192130608308,17.4119905493229,2.51773232191264));
#50639=CARTESIAN_POINT('Ctrl Pts',(18.7094086698816,17.4415371946729,2.48728846964402));
#50640=CARTESIAN_POINT('Ctrl Pts',(18.6993272580374,17.4713432420696,2.45735228351929));
#50641=CARTESIAN_POINT('Ctrl Pts',(18.6889796594319,17.501411375434,2.42790290780628));
#50642=CARTESIAN_POINT('Ctrl Pts',(18.6865516176034,17.5084667984646,2.42099267493209));
#50643=CARTESIAN_POINT('Ctrl Pts',(18.6841089777729,17.515536610181,2.41410916805059));
#50644=CARTESIAN_POINT('Ctrl Pts',(18.6816518430478,17.5226208725668,2.40725216818588));
#50645=CARTESIAN_POINT('Ctrl Pts',(18.6606398054745,17.5832015098058,2.3486149525189));
#50646=CARTESIAN_POINT('Ctrl Pts',(18.6385732142793,17.6448185426341,2.29193550295218));
#50647=CARTESIAN_POINT('Ctrl Pts',(18.6155445047684,17.7074495954823,2.23713374068759));
#50648=CARTESIAN_POINT('Ctrl Pts',(18.5952360125508,17.7626824885256,2.18880531994261));
#50649=CARTESIAN_POINT('Ctrl Pts',(18.5741783699363,17.8187036782295,2.14193759021419));
#50650=CARTESIAN_POINT('Ctrl Pts',(18.5524266721411,17.8754960551877,2.09647914071758));
#50651=CARTESIAN_POINT('Ctrl Pts',(18.5495131449393,17.8831030997816,2.09039021697443));
#50652=CARTESIAN_POINT('Ctrl Pts',(18.5465871498316,17.8907239868604,2.08432659257798));
#50653=CARTESIAN_POINT('Ctrl Pts',(18.5436487795668,17.8983587060738,2.07828820069466));
#50654=CARTESIAN_POINT('Ctrl Pts',(18.5187732391351,17.9629924143411,2.02716861810383));
#50655=CARTESIAN_POINT('Ctrl Pts',(18.493012338885,18.0286179750865,1.97785685211132));
#50656=CARTESIAN_POINT('Ctrl Pts',(18.4664312545691,18.0952307061165,1.93031234669157));
#50657=CARTESIAN_POINT('Ctrl Pts',(18.4428122010353,18.1544205285307,1.88806590537245));
#50658=CARTESIAN_POINT('Ctrl Pts',(18.41854323848,18.2143895483544,1.8472150191826));
#50659=CARTESIAN_POINT('Ctrl Pts',(18.3936671179681,18.2751336625744,1.8077328993508));
#50660=CARTESIAN_POINT('Ctrl Pts',(18.3625516420487,18.3511134369268,1.75834799030573));
#50661=CARTESIAN_POINT('Ctrl Pts',(18.3304856337078,18.4283059298595,1.7111048659539));
#50662=CARTESIAN_POINT('Ctrl Pts',(18.2975275019964,18.5067263915645,1.66599177173665));
#50663=CARTESIAN_POINT('Ctrl Pts',(18.2707759860673,18.5703788536896,1.629374293867));
#50664=CARTESIAN_POINT('Ctrl Pts',(18.2434352523388,18.6348454890174,1.59415750987106));
#50665=CARTESIAN_POINT('Ctrl Pts',(18.2155405293451,18.700118449349,1.56034406141925));
#50666=CARTESIAN_POINT('Ctrl Pts',(18.2125143152344,18.7071997153523,1.55667574268882));
#50667=CARTESIAN_POINT('Ctrl Pts',(18.2094813141992,18.7142910609668,1.55302370505177));
#50668=CARTESIAN_POINT('Ctrl Pts',(18.2064417088042,18.7213921460605,1.54938813161792));
#50669=CARTESIAN_POINT('Ctrl Pts',(18.198677267509,18.7395313290066,1.54010133519732));
#50670=CARTESIAN_POINT('Ctrl Pts',(18.1908700725115,18.7577334941773,1.53092223109942));
#50671=CARTESIAN_POINT('Ctrl Pts',(18.1830206415079,18.7759989510875,1.52185095427166));
#50672=CARTESIAN_POINT('Ctrl Pts',(18.1781063167304,18.7874344790161,1.51617166357434));
#50673=CARTESIAN_POINT('Ctrl Pts',(18.1731754349275,18.7988948155038,1.51053465364943));
#50674=CARTESIAN_POINT('Ctrl Pts',(18.1682293461457,18.8103771802602,1.5049413900067));
#50675=CARTESIAN_POINT('Ctrl Pts',(18.1652752687015,18.8172350827825,1.50160078398545));
#50676=CARTESIAN_POINT('Ctrl Pts',(18.1623177029271,18.8240963542693,1.49827795144323));
#50677=CARTESIAN_POINT('Ctrl Pts',(18.1593568281399,18.8309606733165,1.49497297744696));
#50678=CARTESIAN_POINT('Ctrl Pts',(18.1463365332697,18.8611461639232,1.48043952397064));
#50679=CARTESIAN_POINT('Ctrl Pts',(18.1332465050168,18.8914039864737,1.46624494618778));
#50680=CARTESIAN_POINT('Ctrl Pts',(18.1200901414679,18.9217340445751,1.45238407310797));
#50681=CARTESIAN_POINT('Ctrl Pts',(18.1172443145164,18.9282946793938,1.44938585509466));
#50682=CARTESIAN_POINT('Ctrl Pts',(18.1143953877743,18.934858692716,1.4464032417234));
#50683=CARTESIAN_POINT('Ctrl Pts',(18.1115433909991,18.9414260850989,1.44343619124119));
#50684=CARTESIAN_POINT('Ctrl Pts',(18.082026041729,19.0093967141136,1.41272806907662));
#50685=CARTESIAN_POINT('Ctrl Pts',(18.0521796023943,19.0777294006106,1.38368689482883));
#50686=CARTESIAN_POINT('Ctrl Pts',(18.0220380007022,19.1464249078126,1.35626665519777));
#50687=CARTESIAN_POINT('Ctrl Pts',(17.9866754333215,19.227019480291,1.32409682953767));
#50688=CARTESIAN_POINT('Ctrl Pts',(17.9509084798126,19.3081127623388,1.29415358338591));
#50689=CARTESIAN_POINT('Ctrl Pts',(17.9147779185929,19.3897109870291,1.26639573762749));
#50690=CARTESIAN_POINT('Ctrl Pts',(17.8833654764719,19.4606536855018,1.2422626576571));
#50691=CARTESIAN_POINT('Ctrl Pts',(17.8516776321339,19.531977766523,1.21978161321308));
#50692=CARTESIAN_POINT('Ctrl Pts',(17.8197410752445,19.6036866097686,1.19892627464732));
#50693=CARTESIAN_POINT('Ctrl Pts',(17.7836341935295,19.6847593042972,1.17534761382524));
#50694=CARTESIAN_POINT('Ctrl Pts',(17.7472091082188,19.7663238553438,1.15384744917031));
#50695=CARTESIAN_POINT('Ctrl Pts',(17.7104897656853,19.8483907356608,1.13442371693699));
#50696=CARTESIAN_POINT('Ctrl Pts',(17.6773925085894,19.9223623388952,1.11691598898944));
#50697=CARTESIAN_POINT('Ctrl Pts',(17.6440561966807,19.9967417246677,1.10109534075644));
#50698=CARTESIAN_POINT('Ctrl Pts',(17.6104984919182,20.0715363698375,1.0869606873673));
#50699=CARTESIAN_POINT('Ctrl Pts',(17.5738959008892,20.1531175693769,1.0715435144408));
#50700=CARTESIAN_POINT('Ctrl Pts',(17.5370292830112,20.2351941866344,1.05813195497465));
#50701=CARTESIAN_POINT('Ctrl Pts',(17.4999100362541,20.317778319276,1.04675761316854));
#50702=CARTESIAN_POINT('Origin',(6.61363325216158E-15,53.,-24.));
#50703=CARTESIAN_POINT('',(4.1991313379145,53.,-27.5520833333334));
#50704=CARTESIAN_POINT('',(-4.19913133791448,53.,-27.5520833333334));
#50705=CARTESIAN_POINT('Origin',(6.61363325216158E-15,53.,-24.));
#50706=CARTESIAN_POINT('',(3.43565291283914,52.,-26.90625));
#50707=CARTESIAN_POINT('Origin',(3.43565291283914,53.,-26.90625));
#50708=CARTESIAN_POINT('',(-3.43565291283912,52.,-26.90625));
#50709=CARTESIAN_POINT('Origin',(6.61363325216158E-15,52.,-24.));
#50710=CARTESIAN_POINT('Origin',(-3.43565291283912,53.,-26.90625));
#50711=CARTESIAN_POINT('Origin',(5.2045770037451E-16,8.5,0.));
#50712=CARTESIAN_POINT('',(-1.83698839911727E-15,9.00000000000001,19.5));
#50713=CARTESIAN_POINT('Origin',(-1.86760355796283E-15,8.50000000000001,
19.5));
#50714=CARTESIAN_POINT('Origin',(5.51072859220069E-16,9.,-1.70652395450943E-16));
#50715=CARTESIAN_POINT('Ctrl Pts',(-14.1696709084508,34.2228423347593,-8.45401835497186));
#50716=CARTESIAN_POINT('Ctrl Pts',(-14.4598881528388,34.2800112558736,-7.96758898230353));
#50717=CARTESIAN_POINT('Ctrl Pts',(-15.0284388422964,34.3091931864527,-7.97011831445158));
#50718=CARTESIAN_POINT('Ctrl Pts',(-14.1687509928547,34.2417094783908,-8.45556021361394));
#50719=CARTESIAN_POINT('Ctrl Pts',(-14.4590195349379,34.2974823791094,-7.96916514970434));
#50720=CARTESIAN_POINT('Ctrl Pts',(-15.027463174257,34.3259639809838,-7.97157191635228));
#50721=CARTESIAN_POINT('Ctrl Pts',(-14.1678668544491,34.2605265108349,-8.45704153677041));
#50722=CARTESIAN_POINT('Ctrl Pts',(-14.4581845937863,34.3149090256939,-7.97067959720386));
#50723=CARTESIAN_POINT('Ctrl Pts',(-15.0265254516828,34.3426902318517,-7.97296845218914));
#50724=CARTESIAN_POINT('Ctrl Pts',(-14.1661635328208,34.2981938523499,-8.45989441550156));
#50725=CARTESIAN_POINT('Ctrl Pts',(-14.4565759909218,34.3497943960948,-7.97359633424001));
#50726=CARTESIAN_POINT('Ctrl Pts',(-15.024718898452,34.3761723132014,-7.97565803480127));
#50727=CARTESIAN_POINT('Ctrl Pts',(-14.1653454356421,34.3170219168472,-8.46126415076535));
#50728=CARTESIAN_POINT('Ctrl Pts',(-14.4558033400937,34.3672326811367,-7.97499678944735));
#50729=CARTESIAN_POINT('Ctrl Pts',(-15.0238512196152,34.3929083705295,-7.97694936773952));
#50730=CARTESIAN_POINT('Ctrl Pts',(-14.1629917065432,34.373489337447,-8.46520379440197));
#50731=CARTESIAN_POINT('Ctrl Pts',(-14.4535804037852,34.41953098386,-7.97902465759217));
#50732=CARTESIAN_POINT('Ctrl Pts',(-15.0213548402835,34.4431016332889,-7.98066350984471));
#50733=CARTESIAN_POINT('Ctrl Pts',(-14.1615566384215,34.4111119211253,-8.4676041477937));
#50734=CARTESIAN_POINT('Ctrl Pts',(-14.4522248265318,34.454380888302,-7.98147914140516));
#50735=CARTESIAN_POINT('Ctrl Pts',(-15.0198327983173,34.4765439298872,-7.98292646932796));
#50736=CARTESIAN_POINT('Ctrl Pts',(-14.1576526183944,34.5239129308506,-8.47413110853782));
#50737=CARTESIAN_POINT('Ctrl Pts',(-14.4485372614658,34.5588642949711,-7.98815276719896));
#50738=CARTESIAN_POINT('Ctrl Pts',(-15.0156921710414,34.5768114940933,-7.98907983290995));
#50739=CARTESIAN_POINT('Ctrl Pts',(-14.1555848703909,34.5990246231075,-8.47758373051289));
#50740=CARTESIAN_POINT('Ctrl Pts',(-14.446583355318,34.6284571865908,-7.99168420593832));
#50741=CARTESIAN_POINT('Ctrl Pts',(-15.0134991049499,34.6435774427604,-7.99233483016131));
#50742=CARTESIAN_POINT('Ctrl Pts',(-14.1509771790097,34.8240952679178,-8.4852743386372));
#50743=CARTESIAN_POINT('Ctrl Pts',(-14.4422301623517,34.8369697425827,-7.99954874151129));
#50744=CARTESIAN_POINT('Ctrl Pts',(-15.008612159576,34.8436402381527,-7.99958523498254));
#50745=CARTESIAN_POINT('Ctrl Pts',(-14.1500330992177,34.9737899010413,-8.48684678418226));
#50746=CARTESIAN_POINT('Ctrl Pts',(-14.4413373565372,34.9757252603891,-8.00115815623579));
#50747=CARTESIAN_POINT('Ctrl Pts',(-15.0076108628144,34.9767021342601,-8.00106767539272));
#50748=CARTESIAN_POINT('Ctrl Pts',(-14.1534989333457,35.4218322689878,-8.48106645017854));
#50749=CARTESIAN_POINT('Ctrl Pts',(-14.4446127086534,35.3909181528281,-7.99524560707017));
#50750=CARTESIAN_POINT('Ctrl Pts',(-15.0112867474724,35.3749620168757,-7.99561820204977));
#50751=CARTESIAN_POINT('Ctrl Pts',(-14.1642118082204,35.7191401530233,-8.46324178895702));
#50752=CARTESIAN_POINT('Ctrl Pts',(-14.454761563286,35.6666794668494,-7.97697017454646));
#50753=CARTESIAN_POINT('Ctrl Pts',(-15.0226488876287,35.6392356915726,-7.97881380780291));
#50754=CARTESIAN_POINT('Ctrl Pts',(-14.2018700963651,36.3110245203784,-8.3998954453284));
#50755=CARTESIAN_POINT('Ctrl Pts',(-14.4903036805241,36.2145680745722,-7.91223236340415));
#50756=CARTESIAN_POINT('Ctrl Pts',(-15.0625894960227,36.1653551292289,-7.91909334909917));
#50757=CARTESIAN_POINT('Ctrl Pts',(-14.2288151924285,36.6056011119585,-8.35437505244428));
#50758=CARTESIAN_POINT('Ctrl Pts',(-14.5157733460828,36.4872920363756,-7.86562765440656));
#50759=CARTESIAN_POINT('Ctrl Pts',(-15.0911676285592,36.4272009883655,-7.87617850054425));
#50760=CARTESIAN_POINT('Ctrl Pts',(-14.2678515285549,36.9354562627635,-8.28724846986359));
#50761=CARTESIAN_POINT('Ctrl Pts',(-14.5524221273012,36.7911880341194,-7.7973135407053));
#50762=CARTESIAN_POINT('Ctrl Pts',(-15.1325698029845,36.7204055669061,-7.81289418035236));
#50763=CARTESIAN_POINT('Ctrl Pts',(-14.272310834891,36.9720923458365,-8.27956682548256));
#50764=CARTESIAN_POINT('Ctrl Pts',(-14.5566164314028,36.8250040101967,-7.78948085637131));
#50765=CARTESIAN_POINT('Ctrl Pts',(-15.1372993703662,36.7529709740877,-7.80565222610578));
#50766=CARTESIAN_POINT('Ctrl Pts',(-14.2814663750741,37.0452925529125,-8.26376437000761));
#50767=CARTESIAN_POINT('Ctrl Pts',(-14.5652251137911,36.8925526698609,-7.77337133120969));
#50768=CARTESIAN_POINT('Ctrl Pts',(-15.1470097917179,36.8180378248002,-7.79075428816105));
#50769=CARTESIAN_POINT('Ctrl Pts',(-14.2861536017617,37.081785083136,-8.25565910563603));
#50770=CARTESIAN_POINT('Ctrl Pts',(-14.5696312954759,36.9262202981498,-7.76510980926654));
#50771=CARTESIAN_POINT('Ctrl Pts',(-15.1519810928061,36.850475629465,-7.78311296160134));
#50772=CARTESIAN_POINT('Ctrl Pts',(-14.3005366026303,37.1909436147287,-8.23073635121615));
#50773=CARTESIAN_POINT('Ctrl Pts',(-14.5831518360579,37.0269359064794,-7.7397041366779));
#50774=CARTESIAN_POINT('Ctrl Pts',(-15.1672357906114,36.9475054352928,-7.7596167619714));
#50775=CARTESIAN_POINT('Ctrl Pts',(-14.3105536680637,37.263290615546,-8.21331202705747));
#50776=CARTESIAN_POINT('Ctrl Pts',(-14.5925608990619,37.0936355928615,-7.7219524972774));
#50777=CARTESIAN_POINT('Ctrl Pts',(-15.1778599510383,37.0118138805059,-7.74318978992613));
#50778=CARTESIAN_POINT('Ctrl Pts',(-14.3418348010998,37.4790826477386,-8.15864801908498));
#50779=CARTESIAN_POINT('Ctrl Pts',(-14.6219410641221,37.2926085843646,-7.66625367882849));
#50780=CARTESIAN_POINT('Ctrl Pts',(-15.211036910134,37.2036290201708,-7.69165469791198));
#50781=CARTESIAN_POINT('Ctrl Pts',(-14.3643283878283,37.6212795682079,-8.11901917638115));
#50782=CARTESIAN_POINT('Ctrl Pts',(-14.6430362895773,37.4235089284438,-7.62591654935295));
#50783=CARTESIAN_POINT('Ctrl Pts',(-15.2348937448071,37.3300262828855,-7.65429417319524));
#50784=CARTESIAN_POINT('Ctrl Pts',(-14.4363019502445,38.0430610597211,-7.9907944336361));
#50785=CARTESIAN_POINT('Ctrl Pts',(-14.7105067497658,37.8118623201918,-7.49538846499181));
#50786=CARTESIAN_POINT('Ctrl Pts',(-15.3112293408869,37.7049431641283,-7.53340889331172));
#50787=CARTESIAN_POINT('Ctrl Pts',(-14.49026980554,38.3178484315225,-7.8928871878268));
#50788=CARTESIAN_POINT('Ctrl Pts',(-14.7609541970719,38.0639420611781,-7.39588717756517));
#50789=CARTESIAN_POINT('Ctrl Pts',(-15.3684679759171,37.9491986058153,-7.44110576650622));
#50790=CARTESIAN_POINT('Ctrl Pts',(-14.6080482783172,38.8552917835711,-7.67271221247472));
#50791=CARTESIAN_POINT('Ctrl Pts',(-14.8703740139742,38.5549584396854,-7.17322618837634));
#50792=CARTESIAN_POINT('Ctrl Pts',(-15.4933845372648,38.4269260298234,-7.2335333987612));
#50793=CARTESIAN_POINT('Ctrl Pts',(-14.6718611162741,39.1179471327802,-7.55044413842592));
#50794=CARTESIAN_POINT('Ctrl Pts',(-14.9295100780991,38.794189655202,-7.04967693049274));
#50795=CARTESIAN_POINT('Ctrl Pts',(-15.5610648206959,38.6603974512983,-7.11826383427611));
#50796=CARTESIAN_POINT('Ctrl Pts',(-14.7480666188548,39.4067715675604,-7.3989787087425));
#50797=CARTESIAN_POINT('Ctrl Pts',(-14.999316825149,39.0547855952716,-6.89817098281311));
#50798=CARTESIAN_POINT('Ctrl Pts',(-15.6418888381287,38.9171302822837,-6.97546814291349));
#50799=CARTESIAN_POINT('Ctrl Pts',(-14.7565941785648,39.4387656880567,-7.38195749962283));
#50800=CARTESIAN_POINT('Ctrl Pts',(-15.0071581686653,39.0837656036217,-6.88107637534832));
#50801=CARTESIAN_POINT('Ctrl Pts',(-15.6509332197322,38.9455695005142,-6.95942121181813));
#50802=CARTESIAN_POINT('Ctrl Pts',(-14.7737256022962,39.502412269052,-7.34761186407861));
#50803=CARTESIAN_POINT('Ctrl Pts',(-15.0228997481459,39.1413825527381,-6.84659981861948));
#50804=CARTESIAN_POINT('Ctrl Pts',(-15.6691029114839,39.002144239138,-6.92704148796774));
#50805=CARTESIAN_POINT('Ctrl Pts',(-14.7823346424693,39.5340844533758,-7.33027717344031));
#50806=CARTESIAN_POINT('Ctrl Pts',(-15.0308049908594,39.1700375342947,-6.82920681792526));
#50807=CARTESIAN_POINT('Ctrl Pts',(-15.6782337117527,39.0302972919077,-6.91069901878126));
#50808=CARTESIAN_POINT('Ctrl Pts',(-14.808284656594,39.6286524867301,-7.27779013265149));
#50809=CARTESIAN_POINT('Ctrl Pts',(-15.0546319241823,39.2556023565078,-6.77653515305077));
#50810=CARTESIAN_POINT('Ctrl Pts',(-15.7057564538778,39.1143577659461,-6.8612162865755));
#50811=CARTESIAN_POINT('Ctrl Pts',(-14.8257484822497,39.6910999140348,-7.24215491242092));
#50812=CARTESIAN_POINT('Ctrl Pts',(-15.0706345822693,39.31199951062,-6.74082930478049));
#50813=CARTESIAN_POINT('Ctrl Pts',(-15.7242786933826,39.1698665902847,-6.8276207929431));
#50814=CARTESIAN_POINT('Ctrl Pts',(-14.8785762907581,39.876683136037,-7.1333351875412));
#50815=CARTESIAN_POINT('Ctrl Pts',(-15.1190327204018,39.4796219387076,-6.63176677641015));
#50816=CARTESIAN_POINT('Ctrl Pts',(-15.7803081869927,39.3348294541919,-6.72502980625943));
#50817=CARTESIAN_POINT('Ctrl Pts',(-14.9143760584171,39.9980613049761,-7.05823809590922));
#50818=CARTESIAN_POINT('Ctrl Pts',(-15.1516954791241,39.5888243403568,-6.5567294842393));
#50819=CARTESIAN_POINT('Ctrl Pts',(-15.8182776378986,39.4427211600206,-6.65423120166715));
#50820=CARTESIAN_POINT('Ctrl Pts',(-15.0231004266237,40.3553871225062,-6.82537958602282));
#50821=CARTESIAN_POINT('Ctrl Pts',(-15.2508296348633,39.9103610239103,-6.3239951350709));
#50822=CARTESIAN_POINT('Ctrl Pts',(-15.9335913612037,39.7603441088107,-6.43470129294701));
#50823=CARTESIAN_POINT('Ctrl Pts',(-15.0973449297501,40.5845463158894,-6.66007288714214));
#50824=CARTESIAN_POINT('Ctrl Pts',(-15.31792988494,40.114768031037,-6.15976330372408));
#50825=CARTESIAN_POINT('Ctrl Pts',(-16.0123355319573,39.9640411696614,-6.2788565940716));
#50826=CARTESIAN_POINT('Ctrl Pts',(-15.2472968949109,41.0254173108877,-6.30922595793956));
#50827=CARTESIAN_POINT('Ctrl Pts',(-15.4523126364001,40.5055857309467,-5.81354666702777));
#50828=CARTESIAN_POINT('Ctrl Pts',(-16.1713754941982,40.3559264985848,-5.94809181206602));
#50829=CARTESIAN_POINT('Ctrl Pts',(-15.3230087426575,41.2371284648137,-6.12368686448347));
#50830=CARTESIAN_POINT('Ctrl Pts',(-15.5196455447178,40.6918988399555,-5.63122192702778));
#50831=CARTESIAN_POINT('Ctrl Pts',(-16.2516759396333,40.5441141908017,-5.77317280154761));
#50832=CARTESIAN_POINT('Ctrl Pts',(-15.4173521697931,41.4908768942127,-5.87860618526534));
#50833=CARTESIAN_POINT('Ctrl Pts',(-15.6023498902727,40.9125245108878,-5.39340306565551));
#50834=CARTESIAN_POINT('Ctrl Pts',(-16.3517371496677,40.7696683504473,-5.54212030933746));
#50835=CARTESIAN_POINT('Ctrl Pts',(-15.4362061333438,41.541080480963,-5.82893036895881));
#50836=CARTESIAN_POINT('Ctrl Pts',(-15.6189216498825,40.9563040712589,-5.34503370394812));
#50837=CARTESIAN_POINT('Ctrl Pts',(-16.3717337779055,40.814293760811,-5.49528788992432));
#50838=CARTESIAN_POINT('Ctrl Pts',(-15.4644422759024,41.6155621820111,-5.75341180123559));
#50839=CARTESIAN_POINT('Ctrl Pts',(-15.6436600403385,41.0210733659742,-5.27169025022555));
#50840=CARTESIAN_POINT('Ctrl Pts',(-16.4016812016563,40.8804997173657,-5.42409193382638));
#50841=CARTESIAN_POINT('Ctrl Pts',(-15.4738394697509,41.6402325166288,-5.72809098740203));
#50842=CARTESIAN_POINT('Ctrl Pts',(-15.6518901269291,41.042522534143,-5.24709833812979));
#50843=CARTESIAN_POINT('Ctrl Pts',(-16.4116479225022,40.9024289036886,-5.40022045953334));
#50844=CARTESIAN_POINT('Ctrl Pts',(-15.4925703942472,41.689181898316,-5.67723496738244));
#50845=CARTESIAN_POINT('Ctrl Pts',(-15.6682749940766,41.0850380021743,-5.1977485436834));
#50846=CARTESIAN_POINT('Ctrl Pts',(-16.4315140544655,40.9459394651512,-5.35227539009512));
#50847=CARTESIAN_POINT('Ctrl Pts',(-15.5019086640392,41.7134729307954,-5.65168764188966));
#50848=CARTESIAN_POINT('Ctrl Pts',(-15.6764336314637,41.1061140969787,-5.17297859437461));
#50849=CARTESIAN_POINT('Ctrl Pts',(-16.4414182800811,40.967531494057,-5.32819036948575));
#50850=CARTESIAN_POINT('Ctrl Pts',(-15.5484555651202,41.8340156143712,-5.52335553940722));
#50851=CARTESIAN_POINT('Ctrl Pts',(-15.7171539857794,41.2108612547213,-5.04834447526745));
#50852=CARTESIAN_POINT('Ctrl Pts',(-16.4907862052723,41.074680546041,-5.20720387542547));
#50853=CARTESIAN_POINT('Ctrl Pts',(-15.5852305114518,41.9275319640208,-5.41878553611691));
#50854=CARTESIAN_POINT('Ctrl Pts',(-15.7490791740827,41.2915492195499,-4.94737813664718));
#50855=CARTESIAN_POINT('Ctrl Pts',(-16.5297899365528,41.1578061902771,-5.10861936072794));
#50856=CARTESIAN_POINT('Ctrl Pts',(-15.6938508583456,42.199498468939,-5.0993756835597));
#50857=CARTESIAN_POINT('Ctrl Pts',(-15.8432282443095,41.526068650345,-4.63908945210971));
#50858=CARTESIAN_POINT('Ctrl Pts',(-16.64499333428,41.3995541945398,-4.80749222676696));
#50859=CARTESIAN_POINT('Ctrl Pts',(-15.7639910093299,42.369390564411,-4.87885064391805));
#50860=CARTESIAN_POINT('Ctrl Pts',(-15.9031097774975,41.6705184443034,-4.42842552480797));
#50861=CARTESIAN_POINT('Ctrl Pts',(-16.7193844041967,41.5505693905269,-4.59958983270443));
#50862=CARTESIAN_POINT('Ctrl Pts',(-15.8980969848804,42.6866289429011,-4.42234195955402));
#50863=CARTESIAN_POINT('Ctrl Pts',(-16.0164770439618,41.938203868012,-3.99591210397994));
#50864=CARTESIAN_POINT('Ctrl Pts',(-16.8616180139052,41.8325590604172,-4.16921127494601));
#50865=CARTESIAN_POINT('Ctrl Pts',(-15.9620670091645,42.8339757168234,-4.18635981457349));
#50866=CARTESIAN_POINT('Ctrl Pts',(-16.069837618137,42.061051465547,-3.77409145591909));
#50867=CARTESIAN_POINT('Ctrl Pts',(-16.9294650101271,41.9635339702937,-3.94673652549938));
#50868=CARTESIAN_POINT('Ctrl Pts',(-16.0521582726785,43.037709823846,-3.82021108244197));
#50869=CARTESIAN_POINT('Ctrl Pts',(-16.1440256404094,42.2291011383052,-3.43385778245536));
#50870=CARTESIAN_POINT('Ctrl Pts',(-17.0250163496069,42.1446309546378,-3.60154580164102));
#50871=CARTESIAN_POINT('Ctrl Pts',(-16.0812108244472,43.102733976819,-3.69612831892062));
#50872=CARTESIAN_POINT('Ctrl Pts',(-16.1678670548505,42.2825951618778,-3.31868636626619));
#50873=CARTESIAN_POINT('Ctrl Pts',(-17.0558296625103,42.2024302014641,-3.48456541848317));
#50874=CARTESIAN_POINT('Ctrl Pts',(-16.1231583043917,43.1958323041313,-3.50684228674254));
#50875=CARTESIAN_POINT('Ctrl Pts',(-16.2020593980967,42.358743766398,-3.14397959827399));
#50876=CARTESIAN_POINT('Ctrl Pts',(-17.1003194136399,42.2851842704153,-3.30611394037726));
#50877=CARTESIAN_POINT('Ctrl Pts',(-16.1368688153599,43.2261249913638,-3.44321966940264));
#50878=CARTESIAN_POINT('Ctrl Pts',(-16.2132166154573,42.3834909358494,-3.0852944650872));
#50879=CARTESIAN_POINT('Ctrl Pts',(-17.1148608648885,42.3121111033463,-3.24613302164169));
#50880=CARTESIAN_POINT('Ctrl Pts',(-16.1570050576291,43.2704363362883,-3.3469780073553));
#50881=CARTESIAN_POINT('Ctrl Pts',(-16.2295461487012,42.4195814461551,-2.99676810231204));
#50882=CARTESIAN_POINT('Ctrl Pts',(-17.1362174853078,42.3514989656337,-3.15540014162311));
#50883=CARTESIAN_POINT('Ctrl Pts',(-16.1636460804533,43.2850199841448,-3.31476016326283));
#50884=CARTESIAN_POINT('Ctrl Pts',(-16.234927397343,42.4314525764685,-2.96714277235139));
#50885=CARTESIAN_POINT('Ctrl Pts',(-17.1432609944394,42.3644622081519,-3.12502641655731));
#50886=CARTESIAN_POINT('Ctrl Pts',(-16.176779066406,43.3138032530051,-3.25006285951472));
#50887=CARTESIAN_POINT('Ctrl Pts',(-16.2455540938229,42.4548543838694,-2.90771276300664));
#50888=CARTESIAN_POINT('Ctrl Pts',(-17.1571899188963,42.3900473359813,-3.0640323254552));
#50889=CARTESIAN_POINT('Ctrl Pts',(-16.1832563592051,43.3279707317643,-3.21765573302902));
#50890=CARTESIAN_POINT('Ctrl Pts',(-16.2507873073283,42.4663580683418,-2.87797525515983));
#50891=CARTESIAN_POINT('Ctrl Pts',(-17.164059774934,42.4026406504781,-3.03348015236247));
#50892=CARTESIAN_POINT('Ctrl Pts',(-16.2407423662139,43.4534701977211,-2.92546660438112));
#50893=CARTESIAN_POINT('Ctrl Pts',(-16.2973926330638,42.5686355463496,-2.60882804918763));
#50894=CARTESIAN_POINT('Ctrl Pts',(-17.2250297821921,42.5141957311396,-2.75801565386698));
#50895=CARTESIAN_POINT('Ctrl Pts',(-16.2860851710674,43.5507845829967,-2.66201787685001));
#50896=CARTESIAN_POINT('Ctrl Pts',(-16.3334056853608,42.6464652770683,-2.36955567429105));
#50897=CARTESIAN_POINT('Ctrl Pts',(-17.27312063616,42.6006974071258,-2.50964648325415));
#50898=CARTESIAN_POINT('Ctrl Pts',(-16.3644674413509,43.7174968151427,-2.12770174998652));
#50899=CARTESIAN_POINT('Ctrl Pts',(-16.395286619085,42.7792030237934,-1.88723589636282));
#50900=CARTESIAN_POINT('Ctrl Pts',(-17.3562533467079,42.7488860578871,-2.00591410770285));
#50901=CARTESIAN_POINT('Ctrl Pts',(-16.3975090775376,43.7868935216046,-1.85683435243505));
#50902=CARTESIAN_POINT('Ctrl Pts',(-16.4209906605381,42.8337387768024,-1.64478289056291));
#50903=CARTESIAN_POINT('Ctrl Pts',(-17.3912975066884,42.810572019061,-1.75055090464328));
#50904=CARTESIAN_POINT('Ctrl Pts',(-16.4371973244655,43.8698191922474,-1.44484551307843));
#50905=CARTESIAN_POINT('Ctrl Pts',(-16.4517290374466,42.8986843931254,-1.27807359738039));
#50906=CARTESIAN_POINT('Ctrl Pts',(-17.4333911016012,42.8842837265137,-1.36214391805839));
#50907=CARTESIAN_POINT('Ctrl Pts',(-16.4487802554229,43.8939261909356,-1.30656641831514));
#50908=CARTESIAN_POINT('Ctrl Pts',(-16.4606689802262,42.9175109064172,-1.15517368833686));
#50909=CARTESIAN_POINT('Ctrl Pts',(-17.4456760285918,42.9057121696064,-1.23177978830181));
#50910=CARTESIAN_POINT('Ctrl Pts',(-16.4685324538335,43.9349488754536,-1.02806931366241));
#50911=CARTESIAN_POINT('Ctrl Pts',(-16.4758894976883,42.9495081386978,-0.908068000066032));
#50912=CARTESIAN_POINT('Ctrl Pts',(-17.4666253297105,42.9421767782951,-0.969223595380726));
#50913=CARTESIAN_POINT('Ctrl Pts',(-16.4767018066094,43.9518647448791,-0.887851353093695));
#50914=CARTESIAN_POINT('Ctrl Pts',(-16.4821582142198,42.9626536650404,-0.783956213361243));
#50915=CARTESIAN_POINT('Ctrl Pts',(-17.4752897950108,42.9572131064008,-0.837031578665104));
#50916=CARTESIAN_POINT('Ctrl Pts',(-16.4862967209135,43.9717089312722,-0.676029616417883));
#50917=CARTESIAN_POINT('Ctrl Pts',(-16.4895137451409,42.9780633749711,-0.596718279805704));
#50918=CARTESIAN_POINT('Ctrl Pts',(-17.4854662190897,42.9748523834323,-0.637334318512984));
#50919=CARTESIAN_POINT('Ctrl Pts',(-16.4890517437789,43.977401569991,-0.605173122314613));
#50920=CARTESIAN_POINT('Ctrl Pts',(-16.4916238230334,42.9824805634447,-0.534110465633991));
#50921=CARTESIAN_POINT('Ctrl Pts',(-17.4883882131625,42.9799125065679,-0.57053358332299));
#50922=CARTESIAN_POINT('Ctrl Pts',(-16.492506023628,43.9845357058383,-0.498508314718125));
#50923=CARTESIAN_POINT('Ctrl Pts',(-16.4942681869357,42.9880140786458,-0.439912398698345));
#50924=CARTESIAN_POINT('Ctrl Pts',(-17.49205184321,42.9862539607906,-0.469974168759785));
#50925=CARTESIAN_POINT('Ctrl Pts',(-16.4935448911152,43.9866805929804,-0.462870708599939));
#50926=CARTESIAN_POINT('Ctrl Pts',(-16.4950632373273,42.9896773373646,-0.408444310922235));
#50927=CARTESIAN_POINT('Ctrl Pts',(-17.4931536723775,42.9881605271315,-0.436376425617608));
#50928=CARTESIAN_POINT('Ctrl Pts',(-16.495392016117,43.9904934577505,-0.391554086603203));
#50929=CARTESIAN_POINT('Ctrl Pts',(-16.4964765826267,42.9926335814917,-0.345482344139571));
#50930=CARTESIAN_POINT('Ctrl Pts',(-17.4951127443838,42.9915497401849,-0.36914189982643));
#50931=CARTESIAN_POINT('Ctrl Pts',(-16.4961991039929,43.9921590221803,-0.355925418204801));
#50932=CARTESIAN_POINT('Ctrl Pts',(-16.4970939068081,42.9939245371181,-0.314034598998794));
#50933=CARTESIAN_POINT('Ctrl Pts',(-17.4959687466422,42.9930302419732,-0.335552582820379));
#50934=CARTESIAN_POINT('Ctrl Pts',(-16.4996553193878,43.9992904788907,-0.177929344977772));
#50935=CARTESIAN_POINT('Ctrl Pts',(-16.499737824245,42.9994528692837,-0.156906377895304));
#50936=CARTESIAN_POINT('Ctrl Pts',(-17.4996344297213,42.9993693144289,-0.167744837011927));
#50937=CARTESIAN_POINT('Ctrl Pts',(-16.5005671676994,44.0011697501096,-0.0360034841747721));
#50938=CARTESIAN_POINT('Ctrl Pts',(-16.5004336035839,43.0009063138008,-0.0317784680747621));
#50939=CARTESIAN_POINT('Ctrl Pts',(-17.5006015414388,43.0010397779723,-0.0339426786824198));
#50940=CARTESIAN_POINT('Ctrl Pts',(-16.4978545553025,43.9955752404001,0.388390909530019));
#50941=CARTESIAN_POINT('Ctrl Pts',(-16.4983604076717,42.9965730007167,0.34258128637437));
#50942=CARTESIAN_POINT('Ctrl Pts',(-17.4977245284721,42.9960668801614,0.366159780026568));
#50943=CARTESIAN_POINT('Ctrl Pts',(-16.488785846129,43.9768969118701,0.669479171266392));
#50944=CARTESIAN_POINT('Ctrl Pts',(-16.4914621272788,42.9821709666193,0.590248849637306));
#50945=CARTESIAN_POINT('Ctrl Pts',(-17.488106200346,42.9794639216913,0.631158814660471));
#50946=CARTESIAN_POINT('Ctrl Pts',(-16.4566137829713,43.9102406346531,1.22805693613211));
#50947=CARTESIAN_POINT('Ctrl Pts',(-16.4667388442969,42.9303002753056,1.08490481084554));
#50948=CARTESIAN_POINT('Ctrl Pts',(-17.4539843153664,42.9202138974404,1.15776411487348));
#50949=CARTESIAN_POINT('Ctrl Pts',(-16.4335093295897,43.8622622073091,1.50554633472257));
#50950=CARTESIAN_POINT('Ctrl Pts',(-16.4489907660971,42.8929980278654,1.33109833842561));
#50951=CARTESIAN_POINT('Ctrl Pts',(-17.4294795919199,42.8775664063642,1.41937028185803));
#50952=CARTESIAN_POINT('Ctrl Pts',(-16.3960891495453,43.783793740335,1.85015317363005));
#50953=CARTESIAN_POINT('Ctrl Pts',(-16.4197798825902,42.8310926576272,1.63991769895437));
#50954=CARTESIAN_POINT('Ctrl Pts',(-17.3897915222624,42.8078166581088,1.74425215023244));
#50955=CARTESIAN_POINT('Ctrl Pts',(-16.3881779026531,43.767173088473,1.91896157031875));
#50956=CARTESIAN_POINT('Ctrl Pts',(-16.4136093423201,42.817995097094,1.70150596722071));
#50957=CARTESIAN_POINT('Ctrl Pts',(-17.3814008058283,42.7930427452666,1.80912201914365));
#50958=CARTESIAN_POINT('Ctrl Pts',(-16.375673948842,43.740841555206,2.0220039170481));
#50959=CARTESIAN_POINT('Ctrl Pts',(-16.4038270264028,42.7971893690875,1.79393530076847));
#50960=CARTESIAN_POINT('Ctrl Pts',(-17.3681390366586,42.7696369379822,1.90626631910862));
#50961=CARTESIAN_POINT('Ctrl Pts',(-16.3713997812811,43.7318309227685,2.05632298830878));
#50962=CARTESIAN_POINT('Ctrl Pts',(-16.4004812785263,42.7900667948439,1.82472882562818));
#50963=CARTESIAN_POINT('Ctrl Pts',(-17.3636058286238,42.7616274868815,1.93862099907206));
#50964=CARTESIAN_POINT('Ctrl Pts',(-16.3626396751579,43.7133407089755,2.12490420765856));
#50965=CARTESIAN_POINT('Ctrl Pts',(-16.3936154941633,42.7754354074154,1.88631707234903));
#50966=CARTESIAN_POINT('Ctrl Pts',(-17.3543148069932,42.7451917413354,2.0032766940958));
#50967=CARTESIAN_POINT('Ctrl Pts',(-16.3581504674953,43.7038542075336,2.15919050412873));
#50968=CARTESIAN_POINT('Ctrl Pts',(-16.3900932136698,42.7679218136654,1.9171321516777));
#50969=CARTESIAN_POINT('Ctrl Pts',(-17.3495535260841,42.7367592956301,2.03560047527918));
#50970=CARTESIAN_POINT('Ctrl Pts',(-16.335218649852,43.6553329579177,2.33016678950607));
#50971=CARTESIAN_POINT('Ctrl Pts',(-16.3721055730023,42.7295090646878,2.07069458061821));
#50972=CARTESIAN_POINT('Ctrl Pts',(-17.3252319015473,42.6936292957481,2.19679023923976));
#50973=CARTESIAN_POINT('Ctrl Pts',(-16.315354751774,43.6131097667714,2.46525055695651));
#50974=CARTESIAN_POINT('Ctrl Pts',(-16.3564409704719,42.6959272836267,2.19259820200646));
#50975=CARTESIAN_POINT('Ctrl Pts',(-17.3041641304931,42.6560975705951,2.32414193923568));
#50976=CARTESIAN_POINT('Ctrl Pts',(-16.2515056057596,43.4765147512805,2.8655905997197));
#50977=CARTESIAN_POINT('Ctrl Pts',(-16.3058885440615,42.5869423044208,2.55446830067613));
#50978=CARTESIAN_POINT('Ctrl Pts',(-17.2364453397946,42.5346797786526,2.7015668953238));
#50979=CARTESIAN_POINT('Ctrl Pts',(-16.2032672081898,43.3722448995847,3.12594764367366));
#50980=CARTESIAN_POINT('Ctrl Pts',(-16.2673330709852,42.5030995032564,2.7919929023725));
#50981=CARTESIAN_POINT('Ctrl Pts',(-17.1852834023163,42.441995466392,2.94702134755456));
#50982=CARTESIAN_POINT('Ctrl Pts',(-16.0968875664402,43.1381380127393,3.63422998231717));
#50983=CARTESIAN_POINT('Ctrl Pts',(-16.1809970935074,42.3122776252218,3.25988799511517));
#50984=CARTESIAN_POINT('Ctrl Pts',(-17.07245651017,42.2339004556738,3.42621008435598));
#50985=CARTESIAN_POINT('Ctrl Pts',(-16.0387426559475,43.0082992884229,3.88215383492437));
#50986=CARTESIAN_POINT('Ctrl Pts',(-16.1333904856796,42.2057238967836,3.48991370242924));
#50987=CARTESIAN_POINT('Ctrl Pts',(-17.0107876651219,42.118488256322,3.65994300926234));
#50988=CARTESIAN_POINT('Ctrl Pts',(-15.9607089630699,42.8300074294681,4.18445557032663));
#50989=CARTESIAN_POINT('Ctrl Pts',(-16.0682434684036,42.0567601433772,3.77421115204722));
#50990=CARTESIAN_POINT('Ctrl Pts',(-16.9280246578707,41.9600066039851,3.94494127844591));
#50991=CARTESIAN_POINT('Ctrl Pts',(-15.9448345125254,42.7935473084438,4.2445349020985));
#50992=CARTESIAN_POINT('Ctrl Pts',(-16.0550169591108,42.026372413421,3.83055888715714));
#50993=CARTESIAN_POINT('Ctrl Pts',(-16.9111881192775,41.9275976074833,4.00158172585483));
#50994=CARTESIAN_POINT('Ctrl Pts',(-15.9125710995365,42.7190148602521,4.3639323057479));
#50995=CARTESIAN_POINT('Ctrl Pts',(-16.0280522148975,41.964087720814,3.94277369967183));
#50996=CARTESIAN_POINT('Ctrl Pts',(-16.8769693480609,41.8613465424687,4.1141449347411));
#50997=CARTESIAN_POINT('Ctrl Pts',(-15.8961777996028,42.6809324048149,4.42326572017825));
#50998=CARTESIAN_POINT('Ctrl Pts',(-16.0143130159987,41.9321895117794,3.99865250806258));
#50999=CARTESIAN_POINT('Ctrl Pts',(-16.8595825146128,41.8274954710167,4.17008216045151));
#51000=CARTESIAN_POINT('Ctrl Pts',(-15.8462844618934,42.5643109368609,4.60002845907672));
#51001=CARTESIAN_POINT('Ctrl Pts',(-15.9724388258778,41.8344100525786,4.16519179553658));
#51002=CARTESIAN_POINT('Ctrl Pts',(-16.8066653386068,41.723831943736,4.33672716677812));
#51003=CARTESIAN_POINT('Ctrl Pts',(-15.8122905956358,42.4839122053499,4.71544824060082));
#51004=CARTESIAN_POINT('Ctrl Pts',(-15.9437057928047,41.7665897154923,4.27457431431909));
#51005=CARTESIAN_POINT('Ctrl Pts',(-16.7706112375754,41.652366404853,4.44554042885686));
#51006=CARTESIAN_POINT('Ctrl Pts',(-15.708466257085,42.2349319229732,5.05470392926197));
#51007=CARTESIAN_POINT('Ctrl Pts',(-15.8557182823553,41.5561640523473,4.59624091151791));
#51008=CARTESIAN_POINT('Ctrl Pts',(-16.6604945155305,41.4310505980033,4.76537744171326));
#51009=CARTESIAN_POINT('Ctrl Pts',(-15.6367937805477,42.0585895493903,5.27155542705688));
#51010=CARTESIAN_POINT('Ctrl Pts',(-15.7941524221352,41.4054489545328,4.80429063353521));
#51011=CARTESIAN_POINT('Ctrl Pts',(-16.5844782517039,41.274301821729,4.96981656414753));
#51012=CARTESIAN_POINT('Ctrl Pts',(-15.490346672854,41.6855007303992,5.68751055477781));
#51013=CARTESIAN_POINT('Ctrl Pts',(-15.6669541386688,41.0833353282907,5.20593767654318));
#51014=CARTESIAN_POINT('Ctrl Pts',(-16.42915556251,40.9426673158617,5.36196281266631));
#51015=CARTESIAN_POINT('Ctrl Pts',(-15.4155675047962,41.4887542028889,5.88661251495239));
#51016=CARTESIAN_POINT('Ctrl Pts',(-15.6013785695094,40.9122288799408,5.39970005563699));
#51017=CARTESIAN_POINT('Ctrl Pts',(-16.3498443229104,40.7677815136044,5.54966836406231));
#51018=CARTESIAN_POINT('Ctrl Pts',(-15.3024448812762,41.1779991716065,6.17216839972268));
#51019=CARTESIAN_POINT('Ctrl Pts',(-15.5009241601739,40.6387285873814,5.6799934650858));
#51020=CARTESIAN_POINT('Ctrl Pts',(-16.2298657833509,40.4915548192431,5.81887929950314));
#51021=CARTESIAN_POINT('Ctrl Pts',(-15.2645790020526,41.0718024829547,6.26516634094168));
#51022=CARTESIAN_POINT('Ctrl Pts',(-15.4672614165944,40.5452444380058,5.77127906622756));
#51023=CARTESIAN_POINT('Ctrl Pts',(-16.1897050020046,40.3971577625623,5.90655412600363));
#51024=CARTESIAN_POINT('Ctrl Pts',(-15.2077254227751,40.9084929741541,6.4013676517502));
#51025=CARTESIAN_POINT('Ctrl Pts',(-15.4164278105277,40.4007199180155,5.90553521152224));
#51026=CARTESIAN_POINT('Ctrl Pts',(-16.1294057515143,40.2519937548357,6.03495940239176));
#51027=CARTESIAN_POINT('Ctrl Pts',(-15.1887651989012,40.853386989109,6.44621852703614));
#51028=CARTESIAN_POINT('Ctrl Pts',(-15.3994674120309,40.3519488749432,5.94974031533987));
#51029=CARTESIAN_POINT('Ctrl Pts',(-16.1092964229923,40.2030106569473,6.07724305571356));
#51030=CARTESIAN_POINT('Ctrl Pts',(-15.1508585131677,40.7418148130405,6.53481506085914));
#51031=CARTESIAN_POINT('Ctrl Pts',(-15.365491794666,40.2530328359572,6.03717495128596));
#51032=CARTESIAN_POINT('Ctrl Pts',(-16.0690923625353,40.1038353894078,6.16076840762205));
#51033=CARTESIAN_POINT('Ctrl Pts',(-15.1319787469483,40.685544542223,6.57840481672826));
#51034=CARTESIAN_POINT('Ctrl Pts',(-15.348535637605,40.2030632212813,6.08025593853515));
#51035=CARTESIAN_POINT('Ctrl Pts',(-16.0490683678638,40.0538173708934,6.20186312687394));
#51036=CARTESIAN_POINT('Ctrl Pts',(-15.0380664911524,40.4019030685421,6.79276143414887));
#51037=CARTESIAN_POINT('Ctrl Pts',(-15.2644245680603,39.9519367964584,6.29138993605124));
#51038=CARTESIAN_POINT('Ctrl Pts',(-15.9494644607597,39.8016916163679,6.40395017364007));
#51039=CARTESIAN_POINT('Ctrl Pts',(-14.9644461532019,40.1675514041411,6.95288768593992));
#51040=CARTESIAN_POINT('Ctrl Pts',(-15.1976171693671,39.7421821058477,6.45092268656129));
#51041=CARTESIAN_POINT('Ctrl Pts',(-15.8713822833035,39.5933790259089,6.55491094954876));
#51042=CARTESIAN_POINT('Ctrl Pts',(-14.8222211698946,39.6838140960417,7.25114166432459));
#51043=CARTESIAN_POINT('Ctrl Pts',(-15.06786594057,39.3068953284827,6.74885869506734));
#51044=CARTESIAN_POINT('Ctrl Pts',(-15.7205376048291,39.1633903075869,6.83609315171071));
#51045=CARTESIAN_POINT('Ctrl Pts',(-14.7536128479239,39.4344290298586,7.38926853498414));
#51046=CARTESIAN_POINT('Ctrl Pts',(-15.0048054725226,39.0812939904251,6.88766092280371));
#51047=CARTESIAN_POINT('Ctrl Pts',(-15.6477712019922,38.9417146931311,6.96631377005003));
#51048=CARTESIAN_POINT('Ctrl Pts',(-14.6235443336384,38.9199395169773,7.64345031191053));
#51049=CARTESIAN_POINT('Ctrl Pts',(-14.8848011659622,38.6139543580119,7.14351801279062));
#51050=CARTESIAN_POINT('Ctrl Pts',(-15.5098197481496,38.4843906818341,7.20594642230858));
#51051=CARTESIAN_POINT('Ctrl Pts',(-14.5620800221653,38.6548384656211,7.7595087284317));
#51052=CARTESIAN_POINT('Ctrl Pts',(-14.827716689627,38.3720620877045,7.26095612384862));
#51053=CARTESIAN_POINT('Ctrl Pts',(-15.4446303262328,38.2487453026412,7.31536176370244));
#51054=CARTESIAN_POINT('Ctrl Pts',(-14.4912109590877,38.3128451067789,7.89022745753408));
#51055=CARTESIAN_POINT('Ctrl Pts',(-14.7615399553527,38.0581196581985,7.39373762359809));
#51056=CARTESIAN_POINT('Ctrl Pts',(-15.369466168806,37.944751206059,7.43859827658201));
#51057=CARTESIAN_POINT('Ctrl Pts',(-14.4773360216078,38.2439139811986,7.91565127929397));
#51058=CARTESIAN_POINT('Ctrl Pts',(-14.7486090785329,37.9949822886081,7.41950389459761));
#51059=CARTESIAN_POINT('Ctrl Pts',(-15.3547503258741,37.883479094363,7.46256686250324));
#51060=CARTESIAN_POINT('Ctrl Pts',(-14.4570026893877,38.1396985883734,7.95268958299778));
#51061=CARTESIAN_POINT('Ctrl Pts',(-14.7296347176249,37.8994093453111,7.45707777466083));
#51062=CARTESIAN_POINT('Ctrl Pts',(-15.3331846705994,37.7908431896831,7.49748512881753));
#51063=CARTESIAN_POINT('Ctrl Pts',(-14.4502995623675,38.1047958815478,7.9648621653037));
#51064=CARTESIAN_POINT('Ctrl Pts',(-14.7233795289916,37.8674039475413,7.46942463090051));
#51065=CARTESIAN_POINT('Ctrl Pts',(-15.326075293378,37.7598185613842,7.50896096392519));
#51066=CARTESIAN_POINT('Ctrl Pts',(-14.4370862536553,38.0348626145466,7.98878759631039));
#51067=CARTESIAN_POINT('Ctrl Pts',(-14.711044089513,37.8032526976823,7.49369902639856));
#51068=CARTESIAN_POINT('Ctrl Pts',(-15.3120611781612,37.6976556573663,7.531516925812));
#51069=CARTESIAN_POINT('Ctrl Pts',(-14.430578191227,37.9998443555349,8.00053668324475));
#51070=CARTESIAN_POINT('Ctrl Pts',(-14.7049654891278,37.7711173950731,7.50562346769514));
#51071=CARTESIAN_POINT('Ctrl Pts',(-15.3051586876244,37.6665283160382,7.54259350608998));
#51072=CARTESIAN_POINT('Ctrl Pts',(-14.3985378950991,37.8244951111472,8.05821896776018));
#51073=CARTESIAN_POINT('Ctrl Pts',(-14.6750683621745,37.6103672676509,7.56410181532715));
#51074=CARTESIAN_POINT('Ctrl Pts',(-15.2711765555705,37.5106623209909,7.59697411101706));
#51075=CARTESIAN_POINT('Ctrl Pts',(-14.3745058364078,37.6833906877742,8.10096493484399));
#51076=CARTESIAN_POINT('Ctrl Pts',(-14.652561930448,37.4806229720141,7.60757184213281));
#51077=CARTESIAN_POINT('Ctrl Pts',(-15.2456880081703,37.3852361669233,7.63727333921995));
#51078=CARTESIAN_POINT('Ctrl Pts',(-14.3074780704631,37.2575991659697,8.21914076587046));
#51079=CARTESIAN_POINT('Ctrl Pts',(-14.5898331467566,37.0893377713944,7.72760627073598));
#51080=CARTESIAN_POINT('Ctrl Pts',(-15.1745979538034,37.0067548141695,7.74868489717074));
#51081=CARTESIAN_POINT('Ctrl Pts',(-14.2695523034726,36.9704386282229,8.28453464061196));
#51082=CARTESIAN_POINT('Ctrl Pts',(-14.5540974775854,36.8241663199945,7.79441727640368));
#51083=CARTESIAN_POINT('Ctrl Pts',(-15.1343736550051,36.7515010028509,7.81033568794618));
#51084=CARTESIAN_POINT('Ctrl Pts',(-14.2086105787285,36.3893814021093,8.38862459376293));
#51085=CARTESIAN_POINT('Ctrl Pts',(-14.4967075641971,36.2872858361014,7.90063819784113));
#51086=CARTESIAN_POINT('Ctrl Pts',(-15.069738492784,36.2350056907777,7.90846763065641));
#51087=CARTESIAN_POINT('Ctrl Pts',(-14.1855946049829,36.0954849072401,8.42732167623407));
#51088=CARTESIAN_POINT('Ctrl Pts',(-14.474938277723,36.0150460990806,7.94027178393654));
#51089=CARTESIAN_POINT('Ctrl Pts',(-15.04532761125,35.9737643619689,7.94494972814297));
#51090=CARTESIAN_POINT('Ctrl Pts',(-14.1632592796937,35.6493675288365,8.46476803043535));
#51091=CARTESIAN_POINT('Ctrl Pts',(-14.4538374531707,35.601719694416,7.97857185535198));
#51092=CARTESIAN_POINT('Ctrl Pts',(-15.0216386300259,35.5772155811991,7.98025268877251));
#51093=CARTESIAN_POINT('Ctrl Pts',(-14.1578452220156,35.4997817266829,8.47381023741147));
#51094=CARTESIAN_POINT('Ctrl Pts',(-14.4487195544893,35.4631107873063,7.98782407910831));
#51095=CARTESIAN_POINT('Ctrl Pts',(-15.0158964475708,35.4442504237115,7.98877732802181));
#51096=CARTESIAN_POINT('Ctrl Pts',(-14.1528931524912,35.2740434072532,8.48207673460457));
#51097=CARTESIAN_POINT('Ctrl Pts',(-14.4440400975708,35.2539384493497,7.99627922136717));
#51098=CARTESIAN_POINT('Ctrl Pts',(-15.0106442526529,35.2435941397839,7.99657065897525));
#51099=CARTESIAN_POINT('Ctrl Pts',(-14.1517706094402,35.1985706100121,8.48394895723216));
#51100=CARTESIAN_POINT('Ctrl Pts',(-14.442979184077,35.184001549869,7.9981943881281));
#51101=CARTESIAN_POINT('Ctrl Pts',(-15.0094536766753,35.1765072088985,7.99833571715932));
#51102=CARTESIAN_POINT('Ctrl Pts',(-14.1508941306251,35.0850155880073,8.4854107517919));
#51103=CARTESIAN_POINT('Ctrl Pts',(-14.4421509241428,35.078778187705,7.99968953263258));
#51104=CARTESIAN_POINT('Ctrl Pts',(-15.0085240779375,35.0755694115626,7.99971384012147));
#51105=CARTESIAN_POINT('Ctrl Pts',(-14.150736560916,35.0470814239072,8.48567350216556));
#51106=CARTESIAN_POINT('Ctrl Pts',(-14.4420020169164,35.0436268600821,7.99995828626213));
#51107=CARTESIAN_POINT('Ctrl Pts',(-15.0083569585472,35.0418501545842,7.99996155087807));
#51108=CARTESIAN_POINT('Ctrl Pts',(-14.150692918513,34.9712377388823,8.48574627995365));
#51109=CARTESIAN_POINT('Ctrl Pts',(-14.4419607755292,34.9733482312172,8.0000327238654));
#51110=CARTESIAN_POINT('Ctrl Pts',(-15.0083106711502,34.9744335456731,8.00003016290435));
#51111=CARTESIAN_POINT('Ctrl Pts',(-14.1508066226917,34.9333329107061,8.48555667952094));
#51112=CARTESIAN_POINT('Ctrl Pts',(-14.4420682290436,34.9382240120611,7.99983879114063));
#51113=CARTESIAN_POINT('Ctrl Pts',(-15.0084312664928,34.940740365072,7.99985141504979));
#51114=CARTESIAN_POINT('Ctrl Pts',(-14.1520509011363,34.7438936238919,8.48348153993902));
#51115=CARTESIAN_POINT('Ctrl Pts',(-14.4432440959225,34.7626780463408,7.99771623713472));
#51116=CARTESIAN_POINT('Ctrl Pts',(-15.0097509557443,34.7723498879043,7.9978950544351));
#51117=CARTESIAN_POINT('Ctrl Pts',(-14.1552091806869,34.5926136214512,8.4782167591127));
#51118=CARTESIAN_POINT('Ctrl Pts',(-14.4462304856527,34.6224662811345,7.99232810421143));
#51119=CARTESIAN_POINT('Ctrl Pts',(-15.0131006462177,34.6378787746227,7.99293162477818));
#51120=CARTESIAN_POINT('Ctrl Pts',(-14.1631498026642,34.366097861864,8.46494029855902));
#51121=CARTESIAN_POINT('Ctrl Pts',(-14.4537301008296,34.4126736274608,7.97875461899514));
#51122=CARTESIAN_POINT('Ctrl Pts',(-15.0215225179599,34.4365314327682,7.98041509627186));
#51123=CARTESIAN_POINT('Ctrl Pts',(-14.1663304572642,34.2906600038508,8.45961782992988));
#51124=CARTESIAN_POINT('Ctrl Pts',(-14.4567347009781,34.34279668575,7.97331176954809));
#51125=CARTESIAN_POINT('Ctrl Pts',(-15.0248959395469,34.3694755589792,7.975397280748));
#51126=CARTESIAN_POINT('Ctrl Pts',(-14.1718962020967,34.1776041375939,8.45028822882502));
#51127=CARTESIAN_POINT('Ctrl Pts',(-14.4619896761171,34.2381138641883,7.96377525778024));
#51128=CARTESIAN_POINT('Ctrl Pts',(-15.0307990022117,34.2689814556387,7.96660169720576));
#51129=CARTESIAN_POINT('Ctrl Pts',(-14.1738839055404,34.1399356702887,8.44695401845093));
#51130=CARTESIAN_POINT('Ctrl Pts',(-14.4638665061005,34.2032333257984,7.96036678089891));
#51131=CARTESIAN_POINT('Ctrl Pts',(-15.0329071725568,34.2354983735906,7.96345833389448));
#51132=CARTESIAN_POINT('Ctrl Pts',(-14.1781231744824,34.0646323657967,8.43983651540518));
#51133=CARTESIAN_POINT('Ctrl Pts',(-14.4678686428001,34.1335117477056,7.95309163191476));
#51134=CARTESIAN_POINT('Ctrl Pts',(-15.0374033668614,34.1685621029298,7.95674823001028));
#51135=CARTESIAN_POINT('Ctrl Pts',(-14.1803761277451,34.026976116557,8.43605088762219));
#51136=CARTESIAN_POINT('Ctrl Pts',(-14.4699954006696,34.0986496666099,7.9492223146372));
#51137=CARTESIAN_POINT('Ctrl Pts',(-15.039792862775,34.1350898813783,7.953179288052));
#51138=CARTESIAN_POINT('Ctrl Pts',(-14.2018025764259,33.6887269670264,8.40001146214908));
#51139=CARTESIAN_POINT('Ctrl Pts',(-14.4902406725494,33.7851897713294,7.91234974711415));
#51140=CARTESIAN_POINT('Ctrl Pts',(-15.062517883968,33.8344239707358,7.91920272479425));
#51141=CARTESIAN_POINT('Ctrl Pts',(-14.2289622534947,33.3934618841932,8.35411823426493));
#51142=CARTESIAN_POINT('Ctrl Pts',(-14.5159096719755,33.5118586162235,7.86536934014895));
#51143=CARTESIAN_POINT('Ctrl Pts',(-15.091323602403,33.5719661192377,7.87593638279283));
#51144=CARTESIAN_POINT('Ctrl Pts',(-14.297587136116,32.8129757621643,8.2361192541527));
#51145=CARTESIAN_POINT('Ctrl Pts',(-14.5804718486074,32.975939942154,7.74503244923851));
#51146=CARTESIAN_POINT('Ctrl Pts',(-15.1641075683963,33.0559784553022,7.76469155241571));
#51147=CARTESIAN_POINT('Ctrl Pts',(-14.3390533631708,32.5277562904371,8.16400873147055));
#51148=CARTESIAN_POINT('Ctrl Pts',(-14.6194905451471,32.7128565901746,7.67142630106037));
#51149=CARTESIAN_POINT('Ctrl Pts',(-15.2080869006233,32.8024500359307,7.6967085685757));
#51150=CARTESIAN_POINT('Ctrl Pts',(-14.4344512245411,31.9668958072417,7.99412958149491));
#51151=CARTESIAN_POINT('Ctrl Pts',(-14.7087759143519,32.1972833069676,7.49877760542043));
#51152=CARTESIAN_POINT('Ctrl Pts',(-15.3092664499803,32.3039073842282,7.53655314061732));
#51153=CARTESIAN_POINT('Ctrl Pts',(-14.4883838105694,31.691255013237,7.89636074701349));
#51154=CARTESIAN_POINT('Ctrl Pts',(-14.7592010426945,31.9443746233512,7.39939956315832));
#51155=CARTESIAN_POINT('Ctrl Pts',(-15.3664676782412,32.0588933451493,7.44438050229219));
#51156=CARTESIAN_POINT('Ctrl Pts',(-14.5550635668316,31.3864313723232,7.77176756628671));
#51157=CARTESIAN_POINT('Ctrl Pts',(-14.8209199446041,31.6669143175934,7.27386759669347));
#51158=CARTESIAN_POINT('Ctrl Pts',(-15.4371886314425,31.7879389976144,7.32691891770422));
#51159=CARTESIAN_POINT('Ctrl Pts',(-14.5625558613898,31.352635473547,7.75772049298618));
#51160=CARTESIAN_POINT('Ctrl Pts',(-14.827877420134,31.6360499048315,7.25966604997201));
#51161=CARTESIAN_POINT('Ctrl Pts',(-15.4451350045509,31.7578981987159,7.31367588564878));
#51162=CARTESIAN_POINT('Ctrl Pts',(-14.5777038502899,31.2851903557158,7.72921800162461));
#51163=CARTESIAN_POINT('Ctrl Pts',(-14.8419359589025,31.5744837961381,7.2308617271771));
#51164=CARTESIAN_POINT('Ctrl Pts',(-15.4612010532912,31.697946982851,7.28680485001122));
#51165=CARTESIAN_POINT('Ctrl Pts',(-14.5853648004003,31.2515184553974,7.71475260653216));
#51166=CARTESIAN_POINT('Ctrl Pts',(-14.849042235293,31.543760796002,7.21624805914054));
#51167=CARTESIAN_POINT('Ctrl Pts',(-15.469326303495,31.6680164047788,7.2731674405612));
#51168=CARTESIAN_POINT('Ctrl Pts',(-14.6085452032034,31.1509057610832,7.67082157327148));
#51169=CARTESIAN_POINT('Ctrl Pts',(-14.8705436711721,31.4519516854403,7.171859977806));
#51170=CARTESIAN_POINT('Ctrl Pts',(-15.4939115790748,31.5785828987784,7.2317509780494));
#51171=CARTESIAN_POINT('Ctrl Pts',(-14.6242529880176,31.0844047949656,7.64083891095088));
#51172=CARTESIAN_POINT('Ctrl Pts',(-14.8850903709531,31.3913603681064,7.14160216923058));
#51173=CARTESIAN_POINT('Ctrl Pts',(-15.5105713510105,31.5194709288242,7.20348449527989));
#51174=CARTESIAN_POINT('Ctrl Pts',(-14.6720790763943,30.8865851637151,7.54883265535859));
#51175=CARTESIAN_POINT('Ctrl Pts',(-14.929376159556,31.2110903439192,7.04872760978158));
#51176=CARTESIAN_POINT('Ctrl Pts',(-15.5612959899498,31.3436312567038,7.11674459069576));
#51177=CARTESIAN_POINT('Ctrl Pts',(-14.7048994575313,30.7569483641181,7.48475247389081));
#51178=CARTESIAN_POINT('Ctrl Pts',(-14.95966877612,31.0933259986506,6.98419535501427));
#51179=CARTESIAN_POINT('Ctrl Pts',(-15.5961054854356,31.2283985458312,7.05633229878906));
#51180=CARTESIAN_POINT('Ctrl Pts',(-14.8057173802565,30.3745068040017,7.28444119078806));
#51181=CARTESIAN_POINT('Ctrl Pts',(-15.052677543726,30.7458140689667,6.78241054451384));
#51182=CARTESIAN_POINT('Ctrl Pts',(-15.7030335847703,30.888450492549,6.86748664417107));
#51183=CARTESIAN_POINT('Ctrl Pts',(-14.8760647694745,30.1281517423914,7.14016324914458));
#51184=CARTESIAN_POINT('Ctrl Pts',(-15.1171363078512,30.5235314070459,6.63773030177344));
#51185=CARTESIAN_POINT('Ctrl Pts',(-15.7776444528623,30.6694682154397,6.73146703642075));
#51186=CARTESIAN_POINT('Ctrl Pts',(-15.0208334639485,29.6517703450343,6.83035843117765));
#51187=CARTESIAN_POINT('Ctrl Pts',(-15.2487759421767,30.0960400709944,6.32894683063836));
#51188=CARTESIAN_POINT('Ctrl Pts',(-15.9311870068286,30.2460180844943,6.43939515378203));
#51189=CARTESIAN_POINT('Ctrl Pts',(-15.0952589444123,29.4217455787918,6.66483128140236));
#51190=CARTESIAN_POINT('Ctrl Pts',(-15.3160581108554,29.8908120505933,6.16445964685839));
#51191=CARTESIAN_POINT('Ctrl Pts',(-16.0101231232976,30.0415516256819,6.28334262225704));
#51192=CARTESIAN_POINT('Ctrl Pts',(-15.1895776666482,29.1442442832826,6.4443022486447));
#51193=CARTESIAN_POINT('Ctrl Pts',(-15.4001942830716,29.6459545222953,5.94785171931794));
#51194=CARTESIAN_POINT('Ctrl Pts',(-16.1101581311846,29.79488380734,6.07543646335386));
#51195=CARTESIAN_POINT('Ctrl Pts',(-15.2085060076969,29.0892469278519,6.39951354132192));
#51196=CARTESIAN_POINT('Ctrl Pts',(-15.4171256703624,29.5972806483711,5.90370851153158));
#51197=CARTESIAN_POINT('Ctrl Pts',(-16.1302336446393,29.745997269232,6.03321141943556));
#51198=CARTESIAN_POINT('Ctrl Pts',(-15.2369722744217,29.0075062116329,6.33129394724583));
#51199=CARTESIAN_POINT('Ctrl Pts',(-15.4425151412656,29.5251196490867,5.83662745356123));
#51200=CARTESIAN_POINT('Ctrl Pts',(-16.160425139482,29.6733388547696,5.96889665059839));
#51201=CARTESIAN_POINT('Ctrl Pts',(-15.246473323653,28.980385210548,6.30838130181911));
#51202=CARTESIAN_POINT('Ctrl Pts',(-15.4509873595446,29.5011789547939,5.81409473052649));
#51203=CARTESIAN_POINT('Ctrl Pts',(-16.170502009992,29.6492312982821,5.94729550340031));
#51204=CARTESIAN_POINT('Ctrl Pts',(-15.2654961612181,28.926395398229,6.26220810975159));
#51205=CARTESIAN_POINT('Ctrl Pts',(-15.4679323239667,29.4535620737581,5.76872117594484));
#51206=CARTESIAN_POINT('Ctrl Pts',(-16.1906777466895,29.601240353964,5.90376522131281));
#51207=CARTESIAN_POINT('Ctrl Pts',(-15.2750230398706,28.8995124220965,6.23893492398287));
#51208=CARTESIAN_POINT('Ctrl Pts',(-15.4764096537653,29.4298736780045,5.74586728371073));
#51209=CARTESIAN_POINT('Ctrl Pts',(-16.2007820120252,29.5773443751773,5.88182417079429));
#51210=CARTESIAN_POINT('Ctrl Pts',(-15.3225922161938,28.7660296571919,6.12195830143935));
#51211=CARTESIAN_POINT('Ctrl Pts',(-15.5187963268113,29.3120701815224,5.63080434349472));
#51212=CARTESIAN_POINT('Ctrl Pts',(-16.2512341685254,29.4586930286934,5.77154317966401));
#51213=CARTESIAN_POINT('Ctrl Pts',(-15.3604967735573,28.6620554042277,6.02628494806573));
#51214=CARTESIAN_POINT('Ctrl Pts',(-15.552341978002,29.22088933467,5.5371846231952));
#51215=CARTESIAN_POINT('Ctrl Pts',(-16.2914359721255,29.3662714703737,5.68134607909259));
#51216=CARTESIAN_POINT('Ctrl Pts',(-15.4734024711476,28.3583437765312,5.73303598356708));
#51217=CARTESIAN_POINT('Ctrl Pts',(-15.6521452749257,28.9546179419119,5.25025045759224));
#51218=CARTESIAN_POINT('Ctrl Pts',(-16.4111844387542,29.0963055792408,5.40488240853399));
#51219=CARTESIAN_POINT('Ctrl Pts',(-15.5475928105337,28.166793334864,5.52924812560617));
#51220=CARTESIAN_POINT('Ctrl Pts',(-15.716867186315,28.7887594038429,5.0526403038573));
#51221=CARTESIAN_POINT('Ctrl Pts',(-16.4898711630596,28.9260385198999,5.21275917575155));
#51222=CARTESIAN_POINT('Ctrl Pts',(-15.6920332500668,27.804967416518,5.10493090212559));
#51223=CARTESIAN_POINT('Ctrl Pts',(-15.8416653101424,28.4777545766966,4.64442044202835));
#51224=CARTESIAN_POINT('Ctrl Pts',(-16.6430655678803,28.6044154813285,4.8127294699215));
#51225=CARTESIAN_POINT('Ctrl Pts',(-15.7622877731009,27.6346927109898,4.88440241921411));
#51226=CARTESIAN_POINT('Ctrl Pts',(-15.9016653391294,28.3329345034696,4.43369484971485));
#51227=CARTESIAN_POINT('Ctrl Pts',(-16.7175779415832,28.4530601877117,4.6048238295626));
#51228=CARTESIAN_POINT('Ctrl Pts',(-15.8634153592665,27.3953869383753,4.54052076838177));
#51229=CARTESIAN_POINT('Ctrl Pts',(-15.9868838517309,28.1316515312056,4.10893296665195));
#51230=CARTESIAN_POINT('Ctrl Pts',(-16.8248344717416,28.2403439451399,4.280625640225));
#51231=CARTESIAN_POINT('Ctrl Pts',(-15.8964154242514,27.3183086387693,4.42370773816891));
#51232=CARTESIAN_POINT('Ctrl Pts',(-16.0146143413019,28.0669533026489,3.99868427600105));
#51233=CARTESIAN_POINT('Ctrl Pts',(-16.8598345410939,28.1718299012522,4.17049887771516));
#51234=CARTESIAN_POINT('Ctrl Pts',(-15.9446833059184,27.2068010501802,4.24510042840518));
#51235=CARTESIAN_POINT('Ctrl Pts',(-16.0548906467027,27.9739186191265,3.83109036355919));
#51236=CARTESIAN_POINT('Ctrl Pts',(-16.9110277485907,28.0727120445427,4.00211488200807));
#51237=CARTESIAN_POINT('Ctrl Pts',(-15.9605671695884,27.1703172329925,4.18499971903105));
#51238=CARTESIAN_POINT('Ctrl Pts',(-16.0681256678962,27.9435097431242,3.7747202284785));
#51239=CARTESIAN_POINT('Ctrl Pts',(-16.9278742708902,28.0402819849552,3.94545428055366));
#51240=CARTESIAN_POINT('Ctrl Pts',(-15.9840630498228,27.1166326670936,4.09398463298263));
#51241=CARTESIAN_POINT('Ctrl Pts',(-16.0876324266849,27.8989052244231,3.68960145288528));
#51242=CARTESIAN_POINT('Ctrl Pts',(-16.9527941436941,27.9925623707134,3.85964881224669));
#51243=CARTESIAN_POINT('Ctrl Pts',(-15.9918400182461,27.098911365518,4.06350224576308));
#51244=CARTESIAN_POINT('Ctrl Pts',(-16.0940844067552,27.8841885644318,3.66110082717283));
#51245=CARTESIAN_POINT('Ctrl Pts',(-16.9610424436527,27.9768101027221,3.83091120811858));
#51246=CARTESIAN_POINT('Ctrl Pts',(-16.0072802673827,27.0638183876329,4.00224638321511));
#51247=CARTESIAN_POINT('Ctrl Pts',(-16.1068754781049,27.8550811453129,3.60388755733143));
#51248=CARTESIAN_POINT('Ctrl Pts',(-16.9774184653475,27.9456163445231,3.77316157340969));
#51249=CARTESIAN_POINT('Ctrl Pts',(-16.0149484597681,27.0464356133835,3.97145286285566));
#51250=CARTESIAN_POINT('Ctrl Pts',(-16.11321832627,27.8406819961272,3.57515643717542));
#51251=CARTESIAN_POINT('Ctrl Pts',(-16.9855513967497,27.9301649896533,3.74413064513307));
#51252=CARTESIAN_POINT('Ctrl Pts',(-16.0833253347986,26.8918211440726,3.69342860679508));
#51253=CARTESIAN_POINT('Ctrl Pts',(-16.1700064472163,27.7120571742295,3.3145971632474));
#51254=CARTESIAN_POINT('Ctrl Pts',(-17.0580723245784,27.7927299060094,3.48202023522934));
#51255=CARTESIAN_POINT('Ctrl Pts',(-16.1392489563977,26.7681000791065,3.44139585389464));
#51256=CARTESIAN_POINT('Ctrl Pts',(-16.2154998129262,27.611079704592,3.08181765987248));
#51257=CARTESIAN_POINT('Ctrl Pts',(-17.1173852570175,27.6827556258494,3.24441359968121));
#51258=CARTESIAN_POINT('Ctrl Pts',(-16.2403199527415,26.5474550953827,2.92755360879577));
#51259=CARTESIAN_POINT('Ctrl Pts',(-16.2970459414564,27.4321275309776,2.61077340535992));
#51260=CARTESIAN_POINT('Ctrl Pts',(-17.2245817678271,27.4866267514743,2.7599832001616));
#51261=CARTESIAN_POINT('Ctrl Pts',(-16.2854701813921,26.4505327273823,2.66574409615585));
#51262=CARTESIAN_POINT('Ctrl Pts',(-16.3329171219314,27.3545890540287,2.37293766614214));
#51263=CARTESIAN_POINT('Ctrl Pts',(-17.272468374468,27.4004735355853,2.51315941724635));
#51264=CARTESIAN_POINT('Ctrl Pts',(-16.3638891417636,26.2837240365077,2.13210289884751));
#51265=CARTESIAN_POINT('Ctrl Pts',(-16.3948333150909,27.2217630392128,1.89119238259305));
#51266=CARTESIAN_POINT('Ctrl Pts',(-17.3556399985759,27.252199143428,2.01006333898577));
#51267=CARTESIAN_POINT('Ctrl Pts',(-16.3971609665106,26.2138347665803,1.86027258862789));
#51268=CARTESIAN_POINT('Ctrl Pts',(-16.4207214647061,27.1668306081169,1.64783726428005));
#51269=CARTESIAN_POINT('Ctrl Pts',(-17.3909282981186,27.1900753483798,1.75379233941467));
#51270=CARTESIAN_POINT('Ctrl Pts',(-16.4372282316227,26.1301157641184,1.44461189527185));
#51271=CARTESIAN_POINT('Ctrl Pts',(-16.4517534962573,27.1012636221844,1.27786031263812));
#51272=CARTESIAN_POINT('Ctrl Pts',(-17.4334238818719,27.1156584568399,1.36192367232642));
#51273=CARTESIAN_POINT('Ctrl Pts',(-16.4489425836071,26.1057357203802,1.30473676381471));
#51274=CARTESIAN_POINT('Ctrl Pts',(-16.4607946572,27.0822242725002,1.15354204459136));
#51275=CARTESIAN_POINT('Ctrl Pts',(-17.4458481948988,27.0939873072066,1.23005486149115));
#51276=CARTESIAN_POINT('Ctrl Pts',(-16.4614235356195,26.0798156556365,1.12817920332052));
#51277=CARTESIAN_POINT('Ctrl Pts',(-16.4704032550175,27.0620254439469,0.997028004066201));
#51278=CARTESIAN_POINT('Ctrl Pts',(-17.4590855680403,27.0709472494042,1.06360328933017));
#51279=CARTESIAN_POINT('Ctrl Pts',(-16.4638105601819,26.074861696503,1.09279299652423));
#51280=CARTESIAN_POINT('Ctrl Pts',(-16.4722410434965,27.0581642796167,0.965648605363661));
#51281=CARTESIAN_POINT('Ctrl Pts',(-17.4616172607913,27.0665437301925,1.03024255564937));
#51282=CARTESIAN_POINT('Ctrl Pts',(-16.4683507346043,26.0654443842168,1.02209528756755));
#51283=CARTESIAN_POINT('Ctrl Pts',(-16.4757345383337,27.0508278725685,0.902983985062077));
#51284=CARTESIAN_POINT('Ctrl Pts',(-17.4664325973152,27.0581727860028,0.963591516895074));
#51285=CARTESIAN_POINT('Ctrl Pts',(-16.470506063436,26.0609765048028,0.986753620408229));
#51286=CARTESIAN_POINT('Ctrl Pts',(-16.4773917386444,27.047349490258,0.871673646590079));
#51287=CARTESIAN_POINT('Ctrl Pts',(-17.4687185521219,27.0542013375728,0.930272773451819));
#51288=CARTESIAN_POINT('Ctrl Pts',(-16.4766286018102,26.0482910800257,0.880750072548012));
#51289=CARTESIAN_POINT('Ctrl Pts',(-16.4820979767805,27.0374753525219,0.777776718980477));
#51290=CARTESIAN_POINT('Ctrl Pts',(-17.4752121534494,27.0429254045267,0.830336768726166));
#51291=CARTESIAN_POINT('Ctrl Pts',(-16.4802523787863,26.0407916272951,0.810109642405695));
#51292=CARTESIAN_POINT('Ctrl Pts',(-16.4848785011,27.0316471633613,0.715279089642234));
#51293=CARTESIAN_POINT('Ctrl Pts',(-17.4790555532451,27.0362592242133,0.763739730217897));
#51294=CARTESIAN_POINT('Ctrl Pts',(-16.4897560121036,26.0211373031105,0.598273404163521));
#51295=CARTESIAN_POINT('Ctrl Pts',(-16.4921690314085,27.0163743171162,0.527896985305773));
#51296=CARTESIAN_POINT('Ctrl Pts',(-17.4891351643784,27.0187887139739,0.564028798530454));
#51297=CARTESIAN_POINT('Ctrl Pts',(-16.4942684087839,26.0118246449525,0.457162601989202));
#51298=CARTESIAN_POINT('Ctrl Pts',(-16.4956179815424,27.0091615199262,0.403342719886046));
#51299=CARTESIAN_POINT('Ctrl Pts',(-17.4939210395996,27.0105107954566,0.430995045648165));
#51300=CARTESIAN_POINT('Ctrl Pts',(-16.4996728834952,26.0006733566253,0.175164846125518));
#51301=CARTESIAN_POINT('Ctrl Pts',(-16.4997511923146,27.0005192273558,0.154469345431858));
#51302=CARTESIAN_POINT('Ctrl Pts',(-17.4996530582721,27.0005985392793,0.165138575470091));
#51303=CARTESIAN_POINT('Ctrl Pts',(-16.5005649496479,25.9988348222276,0.0342778948658427));
#51304=CARTESIAN_POINT('Ctrl Pts',(-16.5004319098763,26.9990972249887,0.0302562756544078));
#51305=CARTESIAN_POINT('Ctrl Pts',(-17.5005991890068,26.9989642864088,0.0323158604794608));
#51306=CARTESIAN_POINT('Ctrl Pts',(-16.4978390182597,26.0044568076987,-0.388049293380772));
#51307=CARTESIAN_POINT('Ctrl Pts',(-16.4983485327184,27.0034518225239,-0.342280149680354));
#51308=CARTESIAN_POINT('Ctrl Pts',(-17.4977080496968,27.0039616068747,-0.365837717665129));
#51309=CARTESIAN_POINT('Ctrl Pts',(-16.4888223219516,26.0230271690527,-0.669156567504712));
#51310=CARTESIAN_POINT('Ctrl Pts',(-16.4914905865413,27.0177691015244,-0.589955966903106));
#51311=CARTESIAN_POINT('Ctrl Pts',(-17.4881448869157,27.020468594845,-0.630854676420441));
#51312=CARTESIAN_POINT('Ctrl Pts',(-16.4645479010849,26.0733210916423,-1.09014697727432));
#51313=CARTESIAN_POINT('Ctrl Pts',(-16.4728185592198,27.0569442887207,-0.963125072170838));
#51314=CARTESIAN_POINT('Ctrl Pts',(-17.4623992890308,27.0651743036164,-1.02774799205062));
#51315=CARTESIAN_POINT('Ctrl Pts',(-16.4546639962014,26.0938323280556,-1.23036518951515));
#51316=CARTESIAN_POINT('Ctrl Pts',(-16.4652151995949,27.0729175749462,-1.08745697835527));
#51317=CARTESIAN_POINT('Ctrl Pts',(-17.4519163596122,27.0834065139337,-1.15994024599047));
#51318=CARTESIAN_POINT('Ctrl Pts',(-16.4400673858426,26.1242298032478,-1.40549624934421));
#51319=CARTESIAN_POINT('Ctrl Pts',(-16.4539221087833,27.0967120128198,-1.2433380557798));
#51320=CARTESIAN_POINT('Ctrl Pts',(-17.4364351061955,27.1104264917492,-1.32504696908299));
#51321=CARTESIAN_POINT('Ctrl Pts',(-16.4370359610415,26.130547367242,-1.44051537232677));
#51322=CARTESIAN_POINT('Ctrl Pts',(-16.4515773822401,27.1016553378582,-1.27449396665141));
#51323=CARTESIAN_POINT('Ctrl Pts',(-17.433219958682,27.1160421042443,-1.35806163047139));
#51324=CARTESIAN_POINT('Ctrl Pts',(-16.4307488113996,26.1436611143959,-1.51053938021269));
#51325=CARTESIAN_POINT('Ctrl Pts',(-16.4467096966894,27.1119250811992,-1.33683413188026));
#51326=CARTESIAN_POINT('Ctrl Pts',(-17.4265517696646,27.1276987683228,-1.42407753017187));
#51327=CARTESIAN_POINT('Ctrl Pts',(-16.4274906111759,26.1504624708553,-1.54556967700777));
#51328=CARTESIAN_POINT('Ctrl Pts',(-16.4441850672634,27.1172550250431,-1.36803947412004));
#51329=CARTESIAN_POINT('Ctrl Pts',(-17.4230961027206,27.1337444184933,-1.45710272580348));
#51330=CARTESIAN_POINT('Ctrl Pts',(-16.4173982522689,26.1715491252668,-1.65044486531198));
#51331=CARTESIAN_POINT('Ctrl Pts',(-16.43635996178,27.1337879226008,-1.46149208806462));
#51332=CARTESIAN_POINT('Ctrl Pts',(-17.4123920858232,27.1524881114378,-1.55597495718666));
#51333=CARTESIAN_POINT('Ctrl Pts',(-16.4102542800575,26.186500310749,-1.72000002026246));
#51334=CARTESIAN_POINT('Ctrl Pts',(-16.4308099461936,27.1455302764211,-1.52357398570511));
#51335=CARTESIAN_POINT('Ctrl Pts',(-17.4048151454351,27.1657780539216,-1.62154884066042));
#51336=CARTESIAN_POINT('Ctrl Pts',(-16.3725127956242,26.2656547133766,-2.06599962503883));
#51337=CARTESIAN_POINT('Ctrl Pts',(-16.4014953816007,27.2076634406906,-1.83207874075241));
#51338=CARTESIAN_POINT('Ctrl Pts',(-17.3647862987107,27.2361375233113,-1.94774375420961));
#51339=CARTESIAN_POINT('Ctrl Pts',(-16.3358579567688,26.3430155684638,-2.33712916293811));
#51340=CARTESIAN_POINT('Ctrl Pts',(-16.3728357498743,27.2687196259979,-2.07564354115728));
#51341=CARTESIAN_POINT('Ctrl Pts',(-17.3259099538696,27.3049027273893,-2.20335409300917));
#51342=CARTESIAN_POINT('Ctrl Pts',(-16.2509489421038,26.5246876648651,-2.86863842077008));
#51343=CARTESIAN_POINT('Ctrl Pts',(-16.3054421715168,27.4140279801895,-2.55725670467926));
#51344=CARTESIAN_POINT('Ctrl Pts',(-17.2358549388741,27.4663890355697,-2.70444026200191));
#51345=CARTESIAN_POINT('Ctrl Pts',(-16.2026914231958,26.6290018643058,-3.12901661081332));
#51346=CARTESIAN_POINT('Ctrl Pts',(-16.2668736654531,27.4979009908363,-2.79478543759917));
#51347=CARTESIAN_POINT('Ctrl Pts',(-17.1846727213246,27.5591127682956,-2.94991464986886));
#51348=CARTESIAN_POINT('Ctrl Pts',(-16.1224929527533,26.8055233058917,-3.511724585575));
#51349=CARTESIAN_POINT('Ctrl Pts',(-16.2015927972012,27.6422088112504,-3.14811650491222));
#51350=CARTESIAN_POINT('Ctrl Pts',(-17.099613737892,27.7160207163362,-3.31071678104154));
#51351=CARTESIAN_POINT('Ctrl Pts',(-16.0944573592689,26.8677122005455,-3.6379817080266));
#51352=CARTESIAN_POINT('Ctrl Pts',(-16.1787224577041,27.6931119961222,-3.2648130549793));
#51353=CARTESIAN_POINT('Ctrl Pts',(-17.0698790172897,27.7712997338665,-3.42974706475798));
#51354=CARTESIAN_POINT('Ctrl Pts',(-16.0578742587549,26.9496675749635,-3.79416704657873));
#51355=CARTESIAN_POINT('Ctrl Pts',(-16.1486081613594,27.7607465434304,-3.4101345555538));
#51356=CARTESIAN_POINT('Ctrl Pts',(-17.0310787593147,27.844148955511,-3.57699250183713));
#51357=CARTESIAN_POINT('Ctrl Pts',(-16.0504807062728,26.9662697489414,-3.82532226629593));
#51358=CARTESIAN_POINT('Ctrl Pts',(-16.1425271619055,27.7744328577361,-3.43908652601369));
#51359=CARTESIAN_POINT('Ctrl Pts',(-17.0232371126848,27.8589064435178,-3.60636442612413));
#51360=CARTESIAN_POINT('Ctrl Pts',(-16.0355419811776,26.999897690748,-3.88746893406826));
#51361=CARTESIAN_POINT('Ctrl Pts',(-16.1302215604399,27.8021911773562,-3.49689960574396));
#51362=CARTESIAN_POINT('Ctrl Pts',(-17.0073930103687,27.8887979473173,-3.66495387724952));
#51363=CARTESIAN_POINT('Ctrl Pts',(-16.0279925473271,27.0169331053863,-3.91847760489801));
#51364=CARTESIAN_POINT('Ctrl Pts',(-16.1239938076285,27.8162702352096,-3.52577621154247));
#51365=CARTESIAN_POINT('Ctrl Pts',(-16.9993860349865,27.9039405380826,-3.69418764098899));
#51366=CARTESIAN_POINT('Ctrl Pts',(-16.005151309949,27.0686067279126,-4.01113187201297));
#51367=CARTESIAN_POINT('Ctrl Pts',(-16.1051372201557,27.8589989859183,-3.61208369701427));
#51368=CARTESIAN_POINT('Ctrl Pts',(-16.9751604803637,27.9498726471105,-3.78153846518201));
#51369=CARTESIAN_POINT('Ctrl Pts',(-15.9896858552224,27.1037684311926,-4.07232971282369));
#51370=CARTESIAN_POINT('Ctrl Pts',(-16.0923233519077,27.8881659099294,-3.66925480659103));
#51371=CARTESIAN_POINT('Ctrl Pts',(-16.9587577251248,27.9811274943278,-3.8392333993061));
#51372=CARTESIAN_POINT('Ctrl Pts',(-15.9112419315778,27.2830923847797,-4.37551697666845));
#51373=CARTESIAN_POINT('Ctrl Pts',(-16.0274373719239,28.0366047023604,-3.95173322375266));
#51374=CARTESIAN_POINT('Ctrl Pts',(-16.875559624845,28.1405265645112,-4.1250665099463));
#51375=CARTESIAN_POINT('Ctrl Pts',(-15.844918315659,27.4377681716844,-4.60912492170408));
#51376=CARTESIAN_POINT('Ctrl Pts',(-15.9717543805869,28.166270657865,-4.1723242724571));
#51377=CARTESIAN_POINT('Ctrl Pts',(-16.8052163950039,28.2780161525077,-4.34530295645177));
#51378=CARTESIAN_POINT('Ctrl Pts',(-15.7069099448858,27.7688775711428,-5.05949097805553));
#51379=CARTESIAN_POINT('Ctrl Pts',(-15.8543812193166,28.447094636339,-4.60083479731583));
#51380=CARTESIAN_POINT('Ctrl Pts',(-16.6588438813315,28.5723356188943,-4.76989048439904));
#51381=CARTESIAN_POINT('Ctrl Pts',(-15.6352206245408,27.9453128342832,-5.27624649105232));
#51382=CARTESIAN_POINT('Ctrl Pts',(-15.7928000382307,28.5978883814961,-4.80878789175796));
#51383=CARTESIAN_POINT('Ctrl Pts',(-16.5828097529458,28.7291669638434,-4.97423911600232));
#51384=CARTESIAN_POINT('Ctrl Pts',(-15.5249581839362,28.2263776622186,-5.58908746041189));
#51385=CARTESIAN_POINT('Ctrl Pts',(-15.696693052097,28.8413995443161,-5.11191611245));
#51386=CARTESIAN_POINT('Ctrl Pts',(-16.4658647407159,28.9790023663985,-5.26917336342192));
#51387=CARTESIAN_POINT('Ctrl Pts',(-15.4877493740823,28.3228072898136,-5.69131489459601));
#51388=CARTESIAN_POINT('Ctrl Pts',(-15.6642132176884,28.9249883773396,-5.21099932125141));
#51389=CARTESIAN_POINT('Ctrl Pts',(-16.4264008511294,29.0647175909937,-5.36554939547687));
#51390=CARTESIAN_POINT('Ctrl Pts',(-15.431421554897,28.4716312472057,-5.84158285664235));
#51391=CARTESIAN_POINT('Ctrl Pts',(-15.6147184969787,29.0547764285091,-5.3573483822539));
#51392=CARTESIAN_POINT('Ctrl Pts',(-16.3666592249758,29.1970055530476,-5.50721616119523));
#51393=CARTESIAN_POINT('Ctrl Pts',(-15.4125599052749,28.5219362190851,-5.8911597188493));
#51394=CARTESIAN_POINT('Ctrl Pts',(-15.5981338876659,29.098657869549,-5.40563341726845));
#51395=CARTESIAN_POINT('Ctrl Pts',(-16.3466544449051,29.2417210836625,-5.55395529043817));
#51396=CARTESIAN_POINT('Ctrl Pts',(-15.3841604516061,28.5984513320056,-5.9647546987206));
#51397=CARTESIAN_POINT('Ctrl Pts',(-15.5730837024597,29.1655935118162,-5.47748185994016));
#51398=CARTESIAN_POINT('Ctrl Pts',(-16.3165338123512,29.3097345173226,-5.62333776313334));
#51399=CARTESIAN_POINT('Ctrl Pts',(-15.3746761425149,28.6241326720875,-5.98915795629746));
#51400=CARTESIAN_POINT('Ctrl Pts',(-15.5647153050045,29.1880623175047,-5.50130549482725));
#51401=CARTESIAN_POINT('Ctrl Pts',(-16.3064746965653,29.3325623752064,-5.64634420119125));
#51402=CARTESIAN_POINT('Ctrl Pts',(-15.3556755438085,28.6758503150148,-6.03770718948676));
#51403=CARTESIAN_POINT('Ctrl Pts',(-15.547931168814,29.2333546452359,-5.54873830674073));
#51404=CARTESIAN_POINT('Ctrl Pts',(-16.2863225465049,29.3785336133291,-5.69211452210701));
#51405=CARTESIAN_POINT('Ctrl Pts',(-15.3461631123057,28.7018763061624,-6.06184308744346));
#51406=CARTESIAN_POINT('Ctrl Pts',(-15.5395188506324,29.2561687234751,-5.57233816417615));
#51407=CARTESIAN_POINT('Ctrl Pts',(-16.2762336039025,29.4016678276794,-5.71486890398771));
#51408=CARTESIAN_POINT('Ctrl Pts',(-15.2606323097608,28.9371409426806,-6.27738721348527));
#51409=CARTESIAN_POINT('Ctrl Pts',(-15.4642290688267,29.4614132947124,-5.7820464495127));
#51410=CARTESIAN_POINT('Ctrl Pts',(-16.1855191168777,29.610791949213,-5.918075487456));
#51411=CARTESIAN_POINT('Ctrl Pts',(-15.1848342114096,29.1545099575102,-6.45796308382094));
#51412=CARTESIAN_POINT('Ctrl Pts',(-15.3964943458008,29.6534800554759,-5.96008229317087));
#51413=CARTESIAN_POINT('Ctrl Pts',(-16.1051271935059,29.8040088510832,-6.08831536510389));
#51414=CARTESIAN_POINT('Ctrl Pts',(-15.0356595911467,29.6056859311573,-6.79804515130241));
#51415=CARTESIAN_POINT('Ctrl Pts',(-15.2622391988625,30.0548640664217,-6.29665836970821));
#51416=CARTESIAN_POINT('Ctrl Pts',(-15.9469116879931,30.2050541610657,-6.40893145588782));
#51417=CARTESIAN_POINT('Ctrl Pts',(-14.9622788975724,29.8394929473934,-6.95754936214554));
#51418=CARTESIAN_POINT('Ctrl Pts',(-15.1956484255345,30.2641311892708,-6.45556673433959));
#51419=CARTESIAN_POINT('Ctrl Pts',(-15.8690836788716,30.4128826199675,-6.55930579570915));
#51420=CARTESIAN_POINT('Ctrl Pts',(-14.8199953655875,30.3240935251076,-7.25568882321979));
#51421=CARTESIAN_POINT('Ctrl Pts',(-15.0658271140403,30.7002416979089,-6.75341440551023));
#51422=CARTESIAN_POINT('Ctrl Pts',(-15.7181769032676,30.8436386889222,-6.8403800356117));
#51423=CARTESIAN_POINT('Ctrl Pts',(-14.7510880041712,30.5748839284072,-7.39432626488165));
#51424=CARTESIAN_POINT('Ctrl Pts',(-15.0024895581545,30.9271154442475,-6.89273010331883));
#51425=CARTESIAN_POINT('Ctrl Pts',(-15.645093337422,31.0665634920556,-6.9710820001448));
#51426=CARTESIAN_POINT('Ctrl Pts',(-14.6691811405517,30.8997312170887,-7.55423164883944));
#51427=CARTESIAN_POINT('Ctrl Pts',(-14.9266314159884,31.2233129771628,-7.0542966399533));
#51428=CARTESIAN_POINT('Ctrl Pts',(-15.5582224218811,31.3553166373777,-7.12183455119867));
#51429=CARTESIAN_POINT('Ctrl Pts',(-14.653011891398,30.9652703749227,-7.5855411589654));
#51430=CARTESIAN_POINT('Ctrl Pts',(-14.9116910431975,31.2829158941087,-7.08584557342882));
#51431=CARTESIAN_POINT('Ctrl Pts',(-15.5410732180678,31.4135736666364,-7.15135193426238));
#51432=CARTESIAN_POINT('Ctrl Pts',(-14.6291056146706,31.0644531496729,-7.63148523917637));
#51433=CARTESIAN_POINT('Ctrl Pts',(-14.8895640652671,31.3732579073334,-7.13220066227062));
#51434=CARTESIAN_POINT('Ctrl Pts',(-15.5157180762066,31.5017361330234,-7.19466621881002));
#51435=CARTESIAN_POINT('Ctrl Pts',(-14.6211948006132,31.0976597721854,-7.64662987407586));
#51436=CARTESIAN_POINT('Ctrl Pts',(-14.8822417942904,31.4035020137527,-7.14747837210504));
#51437=CARTESIAN_POINT('Ctrl Pts',(-15.507327818792,31.5312531308516,-7.20894398896686));
#51438=CARTESIAN_POINT('Ctrl Pts',(-14.6054941177937,31.1643679687753,-7.67657654190212));
#51439=CARTESIAN_POINT('Ctrl Pts',(-14.867701061467,31.4642882513809,-7.17769919573129));
#51440=CARTESIAN_POINT('Ctrl Pts',(-15.4906755795184,31.5905493055579,-7.23717653788107));
#51441=CARTESIAN_POINT('Ctrl Pts',(-14.5977025585871,31.1978776275757,-7.69138168422876));
#51442=CARTESIAN_POINT('Ctrl Pts',(-14.8604807256331,31.4948381920921,-7.19264621846369));
#51443=CARTESIAN_POINT('Ctrl Pts',(-15.4824118045141,31.6203356689469,-7.2511342477555));
#51444=CARTESIAN_POINT('Ctrl Pts',(-14.5591761411658,31.3656598443161,-7.76432516797013));
#51445=CARTESIAN_POINT('Ctrl Pts',(-14.8248199038901,31.6476138839898,-7.26619003874707));
#51446=CARTESIAN_POINT('Ctrl Pts',(-15.4415504529436,31.7694754172071,-7.31990251526702));
#51447=CARTESIAN_POINT('Ctrl Pts',(-14.5296413627691,31.5010285289678,-7.81939903927279));
#51448=CARTESIAN_POINT('Ctrl Pts',(-14.7973600530408,31.7713364293414,-7.32192638233487));
#51449=CARTESIAN_POINT('Ctrl Pts',(-15.4102256876126,31.8898031368429,-7.37182401004875));
#51450=CARTESIAN_POINT('Ctrl Pts',(-14.4452230147646,31.9105732769504,-7.97492632680715));
#51451=CARTESIAN_POINT('Ctrl Pts',(-14.7189160078809,32.1454427835541,-7.47912726165049));
#51452=CARTESIAN_POINT('Ctrl Pts',(-15.3206910766111,32.2538429128796,-7.51844906238992));
#51453=CARTESIAN_POINT('Ctrl Pts',(-14.394524204208,32.1881803100535,-8.06571177616595));
#51454=CARTESIAN_POINT('Ctrl Pts',(-14.6714240271853,32.4005576020766,-7.57152225977134));
#51455=CARTESIAN_POINT('Ctrl Pts',(-15.266919610253,32.5006047200686,-7.60403803792814));
#51456=CARTESIAN_POINT('Ctrl Pts',(-14.3060495457409,32.7527931145422,-8.22161662427291));
#51457=CARTESIAN_POINT('Ctrl Pts',(-14.5884881552083,32.9202575071458,-7.73013444004218));
#51458=CARTESIAN_POINT('Ctrl Pts',(-15.1730828518141,33.0024827684609,-7.75101903992668));
#51459=CARTESIAN_POINT('Ctrl Pts',(-14.2682728616157,33.0397984670644,-8.2867370209155));
#51460=CARTESIAN_POINT('Ctrl Pts',(-14.552893734404,33.1852802024212,-7.79666355226168));
#51461=CARTESIAN_POINT('Ctrl Pts',(-15.133016671222,33.2575986374368,-7.81241200590781));
#51462=CARTESIAN_POINT('Ctrl Pts',(-14.2226573712228,33.4777284594361,-8.36462327469889));
#51463=CARTESIAN_POINT('Ctrl Pts',(-14.5098903723144,33.5903491926421,-7.87622892641895));
#51464=CARTESIAN_POINT('Ctrl Pts',(-15.0846366059366,33.6468697416979,-7.8858401244665));
#51465=CARTESIAN_POINT('Ctrl Pts',(-14.2092942502116,33.6249441231039,-8.38727953342513));
#51466=CARTESIAN_POINT('Ctrl Pts',(-14.4972860759252,33.7265132279608,-7.8993776669338));
#51467=CARTESIAN_POINT('Ctrl Pts',(-15.0704635986376,33.7777281094489,-7.90719955992493));
#51468=CARTESIAN_POINT('Ctrl Pts',(-14.1921874059586,33.8476922922332,-8.41617145140093));
#51469=CARTESIAN_POINT('Ctrl Pts',(-14.4811437317631,33.9326839034157,-7.92890420892895));
#51470=CARTESIAN_POINT('Ctrl Pts',(-15.0523199760526,33.9757264819735,-7.93443773206372));
#51471=CARTESIAN_POINT('Ctrl Pts',(-14.1869748028688,33.9222626039221,-8.42495286656801));
#51472=CARTESIAN_POINT('Ctrl Pts',(-14.4762244556026,34.0017015413618,-7.93787844712968));
#51473=CARTESIAN_POINT('Ctrl Pts',(-15.0467914575584,34.0420112034973,-7.94271650708992));
#51474=CARTESIAN_POINT('Ctrl Pts',(-14.1799126492618,34.0346090885612,-8.43682988299433));
#51475=CARTESIAN_POINT('Ctrl Pts',(-14.4695579078732,34.105716008113,-7.95001849700854));
#51476=CARTESIAN_POINT('Ctrl Pts',(-15.0393012946864,34.1418747453823,-7.95391369446155));
#51477=CARTESIAN_POINT('Ctrl Pts',(-14.1776847259483,34.0721397627187,-8.44057300476486));
#51478=CARTESIAN_POINT('Ctrl Pts',(-14.4674547435269,34.1404623010022,-7.9538444086756));
#51479=CARTESIAN_POINT('Ctrl Pts',(-15.0369383456894,34.1752353446439,-7.95744256335628));
#51480=CARTESIAN_POINT('Ctrl Pts',(-14.1745348393834,34.1285598388531,-8.44586089729133));
#51481=CARTESIAN_POINT('Ctrl Pts',(-14.4644807945682,34.192704719503,-7.95924986164786));
#51482=CARTESIAN_POINT('Ctrl Pts',(-15.0335975569284,34.2253865234225,-7.96242778198736));
#51483=CARTESIAN_POINT('Ctrl Pts',(-14.173516877044,34.1473872089809,-8.4475690610768));
#51484=CARTESIAN_POINT('Ctrl Pts',(-14.4635196895548,34.2101377324663,-7.96099596612494));
#51485=CARTESIAN_POINT('Ctrl Pts',(-15.0325178998889,34.242121963541,-7.96403817202918));
#51486=CARTESIAN_POINT('Ctrl Pts',(-14.1720382860565,34.1756594493329,-8.45004921553296));
#51487=CARTESIAN_POINT('Ctrl Pts',(-14.4621235724204,34.2363181267017,-7.96353136267135));
#51488=CARTESIAN_POINT('Ctrl Pts',(-15.0309496973357,34.2672528438503,-7.96637636482709));
#51489=CARTESIAN_POINT('Ctrl Pts',(-14.171553481119,34.1850887269927,-8.45086225174429));
#51490=CARTESIAN_POINT('Ctrl Pts',(-14.4616658100524,34.2450496654721,-7.96436249848284));
#51491=CARTESIAN_POINT('Ctrl Pts',(-15.0304355102747,34.2756344239947,-7.96714286358229));
#51492=CARTESIAN_POINT('Ctrl Pts',(-14.1706000477243,34.2039577059635,-8.45246089334986));
#51493=CARTESIAN_POINT('Ctrl Pts',(-14.4607655369268,34.2625227778338,-7.96599675441144));
#51494=CARTESIAN_POINT('Ctrl Pts',(-15.029424293044,34.2924068497441,-7.96865000047954));
#51495=CARTESIAN_POINT('Ctrl Pts',(-14.1701308662489,34.2134087629436,-8.45324742565082));
#51496=CARTESIAN_POINT('Ctrl Pts',(-14.4603225019436,34.2712748866038,-7.96680082574036));
#51497=CARTESIAN_POINT('Ctrl Pts',(-15.028926676316,34.3008077891872,-7.96939151350123));
#51498=CARTESIAN_POINT('Ctrl Pts',(-14.1696709084508,34.2228423347593,-8.45401835497186));
#51499=CARTESIAN_POINT('Ctrl Pts',(-14.4598881528388,34.2800112558736,-7.96758898230353));
#51500=CARTESIAN_POINT('Ctrl Pts',(-15.0284388422964,34.3091931864527,-7.97011831445158));
#51501=CARTESIAN_POINT('',(-15.0295349626852,35.7093985134194,7.96848509795903));
#51502=CARTESIAN_POINT('Origin',(-15.0295349571007,35.7980733216376,8.96454566463309));
#51503=CARTESIAN_POINT('',(-15.0083310209395,35.,8.00000000518325));
#51504=CARTESIAN_POINT('Origin',(-18.7164865659616,34.9995400237305,2.47743854316487));
#51505=CARTESIAN_POINT('',(-15.0284388455888,34.309193186478,-7.97011831617931));
#51506=CARTESIAN_POINT('Ctrl Pts',(-15.02843884595,34.3091931861949,-7.97011831960585));
#51507=CARTESIAN_POINT('Ctrl Pts',(-15.0288142473897,34.3027403453849,-7.96955903236514));
#51508=CARTESIAN_POINT('Ctrl Pts',(-15.0291947892652,34.2962892726555,-7.96899201083835));
#51509=CARTESIAN_POINT('Ctrl Pts',(-15.0315956288302,34.2561423126393,-7.96541417925132));
#51510=CARTESIAN_POINT('Ctrl Pts',(-15.0423642144861,34.088032797569,-7.94935354892829));
#51511=CARTESIAN_POINT('Ctrl Pts',(-15.0678832016234,33.7888553500623,-7.91115853602496));
#51512=CARTESIAN_POINT('Ctrl Pts',(-15.114218766681,33.3969471600944,-7.84108497328952));
#51513=CARTESIAN_POINT('Ctrl Pts',(-15.1721070596644,33.0117857858136,-7.7523407744212));
#51514=CARTESIAN_POINT('Ctrl Pts',(-15.2408086828326,32.6331700775731,-7.64523216589167));
#51515=CARTESIAN_POINT('Ctrl Pts',(-15.3195994745813,32.2609429659519,-7.51990519357029));
#51516=CARTESIAN_POINT('Ctrl Pts',(-15.3783785863874,32.0169741706016,-7.42420221713392));
#51517=CARTESIAN_POINT('Ctrl Pts',(-15.4169230076772,31.86578574641,-7.36055550663997));
#51518=CARTESIAN_POINT('Ctrl Pts',(-15.4247222721703,31.8356127003689,-7.34763441565639));
#51519=CARTESIAN_POINT('Ctrl Pts',(-15.4404979287257,31.7753956529338,-7.32140733008937));
#51520=CARTESIAN_POINT('Ctrl Pts',(-15.4484765070148,31.7453435409324,-7.30809767333041));
#51521=CARTESIAN_POINT('Ctrl Pts',(-15.4645974622036,31.6854045749681,-7.28110802809177));
#51522=CARTESIAN_POINT('Ctrl Pts',(-15.480871160413,31.6256699667238,-7.25376683616002));
#51523=CARTESIAN_POINT('Ctrl Pts',(-15.4974424841611,31.5663386705606,-7.2257208865272));
#51524=CARTESIAN_POINT('Ctrl Pts',(-15.5391665422511,31.4187349680549,-7.15483721768336));
#51525=CARTESIAN_POINT('Ctrl Pts',(-15.6079136147756,31.186835748441,-7.03634156130629));
#51526=CARTESIAN_POINT('Ctrl Pts',(-15.7160167807744,30.8511654700391,-6.84373604076318));
#51527=CARTESIAN_POINT('Ctrl Pts',(-15.8281946598233,30.5271896294902,-6.63649390534299));
#51528=CARTESIAN_POINT('Ctrl Pts',(-15.9435979596967,30.2145457052581,-6.41469672516666));
#51529=CARTESIAN_POINT('Ctrl Pts',(-16.0614211773277,29.9129824016044,-6.17828945308345));
#51530=CARTESIAN_POINT('Ctrl Pts',(-16.1410674095684,29.7192296560954,-6.01081869654751));
#51531=CARTESIAN_POINT('Ctrl Pts',(-16.201024234375,29.5766379294931,-5.88143375879927));
#51532=CARTESIAN_POINT('Ctrl Pts',(-16.2310582334771,29.5060231437582,-5.81579531894369));
#51533=CARTESIAN_POINT('Ctrl Pts',(-16.2611403443223,29.4364318013772,-5.7487171537012));
#51534=CARTESIAN_POINT('Ctrl Pts',(-16.2812018557675,29.3902654189335,-5.70367582739167));
#51535=CARTESIAN_POINT('Ctrl Pts',(-16.2912418263893,29.3672829433228,-5.68098052707624));
#51536=CARTESIAN_POINT('Ctrl Pts',(-16.3413467073928,29.2531738137251,-5.56692428562546));
#51537=CARTESIAN_POINT('Ctrl Pts',(-16.4209752464494,29.0755663284312,-5.3805739525971));
#51538=CARTESIAN_POINT('Ctrl Pts',(-16.5380927043861,28.8237073710608,-5.08947253852862));
#51539=CARTESIAN_POINT('Ctrl Pts',(-16.6521988334264,28.5861941970401,-4.78670273079409));
#51540=CARTESIAN_POINT('Ctrl Pts',(-16.7626209181631,28.3629560370339,-4.47207657050143));
#51541=CARTESIAN_POINT('Ctrl Pts',(-16.8686811319134,28.1540567825967,-4.14530483840524));
#51542=CARTESIAN_POINT('Ctrl Pts',(-16.9360190919976,28.0244823886621,-3.91909753316576));
#51543=CARTESIAN_POINT('Ctrl Pts',(-16.9769015617865,27.9465993498682,-3.77499834205324));
#51544=CARTESIAN_POINT('Ctrl Pts',(-16.9850178352183,27.9311779156137,-3.74604241809553));
#51545=CARTESIAN_POINT('Ctrl Pts',(-16.9970989762738,27.9082802658396,-3.70240206850094));
#51546=CARTESIAN_POINT('Ctrl Pts',(-17.0011098039485,27.9006880857066,-3.68782323736656));
#51547=CARTESIAN_POINT('Ctrl Pts',(-17.0090894186416,27.8856019217284,-3.65863499164274));
#51548=CARTESIAN_POINT('Ctrl Pts',(-17.028939778303,27.8481194758509,-3.58556503300444));
#51549=CARTESIAN_POINT('Ctrl Pts',(-17.0792575849446,27.7536962530504,-3.39428879967496));
#51550=CARTESIAN_POINT('Ctrl Pts',(-17.1517487909967,27.6195487618826,-3.0952359728616));
#51551=CARTESIAN_POINT('Ctrl Pts',(-17.2303931111566,27.4762917371816,-2.72865648498313));
#51552=CARTESIAN_POINT('Ctrl Pts',(-17.3002063624287,27.350831933827,-2.35424175561368));
#51553=CARTESIAN_POINT('Ctrl Pts',(-17.3606800021804,27.2433944968016,-1.97181718960462));
#51554=CARTESIAN_POINT('Ctrl Pts',(-17.3944075483594,27.1840391028347,-1.71137069546056));
#51555=CARTESIAN_POINT('Ctrl Pts',(-17.4133058696165,27.1508915270291,-1.54681069615592));
#51556=CARTESIAN_POINT('Ctrl Pts',(-17.4169764213736,27.1444596371577,-1.51380958994713));
#51557=CARTESIAN_POINT('Ctrl Pts',(-17.4223161454289,27.1351108602685,-1.46417290182852));
#51558=CARTESIAN_POINT('Ctrl Pts',(-17.4240680925248,27.1320449314045,-1.44760711706817));
#51559=CARTESIAN_POINT('Ctrl Pts',(-17.427510627014,27.1260229673048,-1.41448547255394));
#51560=CARTESIAN_POINT('Ctrl Pts',(-17.4359672821553,27.1112359574074,-1.33167245686228));
#51561=CARTESIAN_POINT('Ctrl Pts',(-17.4560080530611,27.0762709715337,-1.11624288587473));
#51562=CARTESIAN_POINT('Ctrl Pts',(-17.4796590959817,27.0351914609743,-0.784389106663583));
#51563=CARTESIAN_POINT('Ctrl Pts',(-17.4965481041675,27.0059632073484,-0.385493539873767));
#51564=CARTESIAN_POINT('Ctrl Pts',(-17.5019201088062,26.9966828319197,0.0140704127324454));
#51565=CARTESIAN_POINT('Ctrl Pts',(-17.4957277861607,27.007381080892,0.414304207998967));
#51566=CARTESIAN_POINT('Ctrl Pts',(-17.4838428507605,27.0279532267182,0.68157702428669));
#51567=CARTESIAN_POINT('Ctrl Pts',(-17.4719965255021,27.0485072370931,0.882202975679014));
#51568=CARTESIAN_POINT('Ctrl Pts',(-17.4675589144571,27.0562131445112,0.949106860867802));
#51569=CARTESIAN_POINT('Ctrl Pts',(-17.46016565691,27.0690684279055,1.04950595922574));
#51570=CARTESIAN_POINT('Ctrl Pts',(-17.457576204753,27.0735734930765,1.08300512007203));
#51571=CARTESIAN_POINT('Ctrl Pts',(-17.452169990578,27.0829854940715,1.14979178074418));
#51572=CARTESIAN_POINT('Ctrl Pts',(-17.4380789555938,27.1075334506051,1.31633108380749));
#51573=CARTESIAN_POINT('Ctrl Pts',(-17.4076148154949,27.1607728178961,1.61230440878633));
#51574=CARTESIAN_POINT('Ctrl Pts',(-17.3566928471347,27.2504459678313,1.99913654017659));
#51575=CARTESIAN_POINT('Ctrl Pts',(-17.2959966478747,27.3583556678014,2.37840729450143));
#51576=CARTESIAN_POINT('Ctrl Pts',(-17.2260177544666,27.4842097230089,2.75029691761448));
#51577=CARTESIAN_POINT('Ctrl Pts',(-17.1472204053951,27.6278648478571,3.11493317863537));
#51578=CARTESIAN_POINT('Ctrl Pts',(-17.0891066131584,27.7355027829494,3.35324065006489));
#51579=CARTESIAN_POINT('Ctrl Pts',(-17.0435370411747,27.8207186810042,3.53018489758881));
#51580=CARTESIAN_POINT('Ctrl Pts',(-17.0280164627851,27.8498722743193,3.58886846092364));
#51581=CARTESIAN_POINT('Ctrl Pts',(-17.0042530981179,27.8947333077787,3.67644679864269));
#51582=CARTESIAN_POINT('Ctrl Pts',(-16.9962509220472,27.9098766629836,3.70556736279662));
#51583=CARTESIAN_POINT('Ctrl Pts',(-16.9800906316592,27.9405369449744,3.76365014419879));
#51584=CARTESIAN_POINT('Ctrl Pts',(-16.939385630851,28.0179595915168,3.90815062897979));
#51585=CARTESIAN_POINT('Ctrl Pts',(-16.8634740930316,28.1641956124784,4.1619841373753));
#51586=CARTESIAN_POINT('Ctrl Pts',(-16.7573535075419,28.373470605273,4.48761501859039));
#51587=CARTESIAN_POINT('Ctrl Pts',(-16.6470263387764,28.5968114902901,4.80086397909257));
#51588=CARTESIAN_POINT('Ctrl Pts',(-16.5331726018234,28.8341259880668,5.1020516925123));
#51589=CARTESIAN_POINT('Ctrl Pts',(-16.4164677141308,29.085452957734,5.39139609998198));
#51590=CARTESIAN_POINT('Ctrl Pts',(-16.337218745459,29.2624588306839,5.57647684233942));
#51591=CARTESIAN_POINT('Ctrl Pts',(-16.2774164172135,29.3988358675752,5.71236190400463));
#51592=CARTESIAN_POINT('Ctrl Pts',(-16.2474239466557,29.4679305471591,5.77957270791569));
#51593=CARTESIAN_POINT('Ctrl Pts',(-16.2173288684335,29.5384043436101,5.84568321462317));
#51594=CARTESIAN_POINT('Ctrl Pts',(-16.1972465822248,29.5856958608511,5.88951186843353));
#51595=CARTESIAN_POINT('Ctrl Pts',(-16.1871956371008,29.6094971671554,5.91130422498456));
#51596=CARTESIAN_POINT('Ctrl Pts',(-16.1370259930167,29.7289888135984,6.01938988251468));
#51597=CARTESIAN_POINT('Ctrl Pts',(-16.057104001546,29.9237370570165,6.18715440328565));
#51598=CARTESIAN_POINT('Ctrl Pts',(-15.9390297178621,30.2265601706113,6.42365959173941));
#51599=CARTESIAN_POINT('Ctrl Pts',(-15.8235394373094,30.5402010295723,6.64525502413354));
#51600=CARTESIAN_POINT('Ctrl Pts',(-15.711436219916,30.8648784241873,6.85203405066681));
#51601=CARTESIAN_POINT('Ctrl Pts',(-15.6035641544746,31.2009178880349,7.04395106973463));
#51602=CARTESIAN_POINT('Ctrl Pts',(-15.5350683010191,31.4328114844198,7.16186232008555));
#51603=CARTESIAN_POINT('Ctrl Pts',(-15.4935287834857,31.5803222487406,7.23234907826555));
#51604=CARTESIAN_POINT('Ctrl Pts',(-15.4852844648543,31.6099533781527,7.24628590532913));
#51605=CARTESIAN_POINT('Ctrl Pts',(-15.4730173574796,31.6545961141017,7.2669485838441));
#51606=CARTESIAN_POINT('Ctrl Pts',(-15.4689437668496,31.6695138682647,7.27379758384884));
#51607=CARTESIAN_POINT('Ctrl Pts',(-15.4608410564491,31.6993756590486,7.28739653528903));
#51608=CARTESIAN_POINT('Ctrl Pts',(-15.4406901777392,31.7741145411665,7.32115558985279));
#51609=CARTESIAN_POINT('Ctrl Pts',(-15.389690259883,31.9695362055099,7.40582888847468));
#51610=CARTESIAN_POINT('Ctrl Pts',(-15.3165927362425,32.2742629280338,7.524737233672));
#51611=CARTESIAN_POINT('Ctrl Pts',(-15.2381817484458,32.6465557331785,7.64936422964285));
#51612=CARTESIAN_POINT('Ctrl Pts',(-15.1698145869288,33.0256109638998,7.7558817690875));
#51613=CARTESIAN_POINT('Ctrl Pts',(-15.1122465540415,33.4116170399966,7.84408549932686));
#51614=CARTESIAN_POINT('Ctrl Pts',(-15.0815844573055,33.6737462095084,7.8904344550347));
#51615=CARTESIAN_POINT('Ctrl Pts',(-15.0616818008391,33.8722127061586,7.92038964138432));
#51616=CARTESIAN_POINT('Ctrl Pts',(-15.0525040437334,33.9719135555013,7.9341649509122));
#51617=CARTESIAN_POINT('Ctrl Pts',(-15.0445252090246,34.0723315773334,7.946104162559));
#51618=CARTESIAN_POINT('Ctrl Pts',(-15.0407388713525,34.1226615238385,7.95176472328057));
#51619=CARTESIAN_POINT('Ctrl Pts',(-15.0395104426334,34.1394609432997,7.95360031025226));
#51620=CARTESIAN_POINT('Ctrl Pts',(-15.0371247553386,34.1730579141521,7.95716360868016));
#51621=CARTESIAN_POINT('Ctrl Pts',(-15.0267058342764,34.3242805352842,7.9727176126038));
#51622=CARTESIAN_POINT('Ctrl Pts',(-15.0126958765289,34.6050757151467,7.99353488525137));
#51623=CARTESIAN_POINT('Ctrl Pts',(-15.008331055905,34.8700262357082,8.00000016462761));
#51624=CARTESIAN_POINT('Ctrl Pts',(-15.0083310220457,35.,8.00000001022362));
#51625=CARTESIAN_POINT('Origin',(-15.0284388422963,34.2228423347594,-8.96638310375809));
#51626=CARTESIAN_POINT('Origin',(6.61363325216158E-15,51.,8.67361737988404E-16));
#51627=CARTESIAN_POINT('',(-5.94976035341753,52.,-16.457531763205));
#51628=CARTESIAN_POINT('Ctrl Pts',(-5.94976035341754,52.,-16.457531763205));
#51629=CARTESIAN_POINT('Ctrl Pts',(-5.92091018747472,52.,-16.3699833162058));
#51630=CARTESIAN_POINT('Ctrl Pts',(-5.88058573380552,51.9872720702992,-16.2882956005765));
#51631=CARTESIAN_POINT('Ctrl Pts',(-5.76788919698701,51.9323282975261,-16.1199790028325));
#51632=CARTESIAN_POINT('Ctrl Pts',(-5.6925630693955,51.8844425112493,-16.041953238066));
#51633=CARTESIAN_POINT('Ctrl Pts',(-5.5029792070492,51.7471294583736,-15.8953437672898));
#51634=CARTESIAN_POINT('Ctrl Pts',(-5.3784566649255,51.6448478052855,-15.8348531695271));
#51635=CARTESIAN_POINT('Ctrl Pts',(-5.07172747130897,51.3688831050111,-15.7570153376578));
#51636=CARTESIAN_POINT('Ctrl Pts',(-4.8896501126788,51.1882155912351,-15.7607283411234));
#51637=CARTESIAN_POINT('Ctrl Pts',(-4.71705612317004,51.0029762705271,-15.8113722756368));
#51638=CARTESIAN_POINT('Ctrl Pts',(-4.71567047028168,51.0014881341726,-15.8117821292766));
#51639=CARTESIAN_POINT('Ctrl Pts',(-4.71428571428572,51.,-15.8121949837485));
#51640=CARTESIAN_POINT('',(-11.,52.,-13.6106575888162));
#51641=CARTESIAN_POINT('Origin',(6.61363325216158E-15,52.,8.67361737988404E-16));
#51642=CARTESIAN_POINT('Origin',(-11.,51.,-13.6106575888162));
#51643=CARTESIAN_POINT('Origin',(-39.,35.,5.80048162279745E-15));
#51644=CARTESIAN_POINT('',(-39.,35.,8.00000000000001));
#51645=CARTESIAN_POINT('Origin',(-39.,35.,5.80048162279745E-15));
#51646=CARTESIAN_POINT('',(-39.,35.,8.00000000000001));
#51647=CARTESIAN_POINT('',(-15.0083310198037,35.0000000000015,-8.));
#51648=CARTESIAN_POINT('Ctrl Pts',(-15.0295349695495,35.7093985242134,7.96848522340063));
#51649=CARTESIAN_POINT('Ctrl Pts',(-15.0317433566877,35.7463665553888,7.9651940122473));
#51650=CARTESIAN_POINT('Ctrl Pts',(-15.0426551625308,35.9157991681627,7.94891905114317));
#51651=CARTESIAN_POINT('Ctrl Pts',(-15.0683544668512,36.2154241996097,7.91044832409081));
#51652=CARTESIAN_POINT('Ctrl Pts',(-15.114523084639,36.6052396991958,7.84062095850993));
#51653=CARTESIAN_POINT('Ctrl Pts',(-15.172467467588,36.9904539840521,7.75178521528497));
#51654=CARTESIAN_POINT('Ctrl Pts',(-15.2185721709881,37.244239624975,7.67989792119497));
#51655=CARTESIAN_POINT('Ctrl Pts',(-15.2558111371868,37.4334547433118,7.62119799676034));
#51656=CARTESIAN_POINT('Ctrl Pts',(-15.268667511965,37.4963390291725,7.60083353802511));
#51657=CARTESIAN_POINT('Ctrl Pts',(-15.2885991240044,37.5903849273567,7.56908189171299));
#51658=CARTESIAN_POINT('Ctrl Pts',(-15.2953521390605,37.6216927344669,7.55829506683936));
#51659=CARTESIAN_POINT('Ctrl Pts',(-15.3090652550016,37.6841895101737,7.53632694253893));
#51660=CARTESIAN_POINT('Ctrl Pts',(-15.3160188918469,37.7153492440176,7.52515600677147));
#51661=CARTESIAN_POINT('Ctrl Pts',(-15.3301157600136,37.7774928123971,7.50244147730046));
#51662=CARTESIAN_POINT('Ctrl Pts',(-15.3372528052153,37.8084492084351,7.49090783546308));
#51663=CARTESIAN_POINT('Ctrl Pts',(-15.3516906205381,37.8701004077745,7.46750369133237));
#51664=CARTESIAN_POINT('Ctrl Pts',(-15.3735964730095,37.9622016702459,7.43188662647507));
#51665=CARTESIAN_POINT('Ctrl Pts',(-15.426398756667,38.1745080970591,7.34522943759552));
#51666=CARTESIAN_POINT('Ctrl Pts',(-15.5063260286961,38.4705902033911,7.21146276609788));
#51667=CARTESIAN_POINT('Ctrl Pts',(-15.6084646962283,38.8148708775374,7.03535999982788));
#51668=CARTESIAN_POINT('Ctrl Pts',(-15.7159292600327,39.1485423724363,6.84388495360455));
#51669=CARTESIAN_POINT('Ctrl Pts',(-15.8278724895593,39.4719107714082,6.63710017888903));
#51670=CARTESIAN_POINT('Ctrl Pts',(-15.9434872372281,39.7851866573214,6.41492553412863));
#51671=CARTESIAN_POINT('Ctrl Pts',(-16.0224930219074,39.9873883122765,6.25640141129698));
#51672=CARTESIAN_POINT('Ctrl Pts',(-16.0673335103357,40.0992617711462,6.16423464647279));
#51673=CARTESIAN_POINT('Ctrl Pts',(-16.0723213408302,40.111666233097,6.15395223729438));
#51674=CARTESIAN_POINT('Ctrl Pts',(-16.0823076167348,40.136423295282,6.13330380375607));
#51675=CARTESIAN_POINT('Ctrl Pts',(-16.0873075880137,40.1487796487392,6.12293460055931));
#51676=CARTESIAN_POINT('Ctrl Pts',(-16.1023100598661,40.1857398541654,6.09172739208938));
#51677=CARTESIAN_POINT('Ctrl Pts',(-16.132319613612,40.2592118635954,6.02892668369661));
#51678=CARTESIAN_POINT('Ctrl Pts',(-16.2023323628313,40.427529809084,5.87969014002514));
#51679=CARTESIAN_POINT('Ctrl Pts',(-16.3020784722276,40.6592297618689,5.6588095006758));
#51680=CARTESIAN_POINT('Ctrl Pts',(-16.4205991740581,40.9235914790975,5.38144641910375));
#51681=CARTESIAN_POINT('Ctrl Pts',(-16.5372329513425,41.1744683699975,5.09166133998441));
#51682=CARTESIAN_POINT('Ctrl Pts',(-16.6512801927899,41.4119248014439,4.78923193375775));
#51683=CARTESIAN_POINT('Ctrl Pts',(-16.7251214017859,41.5612405737725,4.57896164840507));
#51684=CARTESIAN_POINT('Ctrl Pts',(-16.7795021298059,41.6698078920636,4.41790160529719));
#51685=CARTESIAN_POINT('Ctrl Pts',(-16.8064423804818,41.7232361946865,4.336531809764));
#51686=CARTESIAN_POINT('Ctrl Pts',(-16.8329729212215,41.7753671959408,4.25387627744134));
#51687=CARTESIAN_POINT('Ctrl Pts',(-16.8505649915887,41.8098310331041,4.19848369345172));
#51688=CARTESIAN_POINT('Ctrl Pts',(-16.8593017075143,41.8268946495008,4.17068006136599));
#51689=CARTESIAN_POINT('Ctrl Pts',(-16.9026451868541,41.9113027791667,4.03124011453002));
#51690=CARTESIAN_POINT('Ctrl Pts',(-16.9698918351146,42.0406829901195,3.80520340150321));
#51691=CARTESIAN_POINT('Ctrl Pts',(-17.0639163620806,42.2178935594719,3.45729388963807));
#51692=CARTESIAN_POINT('Ctrl Pts',(-17.1505544674681,42.3782570628572,3.10040997734272));
#51693=CARTESIAN_POINT('Ctrl Pts',(-17.2292496749196,42.5216412285864,2.73436563138696));
#51694=CARTESIAN_POINT('Ctrl Pts',(-17.2760301884329,42.6057249429385,2.48405897740466));
#51695=CARTESIAN_POINT('Ctrl Pts',(-17.308829068095,42.6643630785034,2.29389163401185));
#51696=CARTESIAN_POINT('Ctrl Pts',(-17.3246567295576,42.6925754012235,2.19819833775785));
#51697=CARTESIAN_POINT('Ctrl Pts',(-17.3395957513147,42.7191006585463,2.10157180807124));
#51698=CARTESIAN_POINT('Ctrl Pts',(-17.3469144880934,42.732079591568,2.05310130046466));
#51699=CARTESIAN_POINT('Ctrl Pts',(-17.349329687354,42.7363599449743,2.0369130602982));
#51700=CARTESIAN_POINT('Ctrl Pts',(-17.3541024826582,42.7448134688302,2.00453109096472));
#51701=CARTESIAN_POINT('Ctrl Pts',(-17.3753269002319,42.7823820652959,1.85874834776437));
#51702=CARTESIAN_POINT('Ctrl Pts',(-17.4111077681713,42.8453498665281,1.58229806305072));
#51703=CARTESIAN_POINT('Ctrl Pts',(-17.4506671612683,42.9144491571661,1.18931724193939));
#51704=CARTESIAN_POINT('Ctrl Pts',(-17.4791159589772,42.9638671728884,0.793641063198546));
#51705=CARTESIAN_POINT('Ctrl Pts',(-17.4962775848125,42.9935694415057,0.395255512641708));
#51706=CARTESIAN_POINT('Ctrl Pts',(-17.5019512435747,43.0033708970284,-0.00587045182199218));
#51707=CARTESIAN_POINT('Ctrl Pts',(-17.4979229030629,42.996411578592,-0.275147149881629));
#51708=CARTESIAN_POINT('Ctrl Pts',(-17.4929099765896,42.9877388633763,-0.444040376574195));
#51709=CARTESIAN_POINT('Ctrl Pts',(-17.4917847507504,42.9857917334257,-0.477774124639363));
#51710=CARTESIAN_POINT('Ctrl Pts',(-17.4892933114556,42.9814790647192,-0.54509646113387));
#51711=CARTESIAN_POINT('Ctrl Pts',(-17.4851939707346,42.9743815215779,-0.645889850217576));
#51712=CARTESIAN_POINT('Ctrl Pts',(-17.4731187517648,42.9534521747222,-0.879754014765898));
#51713=CARTESIAN_POINT('Ctrl Pts',(-17.4488480317093,42.9112815338686,-1.21014039122987));
#51714=CARTESIAN_POINT('Ctrl Pts',(-17.4089265646358,42.8415254430959,-1.60084195832246));
#51715=CARTESIAN_POINT('Ctrl Pts',(-17.3586077045064,42.7529391960171,-1.98590605797735));
#51716=CARTESIAN_POINT('Ctrl Pts',(-17.298261825805,42.6456925923558,-2.36541901410585));
#51717=CARTESIAN_POINT('Ctrl Pts',(-17.2515785247746,42.5617707505403,-2.6147603356838));
#51718=CARTESIAN_POINT('Ctrl Pts',(-17.2142296691155,42.4941394755673,-2.80039473020187));
#51719=CARTESIAN_POINT('Ctrl Pts',(-17.1949710995766,42.459150835844,-2.89286890143597));
#51720=CARTESIAN_POINT('Ctrl Pts',(-17.1714983596828,42.4162647832962,-3.00015440654776));
#51721=CARTESIAN_POINT('Ctrl Pts',(-17.1612252823544,42.3974405676299,-3.04600495601648));
#51722=CARTESIAN_POINT('Ctrl Pts',(-17.1543293677358,42.3847921027298,-3.07654331078785));
#51723=CARTESIAN_POINT('Ctrl Pts',(-17.1508564955136,42.3784159555916,-3.09180387440957));
#51724=CARTESIAN_POINT('Ctrl Pts',(-17.1194193072583,42.3206396331724,-3.22888779505685));
#51725=CARTESIAN_POINT('Ctrl Pts',(-17.0610778277326,42.2125971495852,-3.46837047222968));
#51726=CARTESIAN_POINT('Ctrl Pts',(-16.9669450105092,42.0350669660386,-3.81550142136755));
#51727=CARTESIAN_POINT('Ctrl Pts',(-16.8668826707291,41.8424294075684,-4.15099303803763));
#51728=CARTESIAN_POINT('Ctrl Pts',(-16.7615498700067,41.6348972977722,-4.47519454537473));
#51729=CARTESIAN_POINT('Ctrl Pts',(-16.6515873621956,41.4125459881677,-4.78836072736283));
#51730=CARTESIAN_POINT('Ctrl Pts',(-16.5376307394374,41.1753160084247,-5.0906578673893));
#51731=CARTESIAN_POINT('Ctrl Pts',(-16.459424578268,41.0071134947669,-5.28499714012445));
#51732=CARTESIAN_POINT('Ctrl Pts',(-16.4149293360004,40.9096091132394,-5.3922889034193));
#51733=CARTESIAN_POINT('Ctrl Pts',(-16.4099784223582,40.8987351149821,-5.40418207913157));
#51734=CARTESIAN_POINT('Ctrl Pts',(-16.4000630421998,40.8769064826911,-5.42791213035301));
#51735=CARTESIAN_POINT('Ctrl Pts',(-16.3950971987479,40.8659487935054,-5.43975226059081));
#51736=CARTESIAN_POINT('Ctrl Pts',(-16.3801965514582,40.8329910004454,-5.47514895551087));
#51737=CARTESIAN_POINT('Ctrl Pts',(-16.3503724304234,40.7667142379802,-5.54547291492612));
#51738=CARTESIAN_POINT('Ctrl Pts',(-16.2806640395699,40.6095423595599,-5.70629895921682));
#51739=CARTESIAN_POINT('Ctrl Pts',(-16.180974215943,40.3778254119992,-5.92688153012738));
#51740=CARTESIAN_POINT('Ctrl Pts',(-16.0619208336956,40.0882521359279,-6.17725540907027));
#51741=CARTESIAN_POINT('Ctrl Pts',(-15.9441997798774,39.7870400491607,-6.41351604010334));
#51742=CARTESIAN_POINT('Ctrl Pts',(-15.8285960066714,39.4739510666078,-6.63574626677591));
#51743=CARTESIAN_POINT('Ctrl Pts',(-15.7534876620311,39.257070777687,-6.77451562138855));
#51744=CARTESIAN_POINT('Ctrl Pts',(-15.6981121142448,39.0912312910581,-6.87502762908889));
#51745=CARTESIAN_POINT('Ctrl Pts',(-15.6752382613982,39.0214687498039,-6.91616449658992));
#51746=CARTESIAN_POINT('Ctrl Pts',(-15.6526439888158,38.9508583499558,-6.95636275137005));
#51747=CARTESIAN_POINT('Ctrl Pts',(-15.6436292758259,38.9225459338593,-6.97236673066097));
#51748=CARTESIAN_POINT('Ctrl Pts',(-15.6391322617862,38.9083519028867,-6.98033309486872));
#51749=CARTESIAN_POINT('Ctrl Pts',(-15.6256917526769,38.8657149425293,-7.00409230751034));
#51750=CARTESIAN_POINT('Ctrl Pts',(-15.5812090766541,38.723169271701,-7.08238741852476));
#51751=CARTESIAN_POINT('Ctrl Pts',(-15.5041012479151,38.462781160908,-7.21524325503216));
#51752=CARTESIAN_POINT('Ctrl Pts',(-15.4083955592681,38.1073501930475,-7.37530469795503));
#51753=CARTESIAN_POINT('Ctrl Pts',(-15.3206097549118,37.7434785335194,-7.51827869502257));
#51754=CARTESIAN_POINT('Ctrl Pts',(-15.2415938895141,37.3709035407501,-7.64400026688226));
#51755=CARTESIAN_POINT('Ctrl Pts',(-15.1953577523619,37.1164948243452,-7.71609520162805));
#51756=CARTESIAN_POINT('Ctrl Pts',(-15.163332038576,36.9233246794636,-7.76564492189045));
#51757=CARTESIAN_POINT('Ctrl Pts',(-15.1530988410459,36.8585404781279,-7.78140743483318));
#51758=CARTESIAN_POINT('Ctrl Pts',(-15.1408856330674,36.7770549489708,-7.8001509829503));
#51759=CARTESIAN_POINT('Ctrl Pts',(-15.1384724307588,36.7607358821017,-7.80385089936044));
#51760=CARTESIAN_POINT('Ctrl Pts',(-15.1337109333127,36.7280919295432,-7.81114447537864));
#51761=CARTESIAN_POINT('Ctrl Pts',(-15.1266636736583,36.6791013644423,-7.82192932151362));
#51762=CARTESIAN_POINT('Ctrl Pts',(-15.101872893652,36.4991978119273,-7.85976165441412));
#51763=CARTESIAN_POINT('Ctrl Pts',(-15.067082344028,36.2033290107109,-7.91236253990328));
#51764=CARTESIAN_POINT('Ctrl Pts',(-15.0334448413432,35.8056518925192,-7.96269982722361));
#51765=CARTESIAN_POINT('Ctrl Pts',(-15.0197896913276,35.5383826286899,-7.98299411499247));
#51766=CARTESIAN_POINT('Ctrl Pts',(-15.0129323471145,35.3371095966479,-7.99317645517523));
#51767=CARTESIAN_POINT('Ctrl Pts',(-15.0103495943628,35.2362677516597,-7.99700746106585));
#51768=CARTESIAN_POINT('Ctrl Pts',(-15.0088365703435,35.1182557469141,-7.99925059538832));
#51769=CARTESIAN_POINT('Ctrl Pts',(-15.0084304452709,35.0549371823108,-7.99985262131205));
#51770=CARTESIAN_POINT('Ctrl Pts',(-15.0083513612805,35.0253618023294,-7.9999698476096));
#51771=CARTESIAN_POINT('Ctrl Pts',(-15.0083332807496,35.0084550273716,-7.99999664859286));
#51772=CARTESIAN_POINT('Ctrl Pts',(-15.0083310198037,35.0042389907688,-8.));
#51773=CARTESIAN_POINT('Ctrl Pts',(-15.0083310198037,35.,-8.));
#51774=CARTESIAN_POINT('Origin',(-18.7165753455904,35.0004252159185,-2.47873660745326));
#51775=CARTESIAN_POINT('Origin',(33.,35.,5.81688018065629E-15));
#51776=CARTESIAN_POINT('',(17.3292735477736,26.271682819109,2.19464782253529));
#51777=CARTESIAN_POINT('',(14.3614066597098,35.,-9.00000016129458));
#51778=CARTESIAN_POINT('Ctrl Pts',(17.3292737690855,26.2716828205678,2.19464785677071));
#51779=CARTESIAN_POINT('Ctrl Pts',(17.3511060669366,26.2365725392203,2.0550110257917));
#51780=CARTESIAN_POINT('Ctrl Pts',(17.3906663845752,26.1732400003362,1.7748105293247));
#51781=CARTESIAN_POINT('Ctrl Pts',(17.437569987258,26.0986411319388,1.35174774880715));
#51782=CARTESIAN_POINT('Ctrl Pts',(17.4718892370587,26.0443244871895,0.925925340728199));
#51783=CARTESIAN_POINT('Ctrl Pts',(17.4934501269048,26.0103138422386,0.497330371512314));
#51784=CARTESIAN_POINT('Ctrl Pts',(17.5020487821195,25.9967743670159,0.0659341336017064));
#51785=CARTESIAN_POINT('Ctrl Pts',(17.4989814353938,26.0016030072543,-0.223560920629813));
#51786=CARTESIAN_POINT('Ctrl Pts',(17.4947294175519,26.0083037272082,-0.386947362930728));
#51787=CARTESIAN_POINT('Ctrl Pts',(17.4942218702242,26.0091036288164,-0.405108992107224));
#51788=CARTESIAN_POINT('Ctrl Pts',(17.493136378926,26.0108145533485,-0.441447458433586));
#51789=CARTESIAN_POINT('Ctrl Pts',(17.4914016205574,26.0135490847956,-0.496002228547374));
#51790=CARTESIAN_POINT('Ctrl Pts',(17.4866302308682,26.0210726538394,-0.622967538857688));
#51791=CARTESIAN_POINT('Ctrl Pts',(17.4742213411114,26.0406537166651,-0.875588561273599));
#51792=CARTESIAN_POINT('Ctrl Pts',(17.4484604427764,26.0813805487345,-1.23279551020348));
#51793=CARTESIAN_POINT('Ctrl Pts',(17.4051428383694,26.1501709226248,-1.65571464127194));
#51794=CARTESIAN_POINT('Ctrl Pts',(17.3498265631662,26.2385485648806,-2.07302547248468));
#51795=CARTESIAN_POINT('Ctrl Pts',(17.2828820574345,26.346327540878,-2.48481427818531));
#51796=CARTESIAN_POINT('Ctrl Pts',(17.2307282660594,26.4310836356844,-2.75569454847502));
#51797=CARTESIAN_POINT('Ctrl Pts',(17.1888715420821,26.49951298051,-2.9574931035026));
#51798=CARTESIAN_POINT('Ctrl Pts',(17.1744623540533,26.5231335077224,-3.0245322647391));
#51799=CARTESIAN_POINT('Ctrl Pts',(17.1521727950165,26.5597867238486,-3.12475040445865));
#51800=CARTESIAN_POINT('Ctrl Pts',(17.1446270920639,26.5722135398249,-3.15811347120182));
#51801=CARTESIAN_POINT('Ctrl Pts',(17.1293335457261,26.5974404738732,-3.22463311481988));
#51802=CARTESIAN_POINT('Ctrl Pts',(17.1060876109449,26.6358447593403,-3.32411522776261));
#51803=CARTESIAN_POINT('Ctrl Pts',(17.0819389615532,26.6759341796544,-3.42271126226114));
#51804=CARTESIAN_POINT('Ctrl Pts',(17.0489628351658,26.7308759359264,-3.55339434614476));
#51805=CARTESIAN_POINT('Ctrl Pts',(17.0321251263301,26.7590259608061,-3.6181906858736));
#51806=CARTESIAN_POINT('Ctrl Pts',(16.9806303848643,26.8454473156521,-3.81091830589896));
#51807=CARTESIAN_POINT('Ctrl Pts',(16.9093393110058,26.9659542661823,-4.06352061760149));
#51808=CARTESIAN_POINT('Ctrl Pts',(16.7952622185118,27.1620749385031,-4.42989921625676));
#51809=CARTESIAN_POINT('Ctrl Pts',(16.6747509585551,27.3732294139522,-4.78421811769584));
#51810=CARTESIAN_POINT('Ctrl Pts',(16.5484803841572,27.5992268215029,-5.12684327183664));
#51811=CARTESIAN_POINT('Ctrl Pts',(16.4171069086335,27.8400050159176,-5.45805051992441));
#51812=CARTESIAN_POINT('Ctrl Pts',(16.281282026911,28.0956280558873,-5.77803208192815));
#51813=CARTESIAN_POINT('Ctrl Pts',(16.1882039368748,28.2760687412164,-5.98394349483031));
#51814=CARTESIAN_POINT('Ctrl Pts',(16.1352639128197,28.3804481175221,-6.09769030982974));
#51815=CARTESIAN_POINT('Ctrl Pts',(16.1293735897666,28.3920858784171,-6.11029996086992));
#51816=CARTESIAN_POINT('Ctrl Pts',(16.1175772019141,28.4154417739722,-6.13546148370861));
#51817=CARTESIAN_POINT('Ctrl Pts',(16.1116694515318,28.4271632637811,-6.14801691836739));
#51818=CARTESIAN_POINT('Ctrl Pts',(16.0939372564988,28.4624208921774,-6.18556695599072));
#51819=CARTESIAN_POINT('Ctrl Pts',(16.0584429638702,28.533296920399,-6.26018989631675));
#51820=CARTESIAN_POINT('Ctrl Pts',(15.9754558171471,28.701195284815,-6.4309991232647));
#51821=CARTESIAN_POINT('Ctrl Pts',(15.8566650947646,28.9482353299555,-6.66570732687656));
#51822=CARTESIAN_POINT('Ctrl Pts',(15.7145096352823,29.2562207641436,-6.93284443275944));
#51823=CARTESIAN_POINT('Ctrl Pts',(15.5735379528705,29.5758923245201,-7.18571569707291));
#51824=CARTESIAN_POINT('Ctrl Pts',(15.4345728291732,29.9075078732476,-7.42444661746228));
#51825=CARTESIAN_POINT('Ctrl Pts',(15.3438463154491,30.1367964068834,-7.57417606209572));
#51826=CARTESIAN_POINT('Ctrl Pts',(15.2767533263472,30.3119673663242,-7.68290785298914));
#51827=CARTESIAN_POINT('Ctrl Pts',(15.2434450761117,30.4003545024313,-7.73638191511748));
#51828=CARTESIAN_POINT('Ctrl Pts',(15.2105406590842,30.4899725877742,-7.7885075658178));
#51829=CARTESIAN_POINT('Ctrl Pts',(15.1886995006888,30.5499950542398,-7.82295681597048));
#51830=CARTESIAN_POINT('Ctrl Pts',(15.1778240237092,30.5801516665408,-7.84003469134717));
#51831=CARTESIAN_POINT('Ctrl Pts',(15.1237240865472,30.731563564408,-7.92462632761097));
#51832=CARTESIAN_POINT('Ctrl Pts',(15.0393580935828,30.9766684727028,-8.05421723123254));
#51833=CARTESIAN_POINT('Ctrl Pts',(14.9202834898964,31.3530424540673,-8.23149492286624));
#51834=CARTESIAN_POINT('Ctrl Pts',(14.8096155182678,31.73838151464,-8.39167232422591));
#51835=CARTESIAN_POINT('Ctrl Pts',(14.7083363206634,32.1330068510787,-8.53460644040646));
#51836=CARTESIAN_POINT('Ctrl Pts',(14.6477694189893,32.4025470501747,-8.6181996854931));
#51837=CARTESIAN_POINT('Ctrl Pts',(14.6052284867057,32.6072444536737,-8.67639054024899));
#51838=CARTESIAN_POINT('Ctrl Pts',(14.5846793849461,32.7102290861197,-8.70435921933926));
#51839=CARTESIAN_POINT('Ctrl Pts',(14.5652670414341,32.8141936760557,-8.73060894583011));
#51840=CARTESIAN_POINT('Ctrl Pts',(14.5525843754099,32.8837243142594,-8.74772307933595));
#51841=CARTESIAN_POINT('Ctrl Pts',(14.5463699486225,32.9186159013033,-8.75609070595351));
#51842=CARTESIAN_POINT('Ctrl Pts',(14.5160511941617,33.0931020531445,-8.79683395861055));
#51843=CARTESIAN_POINT('Ctrl Pts',(14.4722201586652,33.373221817893,-8.85521402989592));
#51844=CARTESIAN_POINT('Ctrl Pts',(14.4210060853739,33.7962428049278,-8.92256078015134));
#51845=CARTESIAN_POINT('Ctrl Pts',(14.384787810699,34.2221320089307,-8.96973958641945));
#51846=CARTESIAN_POINT('Ctrl Pts',(14.3653246092572,34.6234681282666,-8.99493795043249));
#51847=CARTESIAN_POINT('Ctrl Pts',(14.3614067526773,34.8834816469066,-9.00000050730076));
#51848=CARTESIAN_POINT('Ctrl Pts',(14.3614066597098,35.,-9.00000016129458));
#51849=CARTESIAN_POINT('',(14.3614066770412,34.9999999999574,9.00000209879965));
#51850=CARTESIAN_POINT('Ctrl Pts',(14.3614066597098,35.,-9.00000016129458));
#51851=CARTESIAN_POINT('Ctrl Pts',(14.3614066376026,35.0277074310129,-9.00000007901619));
#51852=CARTESIAN_POINT('Ctrl Pts',(14.3615056095479,35.0554333238382,-8.99987205272605));
#51853=CARTESIAN_POINT('Ctrl Pts',(14.3622202944309,35.1553869208446,-8.99894824492613));
#51854=CARTESIAN_POINT('Ctrl Pts',(14.364004617662,35.2638890175708,-8.99664193507595));
#51855=CARTESIAN_POINT('Ctrl Pts',(14.3678708568023,35.3908080930607,-8.99163943659494));
#51856=CARTESIAN_POINT('Ctrl Pts',(14.3699119521736,35.4452738325292,-8.98899671792919));
#51857=CARTESIAN_POINT('Ctrl Pts',(14.3713582357703,35.4816003408514,-8.98712367181897));
#51858=CARTESIAN_POINT('Ctrl Pts',(14.3721244547376,35.4997776671369,-8.98613114393334));
#51859=CARTESIAN_POINT('Ctrl Pts',(14.3793930408947,35.6631611333616,-8.97671315535948));
#51860=CARTESIAN_POINT('Ctrl Pts',(14.3976438853735,35.9514328119009,-8.95303591956361));
#51861=CARTESIAN_POINT('Ctrl Pts',(14.4402174756958,36.3775287174802,-8.89738550077062));
#51862=CARTESIAN_POINT('Ctrl Pts',(14.4972001649901,36.7975284738977,-8.82208837920263));
#51863=CARTESIAN_POINT('Ctrl Pts',(14.5678058281868,37.2116143810925,-8.72746905651757));
#51864=CARTESIAN_POINT('Ctrl Pts',(14.6512515007626,37.6199371740426,-8.61369740670257));
#51865=CARTESIAN_POINT('Ctrl Pts',(14.714922695497,37.8883901560955,-8.52509406629469));
#51866=CARTESIAN_POINT('Ctrl Pts',(14.7823561461911,38.1549915000705,-8.43006851499351));
#51867=CARTESIAN_POINT('Ctrl Pts',(14.8529334900639,38.4173124396441,-8.32948876487167));
#51868=CARTESIAN_POINT('Ctrl Pts',(14.9670194458454,38.7987124669293,-8.16253453804374));
#51869=CARTESIAN_POINT('Ctrl Pts',(15.0882207409183,39.168649536036,-7.97989226158918));
#51870=CARTESIAN_POINT('Ctrl Pts',(15.2155193643328,39.5276214399999,-7.78180070283411));
#51871=CARTESIAN_POINT('Ctrl Pts',(15.347968056224,39.8760186490394,-7.56835432810572));
#51872=CARTESIAN_POINT('Ctrl Pts',(15.4846761045389,40.2141337582382,-7.33951102833573));
#51873=CARTESIAN_POINT('Ctrl Pts',(15.5780895672648,40.432822845256,-7.17656656886614));
#51874=CARTESIAN_POINT('Ctrl Pts',(15.6487987361288,40.5943470971465,-7.05038640806119));
#51875=CARTESIAN_POINT('Ctrl Pts',(15.6724766893401,40.6477728571003,-7.00766401323145));
#51876=CARTESIAN_POINT('Ctrl Pts',(15.708130928521,40.7272893866598,-6.94257369952877));
#51877=CARTESIAN_POINT('Ctrl Pts',(15.7200453127601,40.7537060004307,-6.92069658004402));
#51878=CARTESIAN_POINT('Ctrl Pts',(15.7438699413295,40.8062312885166,-6.87668903736941));
#51879=CARTESIAN_POINT('Ctrl Pts',(15.8034316480523,40.9367982438501,-6.76601855320207));
#51880=CARTESIAN_POINT('Ctrl Pts',(15.9105449908361,41.165170585149,-6.56096252460349));
#51881=CARTESIAN_POINT('Ctrl Pts',(16.0523683483239,41.4558963118018,-6.27508605292446));
#51882=CARTESIAN_POINT('Ctrl Pts',(16.1924509552874,41.7331271079221,-5.97664957951226));
#51883=CARTESIAN_POINT('Ctrl Pts',(16.3300700330948,41.9970137913492,-5.66546287973468));
#51884=CARTESIAN_POINT('Ctrl Pts',(16.4645126454744,42.2475866322906,-5.34123484264189));
#51885=CARTESIAN_POINT('Ctrl Pts',(16.551545459628,42.4056990482232,-5.11612309781091));
#51886=CARTESIAN_POINT('Ctrl Pts',(16.6156629556038,42.5208783365345,-4.94380041397795));
#51887=CARTESIAN_POINT('Ctrl Pts',(16.6421374084707,42.5681598955139,-4.87127202341161));
#51888=CARTESIAN_POINT('Ctrl Pts',(16.6682856596061,42.6145438657752,-4.79781450748127));
#51889=CARTESIAN_POINT('Ctrl Pts',(16.6787183539013,42.6330253866751,-4.76835671677202));
#51890=CARTESIAN_POINT('Ctrl Pts',(16.6839221782026,42.6422314870762,-4.75358816492742));
#51891=CARTESIAN_POINT('Ctrl Pts',(16.6994733659498,42.6697067160829,-4.70922595173132));
#51892=CARTESIAN_POINT('Ctrl Pts',(16.7509399347112,42.7603918942034,-4.56088716452504));
#51893=CARTESIAN_POINT('Ctrl Pts',(16.8401806635805,42.9155723226508,-4.28969471768694));
#51894=CARTESIAN_POINT('Ctrl Pts',(16.9513843119186,43.1054544466778,-3.91911439587559));
#51895=CARTESIAN_POINT('Ctrl Pts',(17.0542658268551,43.2783291427594,-3.53941810887066));
#51896=CARTESIAN_POINT('Ctrl Pts',(17.1482703302904,43.4340806289113,-3.15042074269136));
#51897=CARTESIAN_POINT('Ctrl Pts',(17.2328153607806,43.5724565750841,-2.75187368374423));
#51898=CARTESIAN_POINT('Ctrl Pts',(17.2824584153442,43.6528595920182,-2.4795973691923));
#51899=CARTESIAN_POINT('Ctrl Pts',(17.3170018972331,43.7085800734727,-2.27282393995594));
#51900=CARTESIAN_POINT('Ctrl Pts',(17.3308346565766,43.7308418656642,-2.18613345094775));
#51901=CARTESIAN_POINT('Ctrl Pts',(17.3439433873367,43.7518874172268,-2.09875922302458));
#51902=CARTESIAN_POINT('Ctrl Pts',(17.3491284574022,43.7602078189126,-2.06375449351543));
#51903=CARTESIAN_POINT('Ctrl Pts',(17.3516928181856,43.7643207749255,-2.04621739953348));
#51904=CARTESIAN_POINT('Ctrl Pts',(17.3592888703892,43.7764982940174,-1.99358342260552));
#51905=CARTESIAN_POINT('Ctrl Pts',(17.3839574521878,43.8160064938899,-1.81802250396776));
#51906=CARTESIAN_POINT('Ctrl Pts',(17.4224896102278,43.8774204221013,-1.50098745610886));
#51907=CARTESIAN_POINT('Ctrl Pts',(17.4612538851346,43.9388668744836,-1.07610201267747));
#51908=CARTESIAN_POINT('Ctrl Pts',(17.4872946690239,43.9799852113784,-0.649047627026372));
#51909=CARTESIAN_POINT('Ctrl Pts',(17.5004730817091,44.0007455676255,-0.219815327381889));
#51910=CARTESIAN_POINT('Ctrl Pts',(17.5006202695435,44.0009772133248,0.211616086610037));
#51911=CARTESIAN_POINT('Ctrl Pts',(17.4918963684518,43.9872347552916,0.500725743964407));
#51912=CARTESIAN_POINT('Ctrl Pts',(17.4844632294961,43.9755071850327,0.663777591100614));
#51913=CARTESIAN_POINT('Ctrl Pts',(17.4836018344785,43.974147935278,0.68190836175621));
#51914=CARTESIAN_POINT('Ctrl Pts',(17.4818107925467,43.9713212685151,0.718139871596486));
#51915=CARTESIAN_POINT('Ctrl Pts',(17.4790225731436,43.9669201546786,0.772429726229226));
#51916=CARTESIAN_POINT('Ctrl Pts',(17.4718092998787,43.955528553035,0.898706242354752));
#51917=CARTESIAN_POINT('Ctrl Pts',(17.4545856479766,43.9282975565738,1.14967584344988));
#51918=CARTESIAN_POINT('Ctrl Pts',(17.4221701314698,43.8769122363278,1.5037659231055));
#51919=CARTESIAN_POINT('Ctrl Pts',(17.3713030937696,43.7958350818669,1.9218003241365));
#51920=CARTESIAN_POINT('Ctrl Pts',(17.3089465433007,43.6957424080558,2.33313911665655));
#51921=CARTESIAN_POINT('Ctrl Pts',(17.2355404985145,43.5768880716263,2.73791691800328));
#51922=CARTESIAN_POINT('Ctrl Pts',(17.1514946160016,43.4393880418327,3.13622814947783));
#51923=CARTESIAN_POINT('Ctrl Pts',(17.0886288004399,43.3352780146074,3.3974953294847));
#51924=CARTESIAN_POINT('Ctrl Pts',(17.0390093050541,43.2524898553595,3.59184767367111));
#51925=CARTESIAN_POINT('Ctrl Pts',(17.0220577526584,43.2241091652068,3.65636534982383));
#51926=CARTESIAN_POINT('Ctrl Pts',(16.9873464535774,43.1657674455286,3.78486738977431));
#51927=CARTESIAN_POINT('Ctrl Pts',(16.969665761866,43.1359391994175,3.84855910124427));
#51928=CARTESIAN_POINT('Ctrl Pts',(16.9157105946208,43.044537870347,4.0379531574931));
#51929=CARTESIAN_POINT('Ctrl Pts',(16.8413257578772,42.9175434522878,4.28603888103889));
#51930=CARTESIAN_POINT('Ctrl Pts',(16.7231644518036,42.7121100049819,4.64542937874511));
#51931=CARTESIAN_POINT('Ctrl Pts',(16.5991255965279,42.492026743552,4.99254748112345));
#51932=CARTESIAN_POINT('Ctrl Pts',(16.4698875992596,42.2574533175684,5.32775738380935));
#51933=CARTESIAN_POINT('Ctrl Pts',(16.3361146386698,42.008423365498,5.65133134784423));
#51934=CARTESIAN_POINT('Ctrl Pts',(16.198469624878,41.7448458160864,5.96345545550853));
#51935=CARTESIAN_POINT('Ctrl Pts',(16.1045744613366,41.5592829957575,6.16397321657772));
#51936=CARTESIAN_POINT('Ctrl Pts',(16.0512901439369,41.4520682654557,6.27464008616567));
#51937=CARTESIAN_POINT('Ctrl Pts',(16.0453631674068,41.4401161028038,6.28690688131533));
#51938=CARTESIAN_POINT('Ctrl Pts',(16.0334966898785,41.4161326615954,6.31138140352268));
#51939=CARTESIAN_POINT('Ctrl Pts',(16.0275562424261,41.4040994470756,6.32359104718472));
#51940=CARTESIAN_POINT('Ctrl Pts',(16.0097365606481,41.3679208424132,6.36009103590755));
#51941=CARTESIAN_POINT('Ctrl Pts',(15.9740858574141,41.2952115292935,6.43261248131344));
#51942=CARTESIAN_POINT('Ctrl Pts',(15.890863814573,41.1230941910587,6.59850667395035));
#51943=CARTESIAN_POINT('Ctrl Pts',(15.7721103718677,40.8701837370035,6.82615055965585));
#51944=CARTESIAN_POINT('Ctrl Pts',(15.6306036959951,40.5553723531171,7.08471028746543));
#51945=CARTESIAN_POINT('Ctrl Pts',(15.4908983764982,40.2290636660933,7.32887233497747));
#51946=CARTESIAN_POINT('Ctrl Pts',(15.3538348876611,39.8909717055415,7.55872848618295));
#51947=CARTESIAN_POINT('Ctrl Pts',(15.2648147848089,39.6574545255017,7.70240667061981));
#51948=CARTESIAN_POINT('Ctrl Pts',(15.1991730514431,39.479138636835,7.80653923747221));
#51949=CARTESIAN_POINT('Ctrl Pts',(15.1666333112585,39.3891856742346,7.85769847361585));
#51950=CARTESIAN_POINT('Ctrl Pts',(15.134563221709,39.2980104232192,7.90748435211918));
#51951=CARTESIAN_POINT('Ctrl Pts',(15.1132930875125,39.2369516244807,7.94036795803072));
#51952=CARTESIAN_POINT('Ctrl Pts',(15.102709165511,39.2062731431645,7.95666206124221));
#51953=CARTESIAN_POINT('Ctrl Pts',(15.0501936888608,39.0525234864699,8.03718433153651));
#51954=CARTESIAN_POINT('Ctrl Pts',(14.9685896006955,38.8037728772036,8.16021179815972));
#51955=CARTESIAN_POINT('Ctrl Pts',(14.8543402338744,38.4222100538624,8.32745277700717));
#51956=CARTESIAN_POINT('Ctrl Pts',(14.7491820596274,38.0319615605815,8.47736748319502));
#51957=CARTESIAN_POINT('Ctrl Pts',(14.6540967740514,37.6327106633516,8.6097776148454));
#51958=CARTESIAN_POINT('Ctrl Pts',(14.5981130579524,37.3602821844718,8.68615604995556));
#51959=CARTESIAN_POINT('Ctrl Pts',(14.5591779822573,37.1534953483407,8.73885104080071));
#51960=CARTESIAN_POINT('Ctrl Pts',(14.5435912348191,37.0668202536551,8.75985069153186));
#51961=CARTESIAN_POINT('Ctrl Pts',(14.5288373475413,36.9794852908176,8.77963320861684));
#51962=CARTESIAN_POINT('Ctrl Pts',(14.5230032029764,36.9444981306421,8.78744833921318));
#51963=CARTESIAN_POINT('Ctrl Pts',(14.5201189478982,36.9269725000721,8.79130815741546));
#51964=CARTESIAN_POINT('Ctrl Pts',(14.5115747072029,36.8743539284632,8.80273172881855));
#51965=CARTESIAN_POINT('Ctrl Pts',(14.4838437603909,36.6988470726635,8.83973528280585));
#51966=CARTESIAN_POINT('Ctrl Pts',(14.4407294163151,36.3819306417377,8.89671331084956));
#51967=CARTESIAN_POINT('Ctrl Pts',(14.3981597821212,35.9572273355899,8.95236357748849));
#51968=CARTESIAN_POINT('Ctrl Pts',(14.3708736668771,35.5303620255068,8.98776686292775));
#51969=CARTESIAN_POINT('Ctrl Pts',(14.3621758928815,35.2107881186055,8.99900502627832));
#51970=CARTESIAN_POINT('Ctrl Pts',(14.3614066471014,35.0336685389156,9.0000000921457));
#51971=CARTESIAN_POINT('Ctrl Pts',(14.3614066770504,35.,9.00000019077833));
#51972=CARTESIAN_POINT('',(16.6650252178838,27.3912428642034,4.80695514514033));
#51973=CARTESIAN_POINT('Ctrl Pts',(14.361406677032,34.9999999999149,9.00000400682097));
#51974=CARTESIAN_POINT('Ctrl Pts',(14.3614067455746,34.9229644059056,9.00000228894048));
#51975=CARTESIAN_POINT('Ctrl Pts',(14.3621716465734,34.8458222221036,8.99901109367336));
#51976=CARTESIAN_POINT('Ctrl Pts',(14.3637083702908,34.7685726083627,8.99702402811064));
#51977=CARTESIAN_POINT('Ctrl Pts',(14.3643637517259,34.7356272180259,8.99617658503076));
#51978=CARTESIAN_POINT('Ctrl Pts',(14.3651594087391,34.7026622701312,8.99514768134809));
#51979=CARTESIAN_POINT('Ctrl Pts',(14.3660957379539,34.6696776740137,8.99393635384563));
#51980=CARTESIAN_POINT('Ctrl Pts',(14.368141414638,34.5976134703744,8.99128986542116));
#51981=CARTESIAN_POINT('Ctrl Pts',(14.3708587724685,34.5254555542841,8.98777262053586));
#51982=CARTESIAN_POINT('Ctrl Pts',(14.3742519630813,34.4532030581254,8.98337457196089));
#51983=CARTESIAN_POINT('Ctrl Pts',(14.3759485583877,34.417076810046,8.98117554767339));
#51984=CARTESIAN_POINT('Ctrl Pts',(14.3778141118918,34.3809269179434,8.97875632244572));
#51985=CARTESIAN_POINT('Ctrl Pts',(14.3798490775206,34.3447532465993,8.97611563701531));
#51986=CARTESIAN_POINT('Ctrl Pts',(14.3802164760517,34.3382223482266,8.97563888009407));
#51987=CARTESIAN_POINT('Ctrl Pts',(14.3805894168745,34.3316902734701,8.97515487505152));
#51988=CARTESIAN_POINT('Ctrl Pts',(14.3809678929735,34.3251572486695,8.97466362940566));
#51989=CARTESIAN_POINT('Ctrl Pts',(14.3826857394991,34.2955048241586,8.97243393873792));
#51990=CARTESIAN_POINT('Ctrl Pts',(14.3845179468002,34.2658321669791,8.97005452374758));
#51991=CARTESIAN_POINT('Ctrl Pts',(14.38645825802,34.2362277317391,8.9675331717211));
#51992=CARTESIAN_POINT('Ctrl Pts',(14.386942240259,34.2288433386044,8.96690425735596));
#51993=CARTESIAN_POINT('Ctrl Pts',(14.3874330028229,34.2214622199065,8.9662664337034));
#51994=CARTESIAN_POINT('Ctrl Pts',(14.3879304679243,34.2140854288794,8.96561979379566));
#51995=CARTESIAN_POINT('Ctrl Pts',(14.3904231202817,34.1771224831559,8.96237967004474));
#51996=CARTESIAN_POINT('Ctrl Pts',(14.3930858453617,34.1402354993775,8.95891587155103));
#51997=CARTESIAN_POINT('Ctrl Pts',(14.3959161528055,34.1034250643409,8.95523050427782));
#51998=CARTESIAN_POINT('Ctrl Pts',(14.401578406325,34.0297828825382,8.94785763605516));
#51999=CARTESIAN_POINT('Ctrl Pts',(14.4079114196966,33.9564470634377,8.93959804622122));
#52000=CARTESIAN_POINT('Ctrl Pts',(14.4148947404169,33.8834224278753,8.93046776632826));
#52001=CARTESIAN_POINT('Ctrl Pts',(14.4173568644703,33.8576759787415,8.92724868437009));
#52002=CARTESIAN_POINT('Ctrl Pts',(14.4198998096941,33.8319681413001,8.92392166901741));
#52003=CARTESIAN_POINT('Ctrl Pts',(14.4225226656181,33.8062991668918,8.92048723942206));
#52004=CARTESIAN_POINT('Ctrl Pts',(14.437045367563,33.6641705577073,8.90147086993391));
#52005=CARTESIAN_POINT('Ctrl Pts',(14.4540204796619,33.5232058055879,8.87915783660387));
#52006=CARTESIAN_POINT('Ctrl Pts',(14.4733045744892,33.3833637054076,8.85362171218632));
#52007=CARTESIAN_POINT('Ctrl Pts',(14.4901043922947,33.2615367892057,8.83137528363922));
#52008=CARTESIAN_POINT('Ctrl Pts',(14.5086565400091,33.1405622247914,8.80668273620936));
#52009=CARTESIAN_POINT('Ctrl Pts',(14.528867066016,33.0204133534421,8.77959205822056));
#52010=CARTESIAN_POINT('Ctrl Pts',(14.531855702318,33.0026463107421,8.77558601782092));
#52011=CARTESIAN_POINT('Ctrl Pts',(14.5348806033553,32.9848973261678,8.77152752638015));
#52012=CARTESIAN_POINT('Ctrl Pts',(14.5379414711734,32.9671663399968,8.76741662665445));
#52013=CARTESIAN_POINT('Ctrl Pts',(14.5617013275574,32.8295303132215,8.73550594220284));
#52014=CARTESIAN_POINT('Ctrl Pts',(14.5876282298979,32.6929783895085,8.70043733105985));
#52015=CARTESIAN_POINT('Ctrl Pts',(14.6155833207169,32.5574832879918,8.66223041570325));
#52016=CARTESIAN_POINT('Ctrl Pts',(14.6414955457034,32.4318897215896,8.62681553570283));
#52017=CARTESIAN_POINT('Ctrl Pts',(14.6691503114154,32.3072043916037,8.58870433773101));
#52018=CARTESIAN_POINT('Ctrl Pts',(14.6984381586483,32.1834048098462,8.54791153059053));
#52019=CARTESIAN_POINT('Ctrl Pts',(14.7007471515061,32.1736447087435,8.54469551066296));
#52020=CARTESIAN_POINT('Ctrl Pts',(14.7030662966404,32.1638901210945,8.54146278887225));
#52021=CARTESIAN_POINT('Ctrl Pts',(14.7053955412755,32.1541410394164,8.53821335745142));
#52022=CARTESIAN_POINT('Ctrl Pts',(14.7358712935118,32.0265844087048,8.49569791472005));
#52023=CARTESIAN_POINT('Ctrl Pts',(14.7680697416918,31.8999932610587,8.45033074738783));
#52024=CARTESIAN_POINT('Ctrl Pts',(14.8018905719573,31.7742858516999,8.40206928282887));
#52025=CARTESIAN_POINT('Ctrl Pts',(14.8034422614015,31.7685184338504,8.39985506145912));
#52026=CARTESIAN_POINT('Ctrl Pts',(14.8049972754406,31.7627532434756,8.39763487044287));
#52027=CARTESIAN_POINT('Ctrl Pts',(14.8065554841667,31.7569906915724,8.39540887856089));
#52028=CARTESIAN_POINT('Ctrl Pts',(14.8109956259332,31.7405702037661,8.38906587754876));
#52029=CARTESIAN_POINT('Ctrl Pts',(14.8154614065699,31.7241722485225,8.38267618919588));
#52030=CARTESIAN_POINT('Ctrl Pts',(14.8199480661342,31.7078127299217,8.37624629491226));
#52031=CARTESIAN_POINT('Ctrl Pts',(14.8231269392599,31.6962217381641,8.37169060758047));
#52032=CARTESIAN_POINT('Ctrl Pts',(14.8263172701105,31.6846464233617,8.36711332261336));
#52033=CARTESIAN_POINT('Ctrl Pts',(14.8295180624613,31.6730898846996,8.36251571506522));
#52034=CARTESIAN_POINT('Ctrl Pts',(14.8308348664555,31.6683355318386,8.36062426216231));
#52035=CARTESIAN_POINT('Ctrl Pts',(14.8321535683165,31.6635838810361,8.35872918832101));
#52036=CARTESIAN_POINT('Ctrl Pts',(14.8334741645343,31.6588349038253,8.35683048833469));
#52037=CARTESIAN_POINT('Ctrl Pts',(14.8414870867154,31.6300197487316,8.34530983195877));
#52038=CARTESIAN_POINT('Ctrl Pts',(14.8495681210058,31.6013090652414,8.33365808856993));
#52039=CARTESIAN_POINT('Ctrl Pts',(14.8577151002777,31.5727014456243,8.32187626795633));
#52040=CARTESIAN_POINT('Ctrl Pts',(14.8587809289823,31.5689588532916,8.32033491107015));
#52041=CARTESIAN_POINT('Ctrl Pts',(14.8598478861308,31.5652180246215,8.3187913282688));
#52042=CARTESIAN_POINT('Ctrl Pts',(14.860915967039,31.5614789566801,8.31724552153602));
#52043=CARTESIAN_POINT('Ctrl Pts',(14.8788752197154,31.4986083769142,8.29125354518811));
#52044=CARTESIAN_POINT('Ctrl Pts',(14.8971521820891,31.4362355887263,8.26463281026042));
#52045=CARTESIAN_POINT('Ctrl Pts',(14.9157246632579,31.3743466445316,8.23739265459531));
#52046=CARTESIAN_POINT('Ctrl Pts',(14.9544372820573,31.2453448658929,8.18061307018132));
#52047=CARTESIAN_POINT('Ctrl Pts',(14.9944326799355,31.11844401031,8.12114416072383));
#52048=CARTESIAN_POINT('Ctrl Pts',(15.0355234592335,30.9935371441862,8.05904804735394));
#52049=CARTESIAN_POINT('Ctrl Pts',(15.0760595854004,30.8703163007073,7.9977901221201));
#52050=CARTESIAN_POINT('Ctrl Pts',(15.1176617289772,30.7490358453888,7.9339756818053));
#52051=CARTESIAN_POINT('Ctrl Pts',(15.1601642196892,30.6296142683619,7.86763807383431));
#52052=CARTESIAN_POINT('Ctrl Pts',(15.1622801068849,30.6236691441707,7.86433561101518));
#52053=CARTESIAN_POINT('Ctrl Pts',(15.1643982264691,30.6177286273639,7.8610268947962));
#52054=CARTESIAN_POINT('Ctrl Pts',(15.1665185580527,30.6117927080271,7.85771192922444));
#52055=CARTESIAN_POINT('Ctrl Pts',(15.2069899929977,30.4984919511389,7.79443814010604));
#52056=CARTESIAN_POINT('Ctrl Pts',(15.2482654107132,30.3868625031313,7.72889267421188));
#52057=CARTESIAN_POINT('Ctrl Pts',(15.2902163323872,30.2768573280646,7.6610740248339));
#52058=CARTESIAN_POINT('Ctrl Pts',(15.3343650971648,30.1610888918886,7.58970230093732));
#52059=CARTESIAN_POINT('Ctrl Pts',(15.3792620199167,30.0471197248531,7.51581318575337));
#52060=CARTESIAN_POINT('Ctrl Pts',(15.4247582257832,29.9348963054931,7.43940391248849));
#52061=CARTESIAN_POINT('Ctrl Pts',(15.4300526658116,29.9218367513552,7.43051208717671));
#52062=CARTESIAN_POINT('Ctrl Pts',(15.4353552375342,29.908800835701,7.42158612927335));
#52063=CARTESIAN_POINT('Ctrl Pts',(15.440665704816,29.8957884768768,7.41262603449125));
#52064=CARTESIAN_POINT('Ctrl Pts',(15.4809891688668,29.7969829753231,7.34459020248898));
#52065=CARTESIAN_POINT('Ctrl Pts',(15.521768751821,29.6995358217372,7.27458636392175));
#52066=CARTESIAN_POINT('Ctrl Pts',(15.5629098190841,29.6034324184065,7.20258197486916));
#52067=CARTESIAN_POINT('Ctrl Pts',(15.6094690292766,29.4946725136796,7.12109484515398));
#52068=CARTESIAN_POINT('Ctrl Pts',(15.6564915273396,29.3876340000113,7.03704588777083));
#52069=CARTESIAN_POINT('Ctrl Pts',(15.703842272904,29.2822954725418,6.95038626702666));
#52070=CARTESIAN_POINT('Ctrl Pts',(15.7126024692674,29.2628071588042,6.93435367270424));
#52071=CARTESIAN_POINT('Ctrl Pts',(15.7213742769299,29.2433762270171,6.91823105084803));
#52072=CARTESIAN_POINT('Ctrl Pts',(15.7301564025366,29.2240035134661,6.90201887765802));
#52073=CARTESIAN_POINT('Ctrl Pts',(15.7424356426793,29.1969164262891,6.8793508839684));
#52074=CARTESIAN_POINT('Ctrl Pts',(15.7547351390208,29.1699434975136,6.85650729420062));
#52075=CARTESIAN_POINT('Ctrl Pts',(15.7670514039235,29.1430872338644,6.83348906854163));
#52076=CARTESIAN_POINT('Ctrl Pts',(15.769732737634,29.1372404446284,6.82847784599135));
#52077=CARTESIAN_POINT('Ctrl Pts',(15.7724151604062,29.1313985509808,6.82345778883465));
#52078=CARTESIAN_POINT('Ctrl Pts',(15.7750984165171,29.125562052055,6.8184293232226));
#52079=CARTESIAN_POINT('Ctrl Pts',(15.7847409247004,29.1045880986464,6.80035910599041));
#52080=CARTESIAN_POINT('Ctrl Pts',(15.7943975342148,29.0836765829379,6.78217404645932));
#52081=CARTESIAN_POINT('Ctrl Pts',(15.8040544431734,29.0628549878643,6.76389747888537));
#52082=CARTESIAN_POINT('Ctrl Pts',(15.8063269600534,29.0579551356988,6.75959653657584));
#52083=CARTESIAN_POINT('Ctrl Pts',(15.8085992529191,29.0530607734459,6.75529098841496));
#52084=CARTESIAN_POINT('Ctrl Pts',(15.8108712747456,29.0481719632851,6.75098089791873));
#52085=CARTESIAN_POINT('Ctrl Pts',(15.822798101834,29.0225084803134,6.72835536523916));
#52086=CARTESIAN_POINT('Ctrl Pts',(15.8347196337546,28.9969933066434,6.70560053229536));
#52087=CARTESIAN_POINT('Ctrl Pts',(15.8466338279487,28.9716252925335,6.68271643277414));
#52088=CARTESIAN_POINT('Ctrl Pts',(15.8571030335415,28.9493339859734,6.66260778431756));
#52089=CARTESIAN_POINT('Ctrl Pts',(15.8675665712898,28.9271563224226,6.64239933651428));
#52090=CARTESIAN_POINT('Ctrl Pts',(15.878023046609,28.9050915408951,6.62209112555336));
#52091=CARTESIAN_POINT('Ctrl Pts',(15.9151653987023,28.8267154285495,6.54995451174513));
#52092=CARTESIAN_POINT('Ctrl Pts',(15.9522184036771,28.7497626995228,6.47655981315418));
#52093=CARTESIAN_POINT('Ctrl Pts',(15.9891221859866,28.6742076578655,6.40190252027229));
#52094=CARTESIAN_POINT('Ctrl Pts',(16.0011265531405,28.6496304897914,6.37761737933574));
#52095=CARTESIAN_POINT('Ctrl Pts',(16.0131151358443,28.625201237453,6.35319865790895));
#52096=CARTESIAN_POINT('Ctrl Pts',(16.0250858673743,28.6009190188436,6.3286461898737));
#52097=CARTESIAN_POINT('Ctrl Pts',(16.0602757174407,28.5295376141228,6.25647034441588));
#52098=CARTESIAN_POINT('Ctrl Pts',(16.0953109612591,28.4594239273951,6.18314101673159));
#52099=CARTESIAN_POINT('Ctrl Pts',(16.1301419128974,28.3905688719057,6.10864380381399));
#52100=CARTESIAN_POINT('Ctrl Pts',(16.1768215075451,28.2982910004001,6.00880445008361));
#52101=CARTESIAN_POINT('Ctrl Pts',(16.2231343215003,28.2082737170057,5.90686754549628));
#52102=CARTESIAN_POINT('Ctrl Pts',(16.2689599967263,28.1204965528934,5.80279824132711));
#52103=CARTESIAN_POINT('Ctrl Pts',(16.2836188628206,28.0924181080365,5.76950821369913));
#52104=CARTESIAN_POINT('Ctrl Pts',(16.298227901363,28.0645688821045,5.73599997077043));
#52105=CARTESIAN_POINT('Ctrl Pts',(16.3127831594297,28.0369482046737,5.70227232738003));
#52106=CARTESIAN_POINT('Ctrl Pts',(16.3437296833362,27.9782227632899,5.63056261823559));
#52107=CARTESIAN_POINT('Ctrl Pts',(16.374433714844,27.9205304328504,5.5578613637537));
#52108=CARTESIAN_POINT('Ctrl Pts',(16.4048575296364,27.8638776557143,5.48414645965917));
#52109=CARTESIAN_POINT('Ctrl Pts',(16.4495907536865,27.7805790493436,5.375760797204));
#52110=CARTESIAN_POINT('Ctrl Pts',(16.4937185698648,27.6995280587495,5.26518414921598));
#52111=CARTESIAN_POINT('Ctrl Pts',(16.5371206449052,27.6207461836642,5.15234532909353));
#52112=CARTESIAN_POINT('Ctrl Pts',(16.553707506264,27.5906383135126,5.10922200230507));
#52113=CARTESIAN_POINT('Ctrl Pts',(16.5701882618752,27.5608617830849,5.0657681510329));
#52114=CARTESIAN_POINT('Ctrl Pts',(16.5865561886659,27.5314178413183,5.02197974299201));
#52115=CARTESIAN_POINT('Ctrl Pts',(16.6130174609297,27.4838171787808,4.95118904347443));
#52116=CARTESIAN_POINT('Ctrl Pts',(16.6391837396048,27.4370877369798,4.87952226067709));
#52117=CARTESIAN_POINT('Ctrl Pts',(16.665025217884,27.391242590013,4.8069553183639));
#52118=CARTESIAN_POINT('',(33.,27.3912430012986,4.80695505852859));
#52119=CARTESIAN_POINT('',(33.,27.3912430012986,4.80695505852859));
#52120=CARTESIAN_POINT('',(33.,26.2716828895474,2.19464813110884));
#52121=CARTESIAN_POINT('Origin',(33.,35.,5.81688018065629E-15));
#52122=CARTESIAN_POINT('',(33.,26.2716828895474,2.19464813110884));
#52123=CARTESIAN_POINT('Origin',(-37.5,48.4656487624794,-19.0077234952746));
#52124=CARTESIAN_POINT('',(-37.,47.5792333881917,-19.4706141780782));
#52125=CARTESIAN_POINT('',(-37.5,48.0436073736659,-18.7396170497563));
#52126=CARTESIAN_POINT('Ctrl Pts',(-37.5,48.0436073736659,-18.7396170497564));
#52127=CARTESIAN_POINT('Ctrl Pts',(-37.3614508889595,47.9693155542843,-18.8565639682411));
#52128=CARTESIAN_POINT('Ctrl Pts',(-37.1980436419056,47.8786620489552,-18.9992667339876));
#52129=CARTESIAN_POINT('Ctrl Pts',(-37.0447859999489,47.7259734976123,-19.2396223440145));
#52130=CARTESIAN_POINT('Ctrl Pts',(-37.,47.6475676678136,-19.3630453569726));
#52131=CARTESIAN_POINT('Ctrl Pts',(-37.,47.5792333881917,-19.4706141780782));
#52132=CARTESIAN_POINT('',(-37.,49.0018616535158,-18.1636407176477));
#52133=CARTESIAN_POINT('Origin',(-37.,48.4656487624794,-19.0077234952746));
#52134=CARTESIAN_POINT('',(-37.5,48.7337552079976,-18.5856821064611));
#52135=CARTESIAN_POINT('Origin',(-37.5,49.0018616535158,-18.1636407176477));
#52136=CARTESIAN_POINT('Origin',(-37.5,48.4656487624794,-19.0077234952746));
#52137=CARTESIAN_POINT('Origin',(3.49012810839377E-15,57.,-2.60208521396521E-14));
#52138=CARTESIAN_POINT('',(3.03365373473698E-15,20.5440037453175,14.5));
#52139=CARTESIAN_POINT('Origin',(1.25791587597333E-15,20.5440037453175,
-6.04998712603518E-15));
#52140=CARTESIAN_POINT('',(5.26586596715743E-15,57.,14.5));
#52141=CARTESIAN_POINT('',(5.26586596715743E-15,57.,14.5));
#52142=CARTESIAN_POINT('Origin',(3.49012810839377E-15,57.,-2.60208521396521E-14));
#52143=CARTESIAN_POINT('',(-14.5,38.9999999945948,6.54987201765396E-10));
#52144=CARTESIAN_POINT('',(-14.5,30.9999999945948,6.54993427017253E-10));
#52145=CARTESIAN_POINT('Ctrl Pts',(-14.5,38.9999999945948,6.54994392057517E-10));
#52146=CARTESIAN_POINT('Ctrl Pts',(-14.5000000000228,38.9999999945948,-0.505032330715858));
#52147=CARTESIAN_POINT('Ctrl Pts',(-14.4709879985074,38.8985352188743,-1.04196886987578));
#52148=CARTESIAN_POINT('Ctrl Pts',(-14.3661925074414,38.4894942453939,-2.0267475502792));
#52149=CARTESIAN_POINT('Ctrl Pts',(-14.2917945289831,38.1820590487641,-2.47479519466809));
#52150=CARTESIAN_POINT('Ctrl Pts',(-14.1511159999958,37.4747208857634,-3.18213335766881));
#52151=CARTESIAN_POINT('Ctrl Pts',(-14.0754408854234,37.0267038181377,-3.48951080938327));
#52152=CARTESIAN_POINT('Ctrl Pts',(-13.9676894199724,36.0420348868828,-3.8985094040844));
#52153=CARTESIAN_POINT('Ctrl Pts',(-13.9373598649543,35.5051384419502,-3.99999999934501));
#52154=CARTESIAN_POINT('Ctrl Pts',(-13.9373598649543,34.4948615472385,-3.99999999934501));
#52155=CARTESIAN_POINT('Ctrl Pts',(-13.9676894199725,33.9579651023051,-3.89850940408406));
#52156=CARTESIAN_POINT('Ctrl Pts',(-14.0754408854238,32.973296171049,-3.48951080938169));
#52157=CARTESIAN_POINT('Ctrl Pts',(-14.1511159999964,32.5252791034228,-3.18213335766633));
#52158=CARTESIAN_POINT('Ctrl Pts',(-14.2917945289836,31.817940940423,-2.47479519466472));
#52159=CARTESIAN_POINT('Ctrl Pts',(-14.3661925074417,31.5105057437941,-2.02674755027626));
#52160=CARTESIAN_POINT('Ctrl Pts',(-14.4709879985075,31.1014647703149,-1.04196886987411));
#52161=CARTESIAN_POINT('Ctrl Pts',(-14.5000000000228,30.9999999945948,-0.505032330715019));
#52162=CARTESIAN_POINT('Ctrl Pts',(-14.5,30.9999999945948,6.5499272672298E-10));
#52163=CARTESIAN_POINT('Ctrl Pts',(-14.5,30.9999999945948,6.54993420612371E-10));
#52164=CARTESIAN_POINT('Ctrl Pts',(-14.4999999999772,30.9999999945948,0.505032332030019));
#52165=CARTESIAN_POINT('Ctrl Pts',(-14.4709879984128,31.1014647703167,1.04196887119144));
#52166=CARTESIAN_POINT('Ctrl Pts',(-14.3661925072559,31.5105057437989,2.02674755159486));
#52167=CARTESIAN_POINT('Ctrl Pts',(-14.2917945287556,31.8179409404289,2.4747951959824));
#52168=CARTESIAN_POINT('Ctrl Pts',(-14.1511159997011,32.5252791034279,3.18213335897963));
#52169=CARTESIAN_POINT('Ctrl Pts',(-14.0754408850987,32.9732961710517,3.48951081069302));
#52170=CARTESIAN_POINT('Ctrl Pts',(-13.967689419607,33.9579651023049,3.89850940539377));
#52171=CARTESIAN_POINT('Ctrl Pts',(-13.9373598645784,34.4948615472378,4.000000000655));
#52172=CARTESIAN_POINT('Ctrl Pts',(-13.9373598645784,34.9999999945948,4.000000000655));
#52173=CARTESIAN_POINT('Ctrl Pts',(-13.9373598645784,35.5051384419526,4.000000000655));
#52174=CARTESIAN_POINT('Ctrl Pts',(-13.9676894196071,36.0420348868864,3.89850940539344));
#52175=CARTESIAN_POINT('Ctrl Pts',(-14.0754408850991,37.0267038181408,3.48951081069144));
#52176=CARTESIAN_POINT('Ctrl Pts',(-14.1511159997017,37.474720885765,3.18213335897715));
#52177=CARTESIAN_POINT('Ctrl Pts',(-14.2917945287562,38.1820590487631,2.47479519597904));
#52178=CARTESIAN_POINT('Ctrl Pts',(-14.3661925072563,38.4894942453923,2.02674755159192));
#52179=CARTESIAN_POINT('Ctrl Pts',(-14.4709879984129,38.8985352188732,1.04196887118977));
#52180=CARTESIAN_POINT('Ctrl Pts',(-14.4999999999772,38.9999999945948,0.505032332029179));
#52181=CARTESIAN_POINT('Ctrl Pts',(-14.5,38.9999999945948,6.54993420612371E-10));
#52182=CARTESIAN_POINT('',(14.5,38.9999999945947,6.54966782784404E-10));
#52183=CARTESIAN_POINT('',(14.5,30.9999999945948,6.54993843350887E-10));
#52184=CARTESIAN_POINT('Ctrl Pts',(14.5,38.9999999945948,6.54992587945102E-10));
#52185=CARTESIAN_POINT('Ctrl Pts',(14.4999999999772,38.9999999945948,0.505032332030019));
#52186=CARTESIAN_POINT('Ctrl Pts',(14.4709879984128,38.8985352188729,1.04196887119144));
#52187=CARTESIAN_POINT('Ctrl Pts',(14.3661925072559,38.4894942453907,2.02674755159486));
#52188=CARTESIAN_POINT('Ctrl Pts',(14.2917945287556,38.1820590487606,2.4747951959824));
#52189=CARTESIAN_POINT('Ctrl Pts',(14.1511159997011,37.4747208857617,3.18213335897963));
#52190=CARTESIAN_POINT('Ctrl Pts',(14.0754408850987,37.0267038181379,3.48951081069302));
#52191=CARTESIAN_POINT('Ctrl Pts',(13.967689419607,36.0420348868847,3.89850940539377));
#52192=CARTESIAN_POINT('Ctrl Pts',(13.9373598645784,35.5051384419518,4.000000000655));
#52193=CARTESIAN_POINT('Ctrl Pts',(13.9373598645784,34.9999999945948,4.000000000655));
#52194=CARTESIAN_POINT('Ctrl Pts',(13.9373598645784,34.4948615472378,4.000000000655));
#52195=CARTESIAN_POINT('Ctrl Pts',(13.967689419607,33.9579651023049,3.89850940539377));
#52196=CARTESIAN_POINT('Ctrl Pts',(14.0754408850987,32.9732961710517,3.48951081069302));
#52197=CARTESIAN_POINT('Ctrl Pts',(14.1511159997011,32.5252791034279,3.18213335897963));
#52198=CARTESIAN_POINT('Ctrl Pts',(14.2917945287556,31.8179409404289,2.4747951959824));
#52199=CARTESIAN_POINT('Ctrl Pts',(14.3661925072559,31.5105057437989,2.02674755159486));
#52200=CARTESIAN_POINT('Ctrl Pts',(14.4709879984128,31.1014647703167,1.04196887119144));
#52201=CARTESIAN_POINT('Ctrl Pts',(14.4999999999772,30.9999999945948,0.50503233203002));
#52202=CARTESIAN_POINT('Ctrl Pts',(14.5,30.9999999945948,6.54994253279639E-10));
#52203=CARTESIAN_POINT('Ctrl Pts',(14.5,30.9999999945948,6.54993975723883E-10));
#52204=CARTESIAN_POINT('Ctrl Pts',(14.5000000000228,30.9999999945948,-0.505032330715018));
#52205=CARTESIAN_POINT('Ctrl Pts',(14.4709879985075,31.1014647703149,-1.04196886987411));
#52206=CARTESIAN_POINT('Ctrl Pts',(14.3661925074417,31.5105057437941,-2.02674755027626));
#52207=CARTESIAN_POINT('Ctrl Pts',(14.2917945289836,31.817940940423,-2.47479519466472));
#52208=CARTESIAN_POINT('Ctrl Pts',(14.1511159999964,32.5252791034228,-3.18213335766633));
#52209=CARTESIAN_POINT('Ctrl Pts',(14.0754408854238,32.973296171049,-3.48951080938169));
#52210=CARTESIAN_POINT('Ctrl Pts',(13.9676894199725,33.9579651023051,-3.89850940408406));
#52211=CARTESIAN_POINT('Ctrl Pts',(13.9373598649543,34.4948615472385,-3.99999999934501));
#52212=CARTESIAN_POINT('Ctrl Pts',(13.9373598649543,35.5051384419511,-3.99999999934501));
#52213=CARTESIAN_POINT('Ctrl Pts',(13.9676894199725,36.0420348868845,-3.89850940408406));
#52214=CARTESIAN_POINT('Ctrl Pts',(14.0754408854238,37.0267038181406,-3.48951080938169));
#52215=CARTESIAN_POINT('Ctrl Pts',(14.1511159999964,37.4747208857667,-3.18213335766633));
#52216=CARTESIAN_POINT('Ctrl Pts',(14.2917945289836,38.1820590487666,-2.47479519466473));
#52217=CARTESIAN_POINT('Ctrl Pts',(14.3661925074418,38.4894942453955,-2.02674755027626));
#52218=CARTESIAN_POINT('Ctrl Pts',(14.4709879985075,38.8985352188747,-1.0419688698741));
#52219=CARTESIAN_POINT('Ctrl Pts',(14.5000000000228,38.9999999945948,-0.505032330715019));
#52220=CARTESIAN_POINT('Ctrl Pts',(14.5,38.9999999945948,6.5499272672298E-10));
#52221=CARTESIAN_POINT('Ctrl Pts',(0.321034048597817,44.2777095070773,-16.496876587392));
#52222=CARTESIAN_POINT('Ctrl Pts',(0.334078182671872,44.0705712895835,-16.4966227447236));
#52223=CARTESIAN_POINT('Ctrl Pts',(0.346147593727982,43.9243235322772,-16.6433959637249));
#52224=CARTESIAN_POINT('Ctrl Pts',(0.307535768851996,44.2768333852379,-16.497139267868));
#52225=CARTESIAN_POINT('Ctrl Pts',(0.32115157242211,44.0697030498192,-16.4968849768605));
#52226=CARTESIAN_POINT('Ctrl Pts',(0.333504576783726,43.9234749343164,-16.6436941271133));
#52227=CARTESIAN_POINT('Ctrl Pts',(0.294017346932686,44.2758981934479,-16.4973857263738));
#52228=CARTESIAN_POINT('Ctrl Pts',(0.308206040614918,44.0687776043361,-16.4971323872042));
#52229=CARTESIAN_POINT('Ctrl Pts',(0.320842694094729,43.9225707071434,-16.6439790196373));
#52230=CARTESIAN_POINT('Ctrl Pts',(0.267039396841221,44.27391662747,-16.4978444642199));
#52231=CARTESIAN_POINT('Ctrl Pts',(0.282371646107752,44.0668191614445,-16.4975958245399));
#52232=CARTESIAN_POINT('Ctrl Pts',(0.295574090707277,43.9206577286911,-16.6445202461941));
#52233=CARTESIAN_POINT('Ctrl Pts',(0.253563318677811,44.2728691821441,-16.4980570656251));
#52234=CARTESIAN_POINT('Ctrl Pts',(0.269466916331725,44.0657850965016,-16.4978121729084));
#52235=CARTESIAN_POINT('Ctrl Pts',(0.282951868731823,43.9196479380401,-16.644776944703));
#52236=CARTESIAN_POINT('Ctrl Pts',(0.213173600931101,44.2695576149692,-16.4986448596443));
#52237=CARTESIAN_POINT('Ctrl Pts',(0.230789208343801,44.0625190499157,-16.4984153937458));
#52238=CARTESIAN_POINT('Ctrl Pts',(0.245121279113449,43.9164593690092,-16.6455055488628));
#52239=CARTESIAN_POINT('Ctrl Pts',(0.186298475258698,44.2671242747577,-16.4989700430965));
#52240=CARTESIAN_POINT('Ctrl Pts',(0.205054254630706,44.0601233301731,-16.4987564104361));
#52241=CARTESIAN_POINT('Ctrl Pts',(0.219948985085661,43.9141214063132,-16.6459359637993));
#52242=CARTESIAN_POINT('Ctrl Pts',(0.105825878010724,44.2591529071548,-16.4997478557418));
#52243=CARTESIAN_POINT('Ctrl Pts',(0.127994124910921,44.0522861114256,-16.4995982912245));
#52244=CARTESIAN_POINT('Ctrl Pts',(0.144575202554741,43.906475946942,-16.6470632548686));
#52245=CARTESIAN_POINT('Ctrl Pts',(0.0523811410166356,44.2529437369118,
-16.5000027615431));
#52246=CARTESIAN_POINT('Ctrl Pts',(0.0768198248561238,44.0461951243862,
-16.4999178604957));
#52247=CARTESIAN_POINT('Ctrl Pts',(0.0945167711882191,43.9005370741829,
-16.6475961824246));
#52248=CARTESIAN_POINT('Ctrl Pts',(-0.107350614477069,44.2316680864431,
-16.4999944092424));
#52249=CARTESIAN_POINT('Ctrl Pts',(-0.0761321294294826,44.0253574854767,
-16.5001684527276));
#52250=CARTESIAN_POINT('Ctrl Pts',(-0.0550942394312359,43.8802288896034,
-16.6485550431313));
#52251=CARTESIAN_POINT('Ctrl Pts',(-0.213035833808924,44.2139564350666,
-16.4989582457926));
#52252=CARTESIAN_POINT('Ctrl Pts',(-0.177314759062477,44.0080500010336,
-16.4993908078766));
#52253=CARTESIAN_POINT('Ctrl Pts',(-0.154083150146027,43.8633708391614,
-16.6483410814393));
#52254=CARTESIAN_POINT('Ctrl Pts',(-0.422829790157967,44.1715971665048,
-16.4949150477184));
#52255=CARTESIAN_POINT('Ctrl Pts',(-0.378133313017958,43.9667246375007,
-16.4960324415121));
#52256=CARTESIAN_POINT('Ctrl Pts',(-0.350584376434533,43.8231263425323,
-16.6462901344215));
#52257=CARTESIAN_POINT('Ctrl Pts',(-0.526938468414131,44.1469492910955,
-16.491907937397));
#52258=CARTESIAN_POINT('Ctrl Pts',(-0.477778440005314,43.9427009960084,
-16.4934505609926));
#52259=CARTESIAN_POINT('Ctrl Pts',(-0.448096637091592,43.7997396541264,
-16.6444530862772));
#52260=CARTESIAN_POINT('Ctrl Pts',(-0.733587594662706,44.0907445802113,
-16.4840086388606));
#52261=CARTESIAN_POINT('Ctrl Pts',(-0.675522285528619,43.8879685573675,
-16.4865649802999));
#52262=CARTESIAN_POINT('Ctrl Pts',(-0.641652292512058,43.7464596423238,
-16.6392391144044));
#52263=CARTESIAN_POINT('Ctrl Pts',(-0.836128020523552,44.0591876523663,
-16.4791163820797));
#52264=CARTESIAN_POINT('Ctrl Pts',(-0.773630842788747,43.85725253155,-16.4822597770412));
#52265=CARTESIAN_POINT('Ctrl Pts',(-0.737695666593328,43.7165662342863,
-16.6358621269656));
#52266=CARTESIAN_POINT('Ctrl Pts',(-0.988754343263762,44.0066257334661,
-16.4704268781621));
#52267=CARTESIAN_POINT('Ctrl Pts',(-0.919592667679679,43.8061296100387,
-16.4745719708769));
#52268=CARTESIAN_POINT('Ctrl Pts',(-0.880651450997229,43.6668004399974,
-16.62970542955));
#52269=CARTESIAN_POINT('Ctrl Pts',(-1.03943225076959,43.988233336078,-16.4673051794513));
#52270=CARTESIAN_POINT('Ctrl Pts',(-0.968061533919264,43.7882402439072,
-16.471803341561));
#52271=CARTESIAN_POINT('Ctrl Pts',(-0.92811836158864,43.6493902559039,-16.6274713470767));
#52272=CARTESIAN_POINT('Ctrl Pts',(-1.11515046567206,43.9593254565497,-16.462292648905));
#52273=CARTESIAN_POINT('Ctrl Pts',(-1.04046157511159,43.760131242437,-16.4673503544702));
#52274=CARTESIAN_POINT('Ctrl Pts',(-0.999039003666644,43.6220311175392,
-16.6238556629229));
#52275=CARTESIAN_POINT('Ctrl Pts',(-1.14034008702055,43.9494695740836,-16.4605668083992));
#52276=CARTESIAN_POINT('Ctrl Pts',(-1.06454821112494,43.7505474186053,-16.4658157518771));
#52277=CARTESIAN_POINT('Ctrl Pts',(-1.02263258838498,43.6127040541935,-16.6226063432779));
#52278=CARTESIAN_POINT('Ctrl Pts',(-1.19061925892548,43.9293155100069,-16.4570064394505));
#52279=CARTESIAN_POINT('Ctrl Pts',(-1.11262228707775,43.7309512076575,-16.4626476168865));
#52280=CARTESIAN_POINT('Ctrl Pts',(-1.06972602765263,43.5936328230074,-16.6200209173139));
#52281=CARTESIAN_POINT('Ctrl Pts',(-1.21573107838862,43.9190077883623,-16.4551701883059));
#52282=CARTESIAN_POINT('Ctrl Pts',(-1.13663118653057,43.7209293797071,-16.4610125155677));
#52283=CARTESIAN_POINT('Ctrl Pts',(-1.09324674012034,43.5838796294641,-16.618683550189));
#52284=CARTESIAN_POINT('Ctrl Pts',(-1.3406740926079,43.8665114056024,-16.4457484072491));
#52285=CARTESIAN_POINT('Ctrl Pts',(-1.25611592982861,43.6698761529651,-16.4526150324278));
#52286=CARTESIAN_POINT('Ctrl Pts',(-1.21027325465697,43.5342106859547,-16.6118037002477));
#52287=CARTESIAN_POINT('Ctrl Pts',(-1.43874378672612,43.8214268381111,-16.4374378027854));
#52288=CARTESIAN_POINT('Ctrl Pts',(-1.34984750421121,43.6260493224596,-16.445193094768));
#52289=CARTESIAN_POINT('Ctrl Pts',(-1.3021291667423,43.4915646194171,-16.6056797596469));
#52290=CARTESIAN_POINT('Ctrl Pts',(-1.72749788443196,43.6771991720061,-16.4104580032492));
#52291=CARTESIAN_POINT('Ctrl Pts',(-1.62585456299005,43.4858144841423,-16.4210581992283));
#52292=CARTESIAN_POINT('Ctrl Pts',(-1.5725875499331,43.3551562723534,-16.5857017103286));
#52293=CARTESIAN_POINT('Ctrl Pts',(-1.9127446936616,43.5691113883,-16.3897439917078));
#52294=CARTESIAN_POINT('Ctrl Pts',(-1.80274205830027,43.3807393221566,-16.4024878858354));
#52295=CARTESIAN_POINT('Ctrl Pts',(-1.74609695837727,43.2529516481594,-16.5702431598975));
#52296=CARTESIAN_POINT('Ctrl Pts',(-2.1801557392676,43.3896071926388,-16.3555799666888));
#52297=CARTESIAN_POINT('Ctrl Pts',(-2.05760446502451,43.2064579036073,-16.3718931324892));
#52298=CARTESIAN_POINT('Ctrl Pts',(-1.99656460420932,43.0832067018407,-16.5448031114995));
#52299=CARTESIAN_POINT('Ctrl Pts',(-2.26754491058278,43.3268692367125,-16.3436754924434));
#52300=CARTESIAN_POINT('Ctrl Pts',(-2.14090553035905,43.1454987345458,-16.3612235417513));
#52301=CARTESIAN_POINT('Ctrl Pts',(-2.07841672068826,43.0238779812105,-16.5359471304104));
#52302=CARTESIAN_POINT('Ctrl Pts',(-2.39602241125449,43.2284104250473,-16.3251630538784));
#52303=CARTESIAN_POINT('Ctrl Pts',(-2.26324112913542,43.0498815519994,-16.3446457798798));
#52304=CARTESIAN_POINT('Ctrl Pts',(-2.19875377361068,42.9307615436581,-16.5222160833336));
#52305=CARTESIAN_POINT('Ctrl Pts',(-2.4384136297981,43.1948651021794,-16.3188829280199));
#52306=CARTESIAN_POINT('Ctrl Pts',(-2.30360778271325,43.0172911666837,-16.3390206470251));
#52307=CARTESIAN_POINT('Ctrl Pts',(-2.23845904720143,42.8990351188427,-16.5175645484453));
#52308=CARTESIAN_POINT('Ctrl Pts',(-2.5013483955168,43.1434553651894,-16.3093134885055));
#52309=CARTESIAN_POINT('Ctrl Pts',(-2.36350239470388,42.9673565647272,-16.3304535133341));
#52310=CARTESIAN_POINT('Ctrl Pts',(-2.29740621067309,42.8504103436033,-16.5104900878419));
#52311=CARTESIAN_POINT('Ctrl Pts',(-2.52221795974619,43.1261368034609,-16.3060987995381));
#52312=CARTESIAN_POINT('Ctrl Pts',(-2.38336413494237,42.9505314385688,-16.3275753119188));
#52313=CARTESIAN_POINT('Ctrl Pts',(-2.31695346092089,42.8340295394261,-16.508115741492));
#52314=CARTESIAN_POINT('Ctrl Pts',(-2.56373951624231,43.0911348998851,-16.2996221180008));
#52315=CARTESIAN_POINT('Ctrl Pts',(-2.42287279694903,42.9165270650644,-16.321777494731));
#52316=CARTESIAN_POINT('Ctrl Pts',(-2.3558441749912,42.8009219471062,-16.5033371082496));
#52317=CARTESIAN_POINT('Ctrl Pts',(-2.58440772848289,43.0734372910358,-16.2963575090795));
#52318=CARTESIAN_POINT('Ctrl Pts',(-2.44253529767474,42.8993336069646,-16.3188554855158));
#52319=CARTESIAN_POINT('Ctrl Pts',(-2.37520283114705,42.7841816631336,-16.5009308965196));
#52320=CARTESIAN_POINT('Ctrl Pts',(-2.76898876271576,42.9129091805958,-16.2668469274607));
#52321=CARTESIAN_POINT('Ctrl Pts',(-2.61835540789446,42.7431513199272,-16.2924080344925));
#52322=CARTESIAN_POINT('Ctrl Pts',(-2.54808864778449,42.6323323225514,-16.4792048254679));
#52323=CARTESIAN_POINT('Ctrl Pts',(-2.92301708649477,42.7613001461326,-16.2396947338131));
#52324=CARTESIAN_POINT('Ctrl Pts',(-2.76462847126197,42.5957682985728,-16.2681310777436));
#52325=CARTESIAN_POINT('Ctrl Pts',(-2.69235760204375,42.488886199182,-16.4593927479317));
#52326=CARTESIAN_POINT('Ctrl Pts',(-3.21259129366432,42.4414613853005,-16.1848994780706));
#52327=CARTESIAN_POINT('Ctrl Pts',(-3.03897378350019,42.2850128986459,-16.2192940222789));
#52328=CARTESIAN_POINT('Ctrl Pts',(-2.96358413143859,42.1861517320565,-16.4200413247235));
#52329=CARTESIAN_POINT('Ctrl Pts',(-3.34812899112022,42.2732247223232,-16.1572537757578));
#52330=CARTESIAN_POINT('Ctrl Pts',(-3.16707816112672,42.1214334676319,-16.1947098049125));
#52331=CARTESIAN_POINT('Ctrl Pts',(-3.09053404151204,42.0268568930642,-16.4004996968118));
#52332=CARTESIAN_POINT('Ctrl Pts',(-3.53828868842179,42.0088979382797,-16.1162873356813));
#52333=CARTESIAN_POINT('Ctrl Pts',(-3.34597462567252,41.8649168770618,-16.1584948890192));
#52334=CARTESIAN_POINT('Ctrl Pts',(-3.26864505239508,41.7764635010048,-16.3722252421456));
#52335=CARTESIAN_POINT('Ctrl Pts',(-3.5994799346103,41.9187901440346,-16.1027143504919));
#52336=CARTESIAN_POINT('Ctrl Pts',(-3.40351260983138,41.7773425460961,-16.1465055224545));
#52337=CARTESIAN_POINT('Ctrl Pts',(-3.32595916749315,41.6910871652366,-16.362972412406));
#52338=CARTESIAN_POINT('Ctrl Pts',(-3.67327289887432,41.8036856256223,-16.0859347036074));
#52339=CARTESIAN_POINT('Ctrl Pts',(-3.47268299468521,41.6656131275086,-16.1317391824527));
#52340=CARTESIAN_POINT('Ctrl Pts',(-3.3950765443778,41.5820004939642,-16.3517021387782));
#52341=CARTESIAN_POINT('Ctrl Pts',(-3.68790324489889,41.7805305132082,-16.0825865601582));
#52342=CARTESIAN_POINT('Ctrl Pts',(-3.48640397870713,41.6431129782816,-16.1287915877042));
#52343=CARTESIAN_POINT('Ctrl Pts',(-3.40877989888389,41.5600546868429,-16.3494618416137));
#52344=CARTESIAN_POINT('Ctrl Pts',(-3.71686467531462,41.7340227710879,-16.0759179456141));
#52345=CARTESIAN_POINT('Ctrl Pts',(-3.51355022417322,41.5979213056804,-16.122924842068));
#52346=CARTESIAN_POINT('Ctrl Pts',(-3.43590630737669,41.5159732371528,-16.3450174403968));
#52347=CARTESIAN_POINT('Ctrl Pts',(-3.73118318182571,41.7106906886745,-16.0726003938663));
#52348=CARTESIAN_POINT('Ctrl Pts',(-3.52696370022908,41.5752492629553,-16.1200082324879));
#52349=CARTESIAN_POINT('Ctrl Pts',(-3.44931758085173,41.493857071485,-16.3428152733996));
#52350=CARTESIAN_POINT('Ctrl Pts',(-3.77365910783509,41.6404628298273,-16.0627003448006));
#52351=CARTESIAN_POINT('Ctrl Pts',(-3.56674649451528,41.5069837011863,-16.1113077604514));
#52352=CARTESIAN_POINT('Ctrl Pts',(-3.48910219450987,41.427285026544,-16.3362710369363));
#52353=CARTESIAN_POINT('Ctrl Pts',(-3.80133703055952,41.5933354841588,-16.0561704793561));
#52354=CARTESIAN_POINT('Ctrl Pts',(-3.59262873818026,41.4611883744804,-16.105579589636));
#52355=CARTESIAN_POINT('Ctrl Pts',(-3.51502641995466,41.3826056395206,-16.3319912551902));
#52356=CARTESIAN_POINT('Ctrl Pts',(-3.93661737229858,41.3561924516797,-16.0239016028219));
#52357=CARTESIAN_POINT('Ctrl Pts',(-3.71926534359318,41.2302267666986,-16.0772522172006));
#52358=CARTESIAN_POINT('Ctrl Pts',(-3.64173527925152,41.1577530499255,-16.3110349773682));
#52359=CARTESIAN_POINT('Ctrl Pts',(-4.03491747293985,41.1616690216634,-15.9993106710039));
#52360=CARTESIAN_POINT('Ctrl Pts',(-3.8105351856191,41.0410889990247,-16.0558581848326));
#52361=CARTESIAN_POINT('Ctrl Pts',(-3.73380699989436,40.9732232360452,-16.2956924811267));
#52362=CARTESIAN_POINT('Ctrl Pts',(-4.21346560575097,40.7637707951905,-15.9532193788555));
#52363=CARTESIAN_POINT('Ctrl Pts',(-3.97517918815052,40.6545075845859,-16.0161173849287));
#52364=CARTESIAN_POINT('Ctrl Pts',(-3.90104216471963,40.5955698374873,-16.2684493117706));
#52365=CARTESIAN_POINT('Ctrl Pts',(-4.29370773194948,40.5603934046897,-15.9317175178876));
#52366=CARTESIAN_POINT('Ctrl Pts',(-4.04850396862992,40.4567958249106,-15.9977704901831));
#52367=CARTESIAN_POINT('Ctrl Pts',(-3.97620007983221,40.4024438484038,-16.2565472800635));
#52368=CARTESIAN_POINT('Ctrl Pts',(-4.40146481480481,40.2490824569658,-15.9021537778166));
#52369=CARTESIAN_POINT('Ctrl Pts',(-4.14571728004939,40.1550827275247,-15.9729333571334));
#52370=CARTESIAN_POINT('Ctrl Pts',(-4.0771295784449,40.1066679258703,-16.2416226946648));
#52371=CARTESIAN_POINT('Ctrl Pts',(-4.43527916848801,40.1442697315678,-15.8927463879809));
#52372=CARTESIAN_POINT('Ctrl Pts',(-4.17607991924084,40.0532812588022,-15.965075967575));
#52373=CARTESIAN_POINT('Ctrl Pts',(-4.10880142516048,40.007059981848,-16.2371350135424));
#52374=CARTESIAN_POINT('Ctrl Pts',(-4.47498970331547,40.0119814226891,-15.8815784864466));
#52375=CARTESIAN_POINT('Ctrl Pts',(-4.21141132770978,39.9250565429304,-15.955847181276));
#52376=CARTESIAN_POINT('Ctrl Pts',(-4.14599586533176,39.8813077925278,-16.2321648104482));
#52377=CARTESIAN_POINT('Ctrl Pts',(-4.48280713505993,39.9854484820733,-15.8793735332333));
#52378=CARTESIAN_POINT('Ctrl Pts',(-4.21836394867178,39.8992957517518,-15.9540264515764));
#52379=CARTESIAN_POINT('Ctrl Pts',(-4.15331797782398,39.8560841569777,-16.2312023454786));
#52380=CARTESIAN_POINT('Ctrl Pts',(-4.49815720553132,39.9323631382508,-15.8750321376815));
#52381=CARTESIAN_POINT('Ctrl Pts',(-4.23198682506552,39.8477579670653,-15.9504505711255));
#52382=CARTESIAN_POINT('Ctrl Pts',(-4.16769545413477,39.805615099322,-16.2293456787121));
#52383=CARTESIAN_POINT('Ctrl Pts',(-4.50569299128003,39.9058006819841,-15.8728948158664));
#52384=CARTESIAN_POINT('Ctrl Pts',(-4.23865969846769,39.8219707212385,-15.9486947308374));
#52385=CARTESIAN_POINT('Ctrl Pts',(-4.1747537660165,39.7803601224423,-16.2284510688984));
#52386=CARTESIAN_POINT('Ctrl Pts',(-4.52788908225558,39.8260548181995,-15.8665830325155));
#52387=CARTESIAN_POINT('Ctrl Pts',(-4.25828083324603,39.7445109973632,-15.9435203785516));
#52388=CARTESIAN_POINT('Ctrl Pts',(-4.19554349286319,39.7045346637349,-16.2258684245472));
#52389=CARTESIAN_POINT('Ctrl Pts',(-4.54213820519509,39.7728129265089,-15.8625087615832));
#52390=CARTESIAN_POINT('Ctrl Pts',(-4.27080745248769,39.6928283677743,-15.9402013833087));
#52391=CARTESIAN_POINT('Ctrl Pts',(-4.20888977911923,39.6539036641976,-16.2242815829051));
#52392=CARTESIAN_POINT('Ctrl Pts',(-4.61072350551952,39.5062243012366,-15.8428055513534));
#52393=CARTESIAN_POINT('Ctrl Pts',(-4.33101064476337,39.4331423066517,-15.9241892497505));
#52394=CARTESIAN_POINT('Ctrl Pts',(-4.27312945361112,39.4003554433727,-16.2170217104017));
#52395=CARTESIAN_POINT('Ctrl Pts',(-4.65710151667135,39.2917430094221,-15.8291830985343));
#52396=CARTESIAN_POINT('Ctrl Pts',(-4.37047377111817,39.2249262086857,-15.9134966630587));
#52397=CARTESIAN_POINT('Ctrl Pts',(-4.3165689141374,39.1962612675561,-16.2133735716419));
#52398=CARTESIAN_POINT('Ctrl Pts',(-4.73455890330831,38.860584008785,-15.8061881582692));
#52399=CARTESIAN_POINT('Ctrl Pts',(-4.43416228480996,38.806836206605,-15.8961542515918));
#52400=CARTESIAN_POINT('Ctrl Pts',(-4.38911853157358,38.7857773011577,-16.2103568495108));
#52401=CARTESIAN_POINT('Ctrl Pts',(-4.7656335172996,38.6439056908728,-15.7968150887316));
#52402=CARTESIAN_POINT('Ctrl Pts',(-4.45824992940577,38.596715083291,-15.8895386759589));
#52403=CARTESIAN_POINT('Ctrl Pts',(-4.41822423140701,38.5793869570085,-16.2109877211159));
#52404=CARTESIAN_POINT('Ctrl Pts',(-4.81366277021719,38.2085119119448,-15.7822457370113));
#52405=CARTESIAN_POINT('Ctrl Pts',(-4.49228715046657,38.1750784013236,-15.8802583836643));
#52406=CARTESIAN_POINT('Ctrl Pts',(-4.46321030786492,38.1644661155498,-16.2164498115114));
#52407=CARTESIAN_POINT('Ctrl Pts',(-4.83061473177268,37.989796110882,-15.7770490650161));
#52408=CARTESIAN_POINT('Ctrl Pts',(-4.50207912059962,37.963297937123,-15.8776364690345));
#52409=CARTESIAN_POINT('Ctrl Pts',(-4.47908817873774,37.9559353121758,-16.2212806621887));
#52410=CARTESIAN_POINT('Ctrl Pts',(-4.85119740418559,37.5504372754616,-15.7707323746352));
#52411=CARTESIAN_POINT('Ctrl Pts',(-4.50825772146479,37.5385831425256,-15.8762196986871));
#52412=CARTESIAN_POINT('Ctrl Pts',(-4.49836671444632,37.5368431558517,-16.2350392361057));
#52413=CARTESIAN_POINT('Ctrl Pts',(-4.85482680237322,37.3297940775806,-15.7696120833341));
#52414=CARTESIAN_POINT('Ctrl Pts',(-4.50446088793284,37.3253626831583,-15.8774765117451));
#52415=CARTESIAN_POINT('Ctrl Pts',(-4.50176615109278,37.3262816596819,-16.2439666982713));
#52416=CARTESIAN_POINT('Ctrl Pts',(-4.85133542686646,37.0528279294366,-15.7706862599499));
#52417=CARTESIAN_POINT('Ctrl Pts',(-4.49167305004904,37.059789020437,-15.8813246755956));
#52418=CARTESIAN_POINT('Ctrl Pts',(-4.49849599207902,37.0618545761177,-16.2576124902641));
#52419=CARTESIAN_POINT('Ctrl Pts',(-4.85023355700303,36.9973424024009,-15.7710252327459));
#52420=CARTESIAN_POINT('Ctrl Pts',(-4.4886839703737,37.0062991010676,-15.8822165992224));
#52421=CARTESIAN_POINT('Ctrl Pts',(-4.49746393778067,37.0088752437307,-16.2604679296177));
#52422=CARTESIAN_POINT('Ctrl Pts',(-4.84724165567112,36.8866091092228,-15.7719450538262));
#52423=CARTESIAN_POINT('Ctrl Pts',(-4.48191083668474,36.8995910435531,-15.884223449632));
#52424=CARTESIAN_POINT('Ctrl Pts',(-4.49466160577087,36.9031322050459,-16.2664058785488));
#52425=CARTESIAN_POINT('Ctrl Pts',(-4.84535166014932,36.8313248270939,-15.7725258903161));
#52426=CARTESIAN_POINT('Ctrl Pts',(-4.47812221634299,36.846334338376,-15.8853396943));
#52427=CARTESIAN_POINT('Ctrl Pts',(-4.49289136220764,36.8503336431165,-16.2694900363544));
#52428=CARTESIAN_POINT('Ctrl Pts',(-4.83852205833163,36.6657142912634,-15.7746228790373));
#52429=CARTESIAN_POINT('Ctrl Pts',(-4.46555605276301,36.6865436945369,-15.8890228148251));
#52430=CARTESIAN_POINT('Ctrl Pts',(-4.48649448972876,36.6921526528426,-16.2790801157266));
#52431=CARTESIAN_POINT('Ctrl Pts',(-4.83242355820479,36.5556302061425,-15.7764934506682));
#52432=CARTESIAN_POINT('Ctrl Pts',(-4.45560823761615,36.5806099310771,-15.8919151266673));
#52433=CARTESIAN_POINT('Ctrl Pts',(-4.48078239625453,36.5869847872263,-16.2859235908837));
#52434=CARTESIAN_POINT('Ctrl Pts',(-4.80964445731595,36.2263139098162,-15.7834588216173));
#52435=CARTESIAN_POINT('Ctrl Pts',(-4.42108305755237,36.2626839420804,-15.9018687747033));
#52436=CARTESIAN_POINT('Ctrl Pts',(-4.45944659885922,36.2723112115469,-16.3077427542653));
#52437=CARTESIAN_POINT('Ctrl Pts',(-4.78849025521988,36.0080156926272,-15.7899064986773));
#52438=CARTESIAN_POINT('Ctrl Pts',(-4.39194405386607,36.0530811161892,-15.9101712621084));
#52439=CARTESIAN_POINT('Ctrl Pts',(-4.43963274611102,36.0636336832212,-16.3240065044515));
#52440=CARTESIAN_POINT('Ctrl Pts',(-4.73479895287024,35.5737873220669,-15.806089492256));
#52441=CARTESIAN_POINT('Ctrl Pts',(-4.32221309888832,35.6372576288513,-15.9296899223679));
#52442=CARTESIAN_POINT('Ctrl Pts',(-4.38934337165934,35.6483850846731,-16.3596596636497));
#52443=CARTESIAN_POINT('Ctrl Pts',(-4.70226083470289,35.3578573765994,-15.8158250321208));
#52444=CARTESIAN_POINT('Ctrl Pts',(-4.28136065754713,35.4308416469974,-15.9409730418437));
#52445=CARTESIAN_POINT('Ctrl Pts',(-4.35886689759704,35.4418142023149,-16.3790492831481));
#52446=CARTESIAN_POINT('Ctrl Pts',(-4.62604323000226,34.9283028530584,-15.838285969081));
#52447=CARTESIAN_POINT('Ctrl Pts',(-4.18843254356921,35.0215742894843,-15.9661140402609));
#52448=CARTESIAN_POINT('Ctrl Pts',(-4.28747850736095,35.030732994809,-16.4206641704048));
#52449=CARTESIAN_POINT('Ctrl Pts',(-4.58236381820235,34.7146782724582,-15.851011583154));
#52450=CARTESIAN_POINT('Ctrl Pts',(-4.13606020425487,34.8185183918786,-15.9800423530578));
#52451=CARTESIAN_POINT('Ctrl Pts',(-4.24656666166447,34.8262226570115,-16.4428896521688));
#52452=CARTESIAN_POINT('Ctrl Pts',(-4.48381152977406,34.2897290978801,-15.8791706501668));
#52453=CARTESIAN_POINT('Ctrl Pts',(-4.02005922178393,34.4162818436401,-16.0101335970749));
#52454=CARTESIAN_POINT('Ctrl Pts',(-4.15425873313437,34.4192706098088,-16.489899151371));
#52455=CARTESIAN_POINT('Ctrl Pts',(-4.42893989399129,34.0784042783794,-15.8946043422336));
#52456=CARTESIAN_POINT('Ctrl Pts',(-3.95608545255841,34.2168878693719,-16.0263702668423));
#52457=CARTESIAN_POINT('Ctrl Pts',(-4.10286381244933,34.2168286739799,-16.5146834150258));
#52458=CARTESIAN_POINT('Ctrl Pts',(-4.30763827259879,33.6581098781651,-15.9279065885377));
#52459=CARTESIAN_POINT('Ctrl Pts',(-3.81658438476888,33.822448010845,-16.0607242667002));
#52460=CARTESIAN_POINT('Ctrl Pts',(-3.9892479689298,33.814078955275,-16.5665395015097));
#52461=CARTESIAN_POINT('Ctrl Pts',(-4.24121110891681,33.4491397713452,-15.9457754442683));
#52462=CARTESIAN_POINT('Ctrl Pts',(-3.7406469800499,33.6271818424222,-16.0789181512321));
#52463=CARTESIAN_POINT('Ctrl Pts',(-3.92702968859027,33.6137706563386,-16.593611645947));
#52464=CARTESIAN_POINT('Ctrl Pts',(-4.15956467569048,33.2154445308089,-15.9670945891216));
#52465=CARTESIAN_POINT('Ctrl Pts',(-3.64949552390511,33.4129433397945,-16.0999721147917));
#52466=CARTESIAN_POINT('Ctrl Pts',(-3.8505564455756,33.3896995093833,-16.6252009188576));
#52467=CARTESIAN_POINT('Ctrl Pts',(-4.15039805956273,33.189502508749,-15.9694798681321));
#52468=CARTESIAN_POINT('Ctrl Pts',(-3.63914933651993,33.3888967259962,-16.102351301209));
#52469=CARTESIAN_POINT('Ctrl Pts',(-3.84197063429969,33.3648249628758,-16.6287259546484));
#52470=CARTESIAN_POINT('Ctrl Pts',(-4.13189835567043,33.1377349934672,-15.9742764246118));
#52471=CARTESIAN_POINT('Ctrl Pts',(-3.61829077577786,33.3409526006064,-16.1071260478771));
#52472=CARTESIAN_POINT('Ctrl Pts',(-3.82464308795729,33.3151858843453,-16.635796298032));
#52473=CARTESIAN_POINT('Ctrl Pts',(-4.12256202229053,33.111900164225,-15.9766885508706));
#52474=CARTESIAN_POINT('Ctrl Pts',(-3.60777388976757,33.3170463264599,-16.1095225753306));
#52475=CARTESIAN_POINT('Ctrl Pts',(-3.81589831288601,33.2904124009369,-16.6393428649039));
#52476=CARTESIAN_POINT('Ctrl Pts',(-4.09429258351795,33.0345428662843,-15.9839653076811));
#52477=CARTESIAN_POINT('Ctrl Pts',(-3.57590653652943,33.2454014404084,-16.1167504752498));
#52478=CARTESIAN_POINT('Ctrl Pts',(-3.78942005068434,33.2162305590499,-16.6500155854832));
#52479=CARTESIAN_POINT('Ctrl Pts',(-4.07509908358835,32.9831675632239,-15.9888703159868));
#52480=CARTESIAN_POINT('Ctrl Pts',(-3.55434588845088,33.1979873053765,-16.1215955300393));
#52481=CARTESIAN_POINT('Ctrl Pts',(-3.77144266781143,33.1669607859179,-16.6571747604242));
#52482=CARTESIAN_POINT('Ctrl Pts',(-4.01646745258513,32.829634429189,-16.0037375413478));
#52483=CARTESIAN_POINT('Ctrl Pts',(-3.48838399516754,33.0560510137945,-16.1362734133368));
#52484=CARTESIAN_POINT('Ctrl Pts',(-3.71652598867197,33.0197101694359,-16.6787750251782));
#52485=CARTESIAN_POINT('Ctrl Pts',(-3.9759789438393,32.728068962807,-16.0138519706474));
#52486=CARTESIAN_POINT('Ctrl Pts',(-3.44313323859855,32.9628501297851,-16.1461489724732));
#52487=CARTESIAN_POINT('Ctrl Pts',(-3.67860286745824,32.9222876367011,-16.6933388861798));
#52488=CARTESIAN_POINT('Ctrl Pts',(-3.85020901317665,32.4257893774983,-16.0447294945566));
#52489=CARTESIAN_POINT('Ctrl Pts',(-3.30213588601185,32.6845768004043,-16.1762600178974));
#52490=CARTESIAN_POINT('Ctrl Pts',(-3.56080183062287,32.6323019776143,-16.7374460185429));
#52491=CARTESIAN_POINT('Ctrl Pts',(-3.76063777621999,32.2274841877532,-16.0660275892435));
#52492=CARTESIAN_POINT('Ctrl Pts',(-3.20289234856102,32.5050107524786,-16.1965656821621));
#52493=CARTESIAN_POINT('Ctrl Pts',(-3.47690590589959,32.4420132288924,-16.767405951522));
#52494=CARTESIAN_POINT('Ctrl Pts',(-3.56918607340305,31.8377243308601,-16.1096415154308));
#52495=CARTESIAN_POINT('Ctrl Pts',(-2.99311023840048,32.1562009537945,-16.2372785343144));
#52496=CARTESIAN_POINT('Ctrl Pts',(-3.29758475214954,32.0679272033942,-16.8280153427249));
#52497=CARTESIAN_POINT('Ctrl Pts',(-3.46731167512559,31.6462664711462,-16.1319583909726));
#52498=CARTESIAN_POINT('Ctrl Pts',(-2.88201843494523,31.9870356344035,-16.2577213825395));
#52499=CARTESIAN_POINT('Ctrl Pts',(-3.20216520503585,31.8841268311116,-16.8586659752245));
#52500=CARTESIAN_POINT('Ctrl Pts',(-3.24986431304015,31.2709079333655,-16.1771664307246));
#52501=CARTESIAN_POINT('Ctrl Pts',(-2.6480156494036,31.6607525771679,-16.2980633785119));
#52502=CARTESIAN_POINT('Ctrl Pts',(-2.99849550013316,31.5237128636391,-16.9201885252478));
#52503=CARTESIAN_POINT('Ctrl Pts',(-3.13430309790084,31.087001037092,-16.2000593106867));
#52504=CARTESIAN_POINT('Ctrl Pts',(-2.52446501017816,31.5038249498316,-16.3179747703128));
#52505=CARTESIAN_POINT('Ctrl Pts',(-2.89025634469189,31.3470932540427,-16.9510624162517));
#52506=CARTESIAN_POINT('Ctrl Pts',(-2.97992813214864,30.8625464320075,-16.2287095736517));
#52507=CARTESIAN_POINT('Ctrl Pts',(-2.36471133653988,31.3195585189969,-16.3416730253026));
#52508=CARTESIAN_POINT('Ctrl Pts',(-2.74566271341961,31.1314993826496,-16.9894416021804));
#52509=CARTESIAN_POINT('Ctrl Pts',(-2.94855445916935,30.817928300523,-16.2344410657162));
#52510=CARTESIAN_POINT('Ctrl Pts',(-2.33186814409271,31.2826216760433,-16.3464413005094));
#52511=CARTESIAN_POINT('Ctrl Pts',(-2.71627690378355,31.0886409312827,-16.9971064561535));
#52512=CARTESIAN_POINT('Ctrl Pts',(-2.88476410492296,30.7292614499473,-16.2458975182613));
#52513=CARTESIAN_POINT('Ctrl Pts',(-2.26536475661494,31.2097212908695,-16.3558796919869));
#52514=CARTESIAN_POINT('Ctrl Pts',(-2.65652836285939,31.0034678637871,-17.0124038567864));
#52515=CARTESIAN_POINT('Ctrl Pts',(-2.85231509096079,30.6851711096193,-16.2516279588096));
#52516=CARTESIAN_POINT('Ctrl Pts',(-2.23166075706606,31.1737321819387,-16.3605534424715));
#52517=CARTESIAN_POINT('Ctrl Pts',(-2.62613534683824,30.9611132622823,-17.0200436860762));
#52518=CARTESIAN_POINT('Ctrl Pts',(-2.75371586507387,30.5543032513299,-16.2687276605509));
#52519=CARTESIAN_POINT('Ctrl Pts',(-2.12916708502008,31.0671513308951,-16.3744245592637));
#52520=CARTESIAN_POINT('Ctrl Pts',(-2.53378345502449,30.8353931303199,-17.0428092866419));
#52521=CARTESIAN_POINT('Ctrl Pts',(-2.68624145339725,30.4688168020419,-16.280019596665));
#52522=CARTESIAN_POINT('Ctrl Pts',(-2.05994523352376,30.9990432166992,-16.3833298319653));
#52523=CARTESIAN_POINT('Ctrl Pts',(-2.47058428125334,30.7532636055963,-17.057800327605));
#52524=CARTESIAN_POINT('Ctrl Pts',(-2.54757388740944,30.3015880840125,-16.3022942711121));
#52525=CARTESIAN_POINT('Ctrl Pts',(-1.9192454319902,30.8681341748231,-16.4004596153518));
#52526=CARTESIAN_POINT('Ctrl Pts',(-2.34070281481905,30.5925930259895,-17.0873081301815));
#52527=CARTESIAN_POINT('Ctrl Pts',(-2.476381206771,30.2198453486412,-16.3132771209141));
#52528=CARTESIAN_POINT('Ctrl Pts',(-1.84771884517628,30.8054525230851,-16.4086687974615));
#52529=CARTESIAN_POINT('Ctrl Pts',(-2.27402096482143,30.5140515215888,-17.1018250250437));
#52530=CARTESIAN_POINT('Ctrl Pts',(-2.32998205788182,30.0603897553416,-16.334829595528));
#52531=CARTESIAN_POINT('Ctrl Pts',(-1.70258673578777,30.6857855527938,-16.4242870257666));
#52532=CARTESIAN_POINT('Ctrl Pts',(-2.13689779545945,30.3608345647763,-17.1302692409457));
#52533=CARTESIAN_POINT('Ctrl Pts',(-2.25477627281575,29.982676223402,-16.345399374049));
#52534=CARTESIAN_POINT('Ctrl Pts',(-1.62894510471729,30.6289401059803,-16.4316764817347));
#52535=CARTESIAN_POINT('Ctrl Pts',(-2.06645711480206,30.2861584632619,-17.1441967467396));
#52536=CARTESIAN_POINT('Ctrl Pts',(-2.09997874346892,29.831641210054,-16.3660070272072));
#52537=CARTESIAN_POINT('Ctrl Pts',(-1.47982485477628,30.5213540438189,-16.4455349971866));
#52538=CARTESIAN_POINT('Ctrl Pts',(-1.92146769383922,30.1410235804603,-17.1713290042148));
#52539=CARTESIAN_POINT('Ctrl Pts',(-2.02038800914664,29.7583187312675,-16.3760451220302));
#52540=CARTESIAN_POINT('Ctrl Pts',(-1.40432964804446,30.4707756283822,-16.4519799689631));
#52541=CARTESIAN_POINT('Ctrl Pts',(-1.84691989810708,30.0705638387238,-17.1845340213945));
#52542=CARTESIAN_POINT('Ctrl Pts',(-1.89735688368434,29.6519763755937,-16.3905992032782));
#52543=CARTESIAN_POINT('Ctrl Pts',(-1.29061421420031,30.4002010119293,-16.4608187862555));
#52544=CARTESIAN_POINT('Ctrl Pts',(-1.73168413361204,29.9683736297906,-17.2036812816511));
#52545=CARTESIAN_POINT('Ctrl Pts',(-1.855738117802,29.6171366953533,-16.3953665421613));
#52546=CARTESIAN_POINT('Ctrl Pts',(-1.25230151783671,30.3773864795662,-16.4636476099762));
#52547=CARTESIAN_POINT('Ctrl Pts',(-1.69270236914862,29.9348943080071,-17.2099534441512));
#52548=CARTESIAN_POINT('Ctrl Pts',(-1.79234339952953,29.5658416895116,-16.4023765699238));
#52549=CARTESIAN_POINT('Ctrl Pts',(-1.19475183342288,30.3445305772294,-16.4676726412067));
#52550=CARTESIAN_POINT('Ctrl Pts',(-1.63332439632481,29.8856025996842,-17.2191791942467));
#52551=CARTESIAN_POINT('Ctrl Pts',(-1.77105066057652,29.5489041771658,-16.4046897342604));
#52552=CARTESIAN_POINT('Ctrl Pts',(-1.17547199819176,30.333762872091,-16.4689831252204));
#52553=CARTESIAN_POINT('Ctrl Pts',(-1.6133807839376,29.8693266444902,-17.2222240118077));
#52554=CARTESIAN_POINT('Ctrl Pts',(-1.72813291087157,29.5153605402291,-16.409266356606));
#52555=CARTESIAN_POINT('Ctrl Pts',(-1.13683610528857,30.3126589001511,-16.4715332981359));
#52556=CARTESIAN_POINT('Ctrl Pts',(-1.57318234083472,29.8370933859026,-17.2282496978405));
#52557=CARTESIAN_POINT('Ctrl Pts',(-1.70649633572161,29.4987461608599,-16.4115309334004));
#52558=CARTESIAN_POINT('Ctrl Pts',(-1.11747086839056,30.3023210014394,-16.4727730500227));
#52559=CARTESIAN_POINT('Ctrl Pts',(-1.5529166780537,29.8211281512158,-17.231232043014));
#52560=CARTESIAN_POINT('Ctrl Pts',(-1.59782880094616,29.416805054283,-16.4226849288261));
#52561=CARTESIAN_POINT('Ctrl Pts',(-1.01994827144306,30.2514460679374,-16.4788242146341));
#52562=CARTESIAN_POINT('Ctrl Pts',(-1.45113441423997,29.7423892766781,-17.2459262700218));
#52563=CARTESIAN_POINT('Ctrl Pts',(-1.50908967345445,29.3546606084382,-16.4310964828382));
#52564=CARTESIAN_POINT('Ctrl Pts',(-0.94294827805055,30.2151476418465,-16.4829741135679));
#52565=CARTESIAN_POINT('Ctrl Pts',(-1.36801787580905,29.6826756493925,-17.2570235387147));
#52566=CARTESIAN_POINT('Ctrl Pts',(-1.32773854032885,29.2376739642212,-16.446744165317));
#52567=CARTESIAN_POINT('Ctrl Pts',(-0.789958819385205,30.1499851126795,
-16.4900488930594));
#52568=CARTESIAN_POINT('Ctrl Pts',(-1.19815731065464,29.570273767709,-17.2777301553418));
#52569=CARTESIAN_POINT('Ctrl Pts',(-1.23512712642901,29.1828306555037,-16.4539805128856));
#52570=CARTESIAN_POINT('Ctrl Pts',(-0.714148771847181,30.1213547087018,
-16.4929390217047));
#52571=CARTESIAN_POINT('Ctrl Pts',(-1.11141383725493,29.5175844450748,-17.2873397728772));
#52572=CARTESIAN_POINT('Ctrl Pts',(-1.04569979909049,29.0810615938186,-16.4671043497951));
#52573=CARTESIAN_POINT('Ctrl Pts',(-0.564018986317464,30.0710934810012,
-16.4975516672181));
#52574=CARTESIAN_POINT('Ctrl Pts',(-0.933988792708237,29.4198266340564,
-17.3048725518148));
#52575=CARTESIAN_POINT('Ctrl Pts',(-0.948884762668731,29.0341341932451,
-16.4729921490482));
#52576=CARTESIAN_POINT('Ctrl Pts',(-0.489933276919771,30.0496744036365,
-16.4992439979384));
#52577=CARTESIAN_POINT('Ctrl Pts',(-0.843308041987629,29.3747565609294,
-17.3127960973893));
#52578=CARTESIAN_POINT('Ctrl Pts',(-0.800191680576077,28.9702716007703,
-16.4806600727396));
#52579=CARTESIAN_POINT('Ctrl Pts',(-0.380586307990408,30.0223765474346,
-16.5009885630312));
#52580=CARTESIAN_POINT('Ctrl Pts',(-0.704036284927813,29.3134377089103,
-17.3232401222866));
#52581=CARTESIAN_POINT('Ctrl Pts',(-0.750048107089607,28.9500736446709,
-16.483021826383));
#52582=CARTESIAN_POINT('Ctrl Pts',(-0.344229360090164,30.014052241189,-16.5014375482369));
#52583=CARTESIAN_POINT('Ctrl Pts',(-0.657069852279363,29.2940472367443,
-17.3264809285521));
#52584=CARTESIAN_POINT('Ctrl Pts',(-0.673915805988587,28.9215008203245,
-16.486251322221));
#52585=CARTESIAN_POINT('Ctrl Pts',(-0.290130099099646,30.0026923249378,
-16.501926978582));
#52586=CARTESIAN_POINT('Ctrl Pts',(-0.585761361026588,29.2666219330869,
-17.3309558082814));
#52587=CARTESIAN_POINT('Ctrl Pts',(-0.648385485598382,28.91226401611,-16.4872756105357));
#52588=CARTESIAN_POINT('Ctrl Pts',(-0.272119298069543,29.9990851554066,
-16.5020595144662));
#52589=CARTESIAN_POINT('Ctrl Pts',(-0.561848664151634,29.2577570144913,
-17.3323830214636));
#52590=CARTESIAN_POINT('Ctrl Pts',(-0.597010216853532,28.8943818767733,
-16.4892158575437));
#52591=CARTESIAN_POINT('Ctrl Pts',(-0.2362023844278,29.9922245088925,-16.5022661141874));
#52592=CARTESIAN_POINT('Ctrl Pts',(-0.513728577814346,29.2405968337917,
-17.3351040222603));
#52593=CARTESIAN_POINT('Ctrl Pts',(-0.571233147511417,28.8857606891544,
-16.4901291611817));
#52594=CARTESIAN_POINT('Ctrl Pts',(-0.218349366931985,29.9889826962993,
-16.5023396092702));
#52595=CARTESIAN_POINT('Ctrl Pts',(-0.4895847662591,29.2323247467198,-17.3363941024547));
#52596=CARTESIAN_POINT('Ctrl Pts',(-0.442166073327688,28.8443554178395,
-16.4943979018314));
#52597=CARTESIAN_POINT('Ctrl Pts',(-0.129239837306087,29.9735906916381,
-16.5025703106399));
#52598=CARTESIAN_POINT('Ctrl Pts',(-0.368695495698975,29.1926016196164,
-17.342474342916));
#52599=CARTESIAN_POINT('Ctrl Pts',(-0.338061778022354,28.8165747708187,
-16.4968705077674));
#52600=CARTESIAN_POINT('Ctrl Pts',(-0.0605317814243137,29.9642648979254,
-16.5023091130787));
#52601=CARTESIAN_POINT('Ctrl Pts',(-0.271187340267436,29.1659679325416,
-17.3461688365462));
#52602=CARTESIAN_POINT('Ctrl Pts',(-0.128108295013126,28.7719728676628,
-16.499836683451));
#52603=CARTESIAN_POINT('Ctrl Pts',(0.074456716006171,29.94974338385,-16.5011651314723));
#52604=CARTESIAN_POINT('Ctrl Pts',(-0.0745366950826016,29.1232544765027,
-17.3511133431508));
#52605=CARTESIAN_POINT('Ctrl Pts',(-0.0222591829595038,28.755151135902,
-16.5003303276454));
#52606=CARTESIAN_POINT('Ctrl Pts',(0.140356992327616,29.9446203245694,-16.5002807332538));
#52607=CARTESIAN_POINT('Ctrl Pts',(0.0246057239760995,29.1071742509764,
-17.3523634528138));
#52608=CARTESIAN_POINT('Ctrl Pts',(0.191245793985154,28.7328543901453,-16.499236995659));
#52609=CARTESIAN_POINT('Ctrl Pts',(0.27161304708856,29.937520037568,-16.4980385051));
#52610=CARTESIAN_POINT('Ctrl Pts',(0.224582837315142,29.0859421960738,-17.3523016800784));
#52611=CARTESIAN_POINT('Ctrl Pts',(0.298901540034271,28.7273786281084,-16.4976501104633));
#52612=CARTESIAN_POINT('Ctrl Pts',(0.336593949719366,29.9355704487499,-16.496686377349));
#52613=CARTESIAN_POINT('Ctrl Pts',(0.325417420428351,29.080789649795,-17.3509899235518));
#52614=CARTESIAN_POINT('Ctrl Pts',(0.434652344247154,28.7279511908531,-16.4942964360642));
#52615=CARTESIAN_POINT('Ctrl Pts',(0.41904432966663,29.9349828888683,-16.4946901599378));
#52616=CARTESIAN_POINT('Ctrl Pts',(0.452566934002955,29.0814932456998,-17.3476656555962));
#52617=CARTESIAN_POINT('Ctrl Pts',(0.461791435185215,28.7284371115372,-16.4935588164354));
#52618=CARTESIAN_POINT('Ctrl Pts',(0.435530517342106,29.9349612139799,-16.4942766579394));
#52619=CARTESIAN_POINT('Ctrl Pts',(0.477986468216754,29.0819916232635,-17.3469181407489));
#52620=CARTESIAN_POINT('Ctrl Pts',(0.515943690984539,28.7301437164452,-16.4919536704588));
#52621=CARTESIAN_POINT('Ctrl Pts',(0.468495969700064,29.9351121018813,-16.4934206136822));
#52622=CARTESIAN_POINT('Ctrl Pts',(0.528707589352712,29.0836958274767,-17.3452619533545));
#52623=CARTESIAN_POINT('Ctrl Pts',(0.542973446398712,28.7313644483332,-16.4910857384778));
#52624=CARTESIAN_POINT('Ctrl Pts',(0.484979151558676,29.9352844403668,-16.4929780058774));
#52625=CARTESIAN_POINT('Ctrl Pts',(0.554024715635541,29.084901718379,-17.344352879355));
#52626=CARTESIAN_POINT('Ctrl Pts',(0.623924958202809,28.7361181266015,-16.4882877715005));
#52627=CARTESIAN_POINT('Ctrl Pts',(0.534479466208411,29.9361010848821,-16.4916034160629));
#52628=CARTESIAN_POINT('Ctrl Pts',(0.629847068288364,29.0895703548083,-17.3413850837553));
#52629=CARTESIAN_POINT('Ctrl Pts',(0.677708990090665,28.7407423067484,-16.4861635783227));
#52630=CARTESIAN_POINT('Ctrl Pts',(0.567561890649228,29.9370419497641,-16.490624834322));
#52631=CARTESIAN_POINT('Ctrl Pts',(0.680223296507896,29.0940838248501,-17.339085810858));
#52632=CARTESIAN_POINT('Ctrl Pts',(0.838519927256103,28.7589030127749,-16.4790291084593));
#52633=CARTESIAN_POINT('Ctrl Pts',(0.667392543733618,29.9411882626693,-16.4874678461666));
#52634=CARTESIAN_POINT('Ctrl Pts',(0.830845110920096,29.1117531657169,-17.3312437799614));
#52635=CARTESIAN_POINT('Ctrl Pts',(0.945006106505387,28.7767241011346,-16.4732571040723));
#52636=CARTESIAN_POINT('Ctrl Pts',(0.734797573094118,29.9456748746285,-16.4850736283494));
#52637=CARTESIAN_POINT('Ctrl Pts',(0.930584232001352,29.1290345185376,-17.3247571305769));
#52638=CARTESIAN_POINT('Ctrl Pts',(1.07723807457993,28.8059438373021,-16.4648188690481));
#52639=CARTESIAN_POINT('Ctrl Pts',(0.821934628374837,29.9543140629695,-16.481507158621));
#52640=CARTESIAN_POINT('Ctrl Pts',(1.05443786599453,29.1573212640841,-17.315130200981));
#52641=CARTESIAN_POINT('Ctrl Pts',(1.10366391397319,28.8121410610613,-16.4630684410996));
#52642=CARTESIAN_POINT('Ctrl Pts',(0.839404777360703,29.9561838764168,-16.4807692180936));
#52643=CARTESIAN_POINT('Ctrl Pts',(1.07918934093606,29.1633187716124,-17.3131270133982));
#52644=CARTESIAN_POINT('Ctrl Pts',(1.15632374754114,28.8252003709767,-16.4594535730141));
#52645=CARTESIAN_POINT('Ctrl Pts',(0.874521011859752,29.9602382847319,-16.4792360955938));
#52646=CARTESIAN_POINT('Ctrl Pts',(1.12851260097818,29.1759537682257,-17.3089782907615));
#52647=CARTESIAN_POINT('Ctrl Pts',(1.18250126727682,28.8320477321608,-16.4575931395356));
#52648=CARTESIAN_POINT('Ctrl Pts',(0.892123466946685,29.9624166282505,-16.4784430213444));
#52649=CARTESIAN_POINT('Ctrl Pts',(1.15303149003764,29.1825770131165,-17.3068373640129));
#52650=CARTESIAN_POINT('Ctrl Pts',(1.26059001577615,28.8535152040682,-16.4518581803553));
#52651=CARTESIAN_POINT('Ctrl Pts',(0.945006269189896,29.9694228223987,-16.4759818429639));
#52652=CARTESIAN_POINT('Ctrl Pts',(1.22617246651459,29.2033372707004,-17.3002214041692));
#52653=CARTESIAN_POINT('Ctrl Pts',(1.31205768956044,28.8690601669617,-16.4478300726312));
#52654=CARTESIAN_POINT('Ctrl Pts',(0.980523921137524,29.974736003371,-16.4742254675058));
#52655=CARTESIAN_POINT('Ctrl Pts',(1.27437910322739,29.2183642879055,-17.2955532864967));
#52656=CARTESIAN_POINT('Ctrl Pts',(1.4647831287284,28.9191944472757,-16.43517107612));
#52657=CARTESIAN_POINT('Ctrl Pts',(1.08747216242771,29.9927517710206,-16.4685881506749));
#52658=CARTESIAN_POINT('Ctrl Pts',(1.41742772376219,29.2668125837537,-17.2808247001297));
#52659=CARTESIAN_POINT('Ctrl Pts',(1.56436648530266,28.957276499474,-16.4259664459877));
#52660=CARTESIAN_POINT('Ctrl Pts',(1.15996351383399,30.0075731994565,-16.4643154615969));
#52661=CARTESIAN_POINT('Ctrl Pts',(1.51070139131698,29.3035947033487,-17.2700412085024));
#52662=CARTESIAN_POINT('Ctrl Pts',(1.75949339397493,29.0418768304825,-16.4062122131103));
#52663=CARTESIAN_POINT('Ctrl Pts',(1.30740732628336,30.0440019520787,-16.4545229469892));
#52664=CARTESIAN_POINT('Ctrl Pts',(1.69346488679426,29.385274695068,-17.246768023877));
#52665=CARTESIAN_POINT('Ctrl Pts',(1.85503603822308,29.0883970101933,-16.3956623294501));
#52666=CARTESIAN_POINT('Ctrl Pts',(1.38208746912005,30.0654311191767,-16.449040555324));
#52667=CARTESIAN_POINT('Ctrl Pts',(1.78295386512358,29.4301743920079,-17.2342779633839));
#52668=CARTESIAN_POINT('Ctrl Pts',(2.04241537792939,29.1891877116256,-16.3733759911771));
#52669=CARTESIAN_POINT('Ctrl Pts',(1.53349668675425,30.1157894070632,-16.4367176133733));
#52670=CARTESIAN_POINT('Ctrl Pts',(1.95846068444071,29.5274274114621,-17.2077786001255));
#52671=CARTESIAN_POINT('Ctrl Pts',(2.13425146341608,29.2434595083696,-16.3616393385331));
#52672=CARTESIAN_POINT('Ctrl Pts',(1.61000429268926,30.1445060379138,-16.4299192937042));
#52673=CARTESIAN_POINT('Ctrl Pts',(2.04447795482465,29.5797819581103,-17.1937690407036));
#52674=CARTESIAN_POINT('Ctrl Pts',(2.3144828178405,29.3592119103105,-16.3371184864176));
#52675=CARTESIAN_POINT('Ctrl Pts',(1.76445361782877,30.2098541291851,-16.4149279831066));
#52676=CARTESIAN_POINT('Ctrl Pts',(2.21328969153138,29.6914212472574,-17.1643920201756));
#52677=CARTESIAN_POINT('Ctrl Pts',(2.40287766710257,29.4206933906018,-16.3243341414413));
#52678=CARTESIAN_POINT('Ctrl Pts',(1.84222493333582,30.2462536617642,-16.4067789597616));
#52679=CARTESIAN_POINT('Ctrl Pts',(2.29608376542315,29.7507068302044,-17.1490243729861));
#52680=CARTESIAN_POINT('Ctrl Pts',(2.51135285252538,29.5017829309144,-16.3077769328132));
#52681=CARTESIAN_POINT('Ctrl Pts',(1.94077379223057,30.2972459914495,-16.3956391132683));
#52682=CARTESIAN_POINT('Ctrl Pts',(2.39768586735591,29.8288858890433,-17.1290549495678));
#52683=CARTESIAN_POINT('Ctrl Pts',(2.53290170127805,29.5181794566019,-16.3044434790811));
#52684=CARTESIAN_POINT('Ctrl Pts',(1.96028897303141,30.3075771594425,-16.3933941774779));
#52685=CARTESIAN_POINT('Ctrl Pts',(2.41786936214229,29.8446932300906,-17.1250312972996));
#52686=CARTESIAN_POINT('Ctrl Pts',(2.57565545767622,29.5512731693992,-16.2977442351459));
#52687=CARTESIAN_POINT('Ctrl Pts',(1.99921568638862,30.3286552806381,-16.3888383057235));
#52688=CARTESIAN_POINT('Ctrl Pts',(2.45791420271846,29.8765964221614,-17.1169385254278));
#52689=CARTESIAN_POINT('Ctrl Pts',(2.59687024481893,29.5679777347785,-16.2943769383145));
#52690=CARTESIAN_POINT('Ctrl Pts',(2.01863572271277,30.3394038774272,-16.3865268648834));
#52691=CARTESIAN_POINT('Ctrl Pts',(2.47778480237176,29.8926993859692,-17.1128675875488));
#52692=CARTESIAN_POINT('Ctrl Pts',(2.66004324798223,29.6185503436459,-16.2842251711301));
#52693=CARTESIAN_POINT('Ctrl Pts',(2.07658934638655,30.3721820016165,-16.3795138210175));
#52694=CARTESIAN_POINT('Ctrl Pts',(2.53695510817887,29.9414486673533,-17.100584863834));
#52695=CARTESIAN_POINT('Ctrl Pts',(2.70153038913429,29.6528770266069,-16.2773908679428));
#52696=CARTESIAN_POINT('Ctrl Pts',(2.11515348080612,30.3949183678539,-16.3746953336256));
#52697=CARTESIAN_POINT('Ctrl Pts',(2.57581358773611,29.9745351098867,-17.0923032197876));
#52698=CARTESIAN_POINT('Ctrl Pts',(2.82421530443451,29.7575890425693,-16.2567120771395));
#52699=CARTESIAN_POINT('Ctrl Pts',(2.22956819594977,30.4651684504852,-16.3599495397914));
#52700=CARTESIAN_POINT('Ctrl Pts',(2.69072507829928,30.0754559176024,-17.0672065911949));
#52701=CARTESIAN_POINT('Ctrl Pts',(2.90364008546083,29.8297029496513,-16.2426922301433));
#52702=CARTESIAN_POINT('Ctrl Pts',(2.30547175408465,30.5154143020214,-16.3495803497904));
#52703=CARTESIAN_POINT('Ctrl Pts',(2.7651174356246,30.1449484959329,-17.0501405710026));
#52704=CARTESIAN_POINT('Ctrl Pts',(3.05823671500216,29.9780894969754,-16.2142950763844));
#52705=CARTESIAN_POINT('Ctrl Pts',(2.45531918886263,30.6220505261989,-16.3279618812435));
#52706=CARTESIAN_POINT('Ctrl Pts',(2.90991868602117,30.2879200951006,-17.0154679498268));
#52707=CARTESIAN_POINT('Ctrl Pts',(3.13340755103014,30.0543631118974,-16.1999176059517));
#52708=CARTESIAN_POINT('Ctrl Pts',(2.52928950864992,30.6782919897607,-16.316734700869));
#52709=CARTESIAN_POINT('Ctrl Pts',(2.98032663199793,30.3614000520084,-16.9978611399441));
#52710=CARTESIAN_POINT('Ctrl Pts',(3.27987015132021,30.210715992756,-16.1709005658607));
#52711=CARTESIAN_POINT('Ctrl Pts',(2.67504196758113,30.7964541736505,-16.2935360824409));
#52712=CARTESIAN_POINT('Ctrl Pts',(3.11750923246245,30.5120049089877,-16.9622167722053));
#52713=CARTESIAN_POINT('Ctrl Pts',(3.35116123035258,30.2907959175364,-16.156260881267));
#52714=CARTESIAN_POINT('Ctrl Pts',(2.74686657696321,30.8582478680463,-16.2815815826731));
#52715=CARTESIAN_POINT('Ctrl Pts',(3.18428324621236,30.5891304417996,-16.9441790683909));
#52716=CARTESIAN_POINT('Ctrl Pts',(3.55966298596679,30.5363244595009,-16.1120758578107));
#52717=CARTESIAN_POINT('Ctrl Pts',(2.95660210195659,31.049475646984,-16.2451814165979));
#52718=CARTESIAN_POINT('Ctrl Pts',(3.37957414633138,30.8255678671554,-16.8895639888451));
#52719=CARTESIAN_POINT('Ctrl Pts',(3.69152422416695,30.7070404100115,-16.0822670185369));
#52720=CARTESIAN_POINT('Ctrl Pts',(3.0935680110286,31.188233012752,-16.2194870411642));
#52721=CARTESIAN_POINT('Ctrl Pts',(3.50308054074258,30.9899200073615,-16.8524880403649));
#52722=CARTESIAN_POINT('Ctrl Pts',(3.84850625888578,30.9282217390845,-16.0449381752436));
#52723=CARTESIAN_POINT('Ctrl Pts',(3.2607646882954,31.3759330382798,-16.1859089389379));
#52724=CARTESIAN_POINT('Ctrl Pts',(3.6501160551046,31.2027958226833,-16.8057225066586));
#52725=CARTESIAN_POINT('Ctrl Pts',(3.87953256866694,30.9728856431268,-16.0374628392411));
#52726=CARTESIAN_POINT('Ctrl Pts',(3.29342662187892,31.4134934654484,-16.1792418772485));
#52727=CARTESIAN_POINT('Ctrl Pts',(3.67917651069663,31.2457796337213,-16.7963405521398));
#52728=CARTESIAN_POINT('Ctrl Pts',(3.94058434545197,31.0626285007038,-16.022571026142));
#52729=CARTESIAN_POINT('Ctrl Pts',(3.35787539127852,31.4893981914476,-16.1658790869078));
#52730=CARTESIAN_POINT('Ctrl Pts',(3.73635999288582,31.3321406834297,-16.7776156643026));
#52731=CARTESIAN_POINT('Ctrl Pts',(3.97063463723664,31.1077409109996,-16.0151487999533));
#52732=CARTESIAN_POINT('Ctrl Pts',(3.38969847622929,31.5277649299416,-16.1591781972395));
#52733=CARTESIAN_POINT('Ctrl Pts',(3.76450627188365,31.3755501268062,-16.7682655550614));
#52734=CARTESIAN_POINT('Ctrl Pts',(4.05941717087094,31.2437732562028,-15.9929626480247));
#52735=CARTESIAN_POINT('Ctrl Pts',(3.48351050644036,31.6435098716445,-16.1391308660064));
#52736=CARTESIAN_POINT('Ctrl Pts',(3.84766346564603,31.5064382047407,-16.7402628285028));
#52737=CARTESIAN_POINT('Ctrl Pts',(4.1167828254897,31.3353874419429,-15.978279338896));
#52738=CARTESIAN_POINT('Ctrl Pts',(3.54479499845881,31.7226089412723,-16.1256471238317));
#52739=CARTESIAN_POINT('Ctrl Pts',(3.90139438215665,31.5945757570875,-16.7216579368768));
#52740=CARTESIAN_POINT('Ctrl Pts',(4.28380788594745,31.6128203257638,-15.9346238064299));
#52741=CARTESIAN_POINT('Ctrl Pts',(3.72231473431664,31.9620905398297,-16.0855354656462));
#52742=CARTESIAN_POINT('Ctrl Pts',(4.05783658707824,31.8614425296594,-16.6661133987202));
#52743=CARTESIAN_POINT('Ctrl Pts',(4.3884148581878,31.8012197189447,-15.9060466319014));
#52744=CARTESIAN_POINT('Ctrl Pts',(3.83587999076983,32.1288604724229,-16.0584933410282));
#52745=CARTESIAN_POINT('Ctrl Pts',(4.15581556986088,32.0426166386068,-16.6294449643945));
#52746=CARTESIAN_POINT('Ctrl Pts',(4.58567200756637,32.1841943988468,-15.8503033618542));
#52747=CARTESIAN_POINT('Ctrl Pts',(4.05086579113235,32.4720636118671,-16.0050120263636));
#52748=CARTESIAN_POINT('Ctrl Pts',(4.34057433194744,32.4107939451974,-16.5572151315481));
#52749=CARTESIAN_POINT('Ctrl Pts',(4.67831544203237,32.3787729501169,-15.8231365471297));
#52750=CARTESIAN_POINT('Ctrl Pts',(4.152839616667,32.6484592325927,-15.9785118187779));
#52751=CARTESIAN_POINT('Ctrl Pts',(4.4273477970609,32.5978002916929,-16.5216528747722));
#52752=CARTESIAN_POINT('Ctrl Pts',(4.8526074647995,32.7736749069825,-15.7705575791359));
#52753=CARTESIAN_POINT('Ctrl Pts',(4.34531777018242,33.0096063680591,-15.9266467671527));
#52754=CARTESIAN_POINT('Ctrl Pts',(4.59059652338769,32.9772145356856,-16.4519928922655));
#52755=CARTESIAN_POINT('Ctrl Pts',(4.93425250225085,32.9740000075212,-15.7451448786754));
#52756=CARTESIAN_POINT('Ctrl Pts',(4.43629332140126,33.1943793675723,-15.9012113154715));
#52757=CARTESIAN_POINT('Ctrl Pts',(4.66706845943702,33.1696240761953,-16.4178945495574));
#52758=CARTESIAN_POINT('Ctrl Pts',(5.08711281849313,33.3801631316144,-15.6964237384943));
#52759=CARTESIAN_POINT('Ctrl Pts',(4.60722078767624,33.5714101157215,-15.8519572579756));
#52760=CARTESIAN_POINT('Ctrl Pts',(4.81024341123228,33.5596069464454,-16.3515167576984));
#52761=CARTESIAN_POINT('Ctrl Pts',(5.15832642133817,33.5860019204558,-15.6731147994769));
#52762=CARTESIAN_POINT('Ctrl Pts',(4.68757869339825,33.7637237962017,-15.8280627301349));
#52763=CARTESIAN_POINT('Ctrl Pts',(4.87694485739314,33.7571810298932,-16.3192367814774));
#52764=CARTESIAN_POINT('Ctrl Pts',(5.24097629968965,33.8467036990582,-15.6455255940079));
#52765=CARTESIAN_POINT('Ctrl Pts',(4.78213072770676,34.0107071083605,-15.7992314731343));
#52766=CARTESIAN_POINT('Ctrl Pts',(4.95435796666611,34.0073247840893,-16.2802535152582));
#52767=CARTESIAN_POINT('Ctrl Pts',(5.25719362818707,33.8990359684241,-15.6400829974654));
#52768=CARTESIAN_POINT('Ctrl Pts',(4.80054957120818,34.0598870173825,-15.793578275618));
#52769=CARTESIAN_POINT('Ctrl Pts',(4.96954775094229,34.0575332013725,-16.2725221393888));
#52770=CARTESIAN_POINT('Ctrl Pts',(5.28896226944923,34.0039467757404,-15.6293684812982));
#52771=CARTESIAN_POINT('Ctrl Pts',(4.83669604861666,34.1585897884646,-15.7824156043202));
#52772=CARTESIAN_POINT('Ctrl Pts',(4.99930350304212,34.1581771173989,-16.2572160497018));
#52773=CARTESIAN_POINT('Ctrl Pts',(5.30449626492683,34.0564670383293,-15.624102431784));
#52774=CARTESIAN_POINT('Ctrl Pts',(4.85440974566674,34.2080603224636,-15.7769108872987));
#52775=CARTESIAN_POINT('Ctrl Pts',(5.0138532509136,34.208556714705,-16.2496497575703));
#52776=CARTESIAN_POINT('Ctrl Pts',(5.3500593030389,34.2142207349753,-15.6085840212356));
#52777=CARTESIAN_POINT('Ctrl Pts',(4.90631386646526,34.3563731632076,-15.7606865923713));
#52778=CARTESIAN_POINT('Ctrl Pts',(5.05652937471128,34.3598665463188,-16.2272172272366));
#52779=CARTESIAN_POINT('Ctrl Pts',(5.37905002720047,34.3196469683343,-15.598611350614));
#52780=CARTESIAN_POINT('Ctrl Pts',(4.9396069834735,34.4560073796611,-15.7501529654412));
#52781=CARTESIAN_POINT('Ctrl Pts',(5.08368322108408,34.460967717809,-16.2126172924642));
#52782=CARTESIAN_POINT('Ctrl Pts',(5.46194078461707,34.6366877503115,-15.569862681342));
#52783=CARTESIAN_POINT('Ctrl Pts',(5.03466043352864,34.7544911380799,-15.7197631997284));
#52784=CARTESIAN_POINT('Ctrl Pts',(5.16132194699471,34.7649439115857,-16.1699328633975));
#52785=CARTESIAN_POINT('Ctrl Pts',(5.51176846617966,34.8490627904254,-15.5522551143952));
#52786=CARTESIAN_POINT('Ctrl Pts',(5.09291260313501,34.9564096240105,-15.7007118502892));
#52787=CARTESIAN_POINT('Ctrl Pts',(5.2079925027011,34.968490137579,-16.1429629194519));
#52788=CARTESIAN_POINT('Ctrl Pts',(5.60071361456991,35.275833071767,-15.5204457982229));
#52789=CARTESIAN_POINT('Ctrl Pts',(5.19800485837501,35.3631027727456,-15.6657772117967));
#52790=CARTESIAN_POINT('Ctrl Pts',(5.29130200819381,35.3773514622423,-16.0922807281473));
#52791=CARTESIAN_POINT('Ctrl Pts',(5.63983069135891,35.4902283652519,-15.5062438204224));
#52792=CARTESIAN_POINT('Ctrl Pts',(5.24514293116004,35.5680932299173,-15.649807466499));
#52793=CARTESIAN_POINT('Ctrl Pts',(5.32794059231136,35.5826666215459,-16.0685682530086));
#52794=CARTESIAN_POINT('Ctrl Pts',(5.70722219029865,35.9210809846202,-15.4815665394735));
#52795=CARTESIAN_POINT('Ctrl Pts',(5.32796042195972,35.9807456339375,-15.6213886714218));
#52796=CARTESIAN_POINT('Ctrl Pts',(5.39106210676183,35.9950907162295,-16.0247146511509));
#52797=CARTESIAN_POINT('Ctrl Pts',(5.73549725525296,36.1375381840345,-15.4710909455289));
#52798=CARTESIAN_POINT('Ctrl Pts',(5.36389926796403,36.1886130621991,-15.6088583771076));
#52799=CARTESIAN_POINT('Ctrl Pts',(5.41754563828522,36.2021995446388,-16.004573243818));
#52800=CARTESIAN_POINT('Ctrl Pts',(5.78078346060784,36.5726077638088,-15.4542268131215));
#52801=CARTESIAN_POINT('Ctrl Pts',(5.42398393004534,36.606935192749,-15.5876972584938));
#52802=CARTESIAN_POINT('Ctrl Pts',(5.45996247023453,36.6182830146743,-15.9682119674733));
#52803=CARTESIAN_POINT('Ctrl Pts',(5.7977963957715,36.7912198164816,-15.4478378834369));
#52804=CARTESIAN_POINT('Ctrl Pts',(5.44836047329696,36.8175859984048,-15.5789899469686));
#52805=CARTESIAN_POINT('Ctrl Pts',(5.47589745022953,36.8272573619824,-15.9519917284049));
#52806=CARTESIAN_POINT('Ctrl Pts',(5.81430843554853,37.1208676336436,-15.4416272457358));
#52807=CARTESIAN_POINT('Ctrl Pts',(5.47569053932407,37.1367087944884,-15.5691295274642));
#52808=CARTESIAN_POINT('Ctrl Pts',(5.49136327314324,37.1422120437367,-15.9308997542));
#52809=CARTESIAN_POINT('Ctrl Pts',(5.81830852011158,37.2310390122662,-15.4401195822918));
#52810=CARTESIAN_POINT('Ctrl Pts',(5.48324669152352,37.243039155561,-15.5663815273683));
#52811=CARTESIAN_POINT('Ctrl Pts',(5.49510990843326,37.2474462392647,-15.924409220868));
#52812=CARTESIAN_POINT('Ctrl Pts',(5.8219552680468,37.3967483415922,-15.4387447204924));
#52813=CARTESIAN_POINT('Ctrl Pts',(5.49218973652234,37.4033363287178,-15.5630995045285));
#52814=CARTESIAN_POINT('Ctrl Pts',(5.49852559552139,37.4056877138083,-15.9155248418178));
#52815=CARTESIAN_POINT('Ctrl Pts',(5.82277787197035,37.4520779924035,-15.4384344431652));
#52816=CARTESIAN_POINT('Ctrl Pts',(5.49476863526362,37.4567795900761,-15.5621468243714));
#52817=CARTESIAN_POINT('Ctrl Pts',(5.49929607838327,37.4585169113888,-15.9127047089119));
#52818=CARTESIAN_POINT('Ctrl Pts',(5.82361937406439,37.5625395576871,-15.438117035061));
#52819=CARTESIAN_POINT('Ctrl Pts',(5.49909810504416,37.5635003468084,-15.5605340956755));
#52820=CARTESIAN_POINT('Ctrl Pts',(5.50008426225533,37.5639723612738,-15.9073715669842));
#52821=CARTESIAN_POINT('Ctrl Pts',(5.82363950904436,37.6177133458351,-15.438109438589));
#52822=CARTESIAN_POINT('Ctrl Pts',(5.5008542982352,37.6168225419558,-15.5598720284282));
#52823=CARTESIAN_POINT('Ctrl Pts',(5.50010312136638,37.6166386057181,-15.9048561966123));
#52824=CARTESIAN_POINT('Ctrl Pts',(5.8217154307924,37.893294229626,-15.4388351940587));
#52825=CARTESIAN_POINT('Ctrl Pts',(5.50752491944064,37.881853217054,-15.5573104201885));
#52826=CARTESIAN_POINT('Ctrl Pts',(5.49830095467151,37.8796590971548,-15.8930435523112));
#52827=CARTESIAN_POINT('Ctrl Pts',(5.8137104043734,38.1128388502149,-15.4418594419708));
#52828=CARTESIAN_POINT('Ctrl Pts',(5.50636898532151,38.0944392377558,-15.5575651542258));
#52829=CARTESIAN_POINT('Ctrl Pts',(5.49080313325399,38.0890827853353,-15.886038511744));
#52830=CARTESIAN_POINT('Ctrl Pts',(5.7840049154644,38.5499825598019,-15.4530106720142));
#52831=CARTESIAN_POINT('Ctrl Pts',(5.48999166329811,38.5177567680441,-15.5630532663817));
#52832=CARTESIAN_POINT('Ctrl Pts',(5.46297981094671,38.5058340924418,-15.8771352552735));
#52833=CARTESIAN_POINT('Ctrl Pts',(5.76230703860224,38.7675819658764,-15.4611377904124));
#52834=CARTESIAN_POINT('Ctrl Pts',(5.47493356768806,38.7287614510696,-15.568229955048));
#52835=CARTESIAN_POINT('Ctrl Pts',(5.44265672992744,38.7131620074787,-15.8752371590965));
#52836=CARTESIAN_POINT('Ctrl Pts',(5.70407395336722,39.2006823460781,-15.4827163158072));
#52837=CARTESIAN_POINT('Ctrl Pts',(5.42972855746396,39.1486876692357,-15.5837780636752));
#52838=CARTESIAN_POINT('Ctrl Pts',(5.38811334519547,39.1255654423464,-15.8767726336669));
#52839=CARTESIAN_POINT('Ctrl Pts',(5.66754335828454,39.4161838894492,-15.4961678890182));
#52840=CARTESIAN_POINT('Ctrl Pts',(5.39972357971351,39.3578660216,-15.5941025574047));
#52841=CARTESIAN_POINT('Ctrl Pts',(5.35389735978674,39.3306414973316,-15.88020634219));
#52842=CARTESIAN_POINT('Ctrl Pts',(5.60039918974671,39.7377021629651,-15.5205056507883));
#52843=CARTESIAN_POINT('Ctrl Pts',(5.34213771584874,39.6706104721975,-15.6136918367253));
#52844=CARTESIAN_POINT('Ctrl Pts',(5.29100750584286,39.6364055190875,-15.8895273598811));
#52845=CARTESIAN_POINT('Ctrl Pts',(5.57595554966988,39.8445853883982,-15.5293116329089));
#52846=CARTESIAN_POINT('Ctrl Pts',(5.32093394283459,39.7743589127886,-15.6208743387635));
#52847=CARTESIAN_POINT('Ctrl Pts',(5.26811263571756,39.7380180145649,-15.8933294601772));
#52848=CARTESIAN_POINT('Ctrl Pts',(5.53599851525571,40.004450203368,-15.5435813267104));
#52849=CARTESIAN_POINT('Ctrl Pts',(5.28579906825781,39.929705256497,-15.632690927334));
#52850=CARTESIAN_POINT('Ctrl Pts',(5.23068731473301,39.8899479695032,-15.9000967087543));
#52851=CARTESIAN_POINT('Ctrl Pts',(5.5221305599358,40.0576617611033,-15.5485146750299));
#52852=CARTESIAN_POINT('Ctrl Pts',(5.27355459719845,39.9813594979742,-15.6367961486595));
#52853=CARTESIAN_POINT('Ctrl Pts',(5.2176980449392,39.9405097816184,-15.9025298069678));
#52854=CARTESIAN_POINT('Ctrl Pts',(5.50047699149048,40.1373603819414,-15.556182420383));
#52855=CARTESIAN_POINT('Ctrl Pts',(5.25432923497206,40.0587687077115,-15.6432168973992));
#52856=CARTESIAN_POINT('Ctrl Pts',(5.19741646594872,40.0162266424403,-15.9064481481372));
#52857=CARTESIAN_POINT('Ctrl Pts',(5.49311741536451,40.1639050501549,-15.5587828592327));
#52858=CARTESIAN_POINT('Ctrl Pts',(5.24778336468827,40.0845377385951,-15.6453990618431));
#52859=CARTESIAN_POINT('Ctrl Pts',(5.19052319892915,40.041442951149,-15.907799028716));
#52860=CARTESIAN_POINT('Ctrl Pts',(5.47814593729634,40.2168282263209,-15.5640605270417));
#52861=CARTESIAN_POINT('Ctrl Pts',(5.23443708951077,40.1359150171577,-15.649839332167));
#52862=CARTESIAN_POINT('Ctrl Pts',(5.17650032697911,40.0917133649177,-15.9105838634));
#52863=CARTESIAN_POINT('Ctrl Pts',(5.470529823742,40.2432224288697,-15.5667392494243));
#52864=CARTESIAN_POINT('Ctrl Pts',(5.22763310795184,40.1615391166161,-15.6520986436733));
#52865=CARTESIAN_POINT('Ctrl Pts',(5.16936677702167,40.1167823811518,-15.9120185729299));
#52866=CARTESIAN_POINT('Ctrl Pts',(5.40080286686056,40.4801601691466,-15.5912040190124));
#52867=CARTESIAN_POINT('Ctrl Pts',(5.1654386504834,40.3907259377088,-15.672707312104));
#52868=CARTESIAN_POINT('Ctrl Pts',(5.10405778192814,40.3418044912576,-15.9253090687417));
#52869=CARTESIAN_POINT('Ctrl Pts',(5.33043670111554,40.6864411445816,-15.6154875831029));
#52870=CARTESIAN_POINT('Ctrl Pts',(5.10156582395526,40.5911762940015,-15.6935809949587));
#52871=CARTESIAN_POINT('Ctrl Pts',(5.03815007775546,40.5375718116029,-15.9398148438705));
#52872=CARTESIAN_POINT('Ctrl Pts',(5.17171535959732,41.0898251595944,-15.6687704725657));
#52873=CARTESIAN_POINT('Ctrl Pts',(4.9558472522213,40.9828549133869,-15.739985220476));
#52874=CARTESIAN_POINT('Ctrl Pts',(4.88948546120424,40.9201248480408,-15.9738813871344));
#52875=CARTESIAN_POINT('Ctrl Pts',(5.08336558250042,41.2869305832741,-15.6977708167442));
#52876=CARTESIAN_POINT('Ctrl Pts',(4.87405064261176,41.1743746865059,-15.7655101753502));
#52877=CARTESIAN_POINT('Ctrl Pts',(4.80673360287453,41.1069127909073,-15.9934430495542));
#52878=CARTESIAN_POINT('Ctrl Pts',(4.88694399553687,41.671218731313,-15.7600251473423));
#52879=CARTESIAN_POINT('Ctrl Pts',(4.69092137437619,41.5474552367694,-15.8207627043341));
#52880=CARTESIAN_POINT('Ctrl Pts',(4.62275746195378,41.4708178044506,-16.0372007396695));
#52881=CARTESIAN_POINT('Ctrl Pts',(4.77888228918939,41.858405974228,-15.7932806671364));
#52882=CARTESIAN_POINT('Ctrl Pts',(4.58961749308463,41.7292760041513,-15.8504958068979));
#52883=CARTESIAN_POINT('Ctrl Pts',(4.5215426392795,41.6479391144314,-16.0613980705431));
#52884=CARTESIAN_POINT('Ctrl Pts',(4.64482519461143,42.0628061930575,-15.8327458139082));
#52885=CARTESIAN_POINT('Ctrl Pts',(4.46310917160174,41.9280541129356,-15.8860546410961));
#52886=CARTESIAN_POINT('Ctrl Pts',(4.39597952121523,41.8412001847982,-16.0909199817576));
#52887=CARTESIAN_POINT('Ctrl Pts',(4.62976965412125,42.0854096858801,-15.8371551458627));
#52888=CARTESIAN_POINT('Ctrl Pts',(4.44892446825342,41.9499886943975,-15.8900217942609));
#52889=CARTESIAN_POINT('Ctrl Pts',(4.38187791293436,41.8625697484028,-16.0942290007409));
#52890=CARTESIAN_POINT('Ctrl Pts',(4.59939878543121,42.1303067904093,-15.8460020502624));
#52891=CARTESIAN_POINT('Ctrl Pts',(4.42029652797858,41.9935550766478,-15.8979866657635));
#52892=CARTESIAN_POINT('Ctrl Pts',(4.35343136929109,41.9050117576583,-16.1008888977657));
#52893=CARTESIAN_POINT('Ctrl Pts',(4.58407427222009,42.1526144588579,-15.8504423301015));
#52894=CARTESIAN_POINT('Ctrl Pts',(4.40584455629757,42.0152010592343,-15.9019868666117));
#52895=CARTESIAN_POINT('Ctrl Pts',(4.3390778307107,41.9260974941438,-16.1042417996911));
#52896=CARTESIAN_POINT('Ctrl Pts',(4.53768208250935,42.2191142602777,-15.8638103017682));
#52897=CARTESIAN_POINT('Ctrl Pts',(4.36208642108868,42.0797067591165,-15.914033937939));
#52898=CARTESIAN_POINT('Ctrl Pts',(4.2956250910933,41.9889485291262,-16.1143660947964));
#52899=CARTESIAN_POINT('Ctrl Pts',(4.50619581303838,42.2628832431857,-15.8727851349316));
#52900=CARTESIAN_POINT('Ctrl Pts',(4.33235251838812,42.1221742523451,-15.9221344733298));
#52901=CARTESIAN_POINT('Ctrl Pts',(4.26613381932855,42.0303077037197,-16.121203084525));
#52902=CARTESIAN_POINT('Ctrl Pts',(4.41004926624052,42.3924912295783,-15.8998710702299));
#52903=CARTESIAN_POINT('Ctrl Pts',(4.24153152750805,42.2478448168248,-15.9465961576241));
#52904=CARTESIAN_POINT('Ctrl Pts',(4.1760792026318,42.1527559308387,-16.1419500461017));
#52905=CARTESIAN_POINT('Ctrl Pts',(4.34370225939985,42.4766322174293,-15.9181437877767));
#52906=CARTESIAN_POINT('Ctrl Pts',(4.17872361398144,42.3294747743511,-15.9631463234755));
#52907=CARTESIAN_POINT('Ctrl Pts',(4.11393600041315,42.2322165809747,-16.1560961451583));
#52908=CARTESIAN_POINT('Ctrl Pts',(4.13777251537753,42.7221794291726,-15.9733854419649));
#52909=CARTESIAN_POINT('Ctrl Pts',(3.98370692807761,42.5673833142134,-16.0132260504743));
#52910=CARTESIAN_POINT('Ctrl Pts',(3.92105414688791,42.4640154815466,-16.1992634768941));
#52911=CARTESIAN_POINT('Ctrl Pts',(3.99132195149594,42.8767293832158,-16.0107821043782));
#52912=CARTESIAN_POINT('Ctrl Pts',(3.84451111612512,42.7173047864165,-16.0473039779341));
#52913=CARTESIAN_POINT('Ctrl Pts',(3.78388281919657,42.6097890780496,-16.2290170151344));
#52914=CARTESIAN_POINT('Ctrl Pts',(3.75700972962784,43.0941951466418,-16.0667771043254));
#52915=CARTESIAN_POINT('Ctrl Pts',(3.62129524685035,42.9281698633173,-16.0984923203175));
#52916=CARTESIAN_POINT('Ctrl Pts',(3.56441682684187,42.8147476794126,-16.2742016702415));
#52917=CARTESIAN_POINT('Ctrl Pts',(3.67646144559015,43.1642860455141,-16.0854244903344));
#52918=CARTESIAN_POINT('Ctrl Pts',(3.54454660494019,42.9960786893441,-16.115553648241));
#52919=CARTESIAN_POINT('Ctrl Pts',(3.48897215266966,42.8807793342241,-16.2893548851606));
#52920=CARTESIAN_POINT('Ctrl Pts',(3.55180835016696,43.2656968454944,-16.1132389634261));
#52921=CARTESIAN_POINT('Ctrl Pts',(3.42566053370466,43.0943214418982,-16.1410401047175));
#52922=CARTESIAN_POINT('Ctrl Pts',(3.37221718759655,42.9762779466704,-16.3121000330166));
#52923=CARTESIAN_POINT('Ctrl Pts',(3.50961052575669,43.2988851470272,-16.122485966165));
#52924=CARTESIAN_POINT('Ctrl Pts',(3.38541262458361,43.1264600581356,-16.1495163495703));
#52925=CARTESIAN_POINT('Ctrl Pts',(3.33269305445803,43.0075246336688,-16.3196856337079));
#52926=CARTESIAN_POINT('Ctrl Pts',(3.4239361870611,43.3639679820918,-16.1408977680494));
#52927=CARTESIAN_POINT('Ctrl Pts',(3.30367271591507,43.189473362121,-16.1664034224739));
#52928=CARTESIAN_POINT('Ctrl Pts',(3.25244711732724,43.0687868973452,-16.3348347973778));
#52929=CARTESIAN_POINT('Ctrl Pts',(3.38069422093024,43.3956846955611,-16.1500121560905));
#52930=CARTESIAN_POINT('Ctrl Pts',(3.26240299114715,43.2201782549395,-16.1747684968875));
#52931=CARTESIAN_POINT('Ctrl Pts',(3.21194500033968,43.0986350973994,-16.3423568657999));
#52932=CARTESIAN_POINT('Ctrl Pts',(3.16247293665689,43.5501883769039,-16.1950777040967));
#52933=CARTESIAN_POINT('Ctrl Pts',(3.05423596689228,43.3696142664887,-16.2161210510762));
#52934=CARTESIAN_POINT('Ctrl Pts',(3.00755040891255,43.2440053764108,-16.3796546335878));
#52935=CARTESIAN_POINT('Ctrl Pts',(2.98147832252801,43.660776482398,-16.2295084233055));
#52936=CARTESIAN_POINT('Ctrl Pts',(2.88121816202138,43.4766418873115,-16.2478293654573));
#52937=CARTESIAN_POINT('Ctrl Pts',(2.83802377309921,43.3479542916528,-16.4084895185999));
#52938=CARTESIAN_POINT('Ctrl Pts',(2.70037397572554,43.8074863821001,-16.277807578224));
#52939=CARTESIAN_POINT('Ctrl Pts',(2.61232205384454,43.6184982166501,-16.2923899551782));
#52940=CARTESIAN_POINT('Ctrl Pts',(2.57473044561691,43.4857336160062,-16.4493217081974));
#52941=CARTESIAN_POINT('Ctrl Pts',(2.60506670587299,43.8531862697985,-16.2933497575293));
#52942=CARTESIAN_POINT('Ctrl Pts',(2.52114721824606,43.6626594710407,-16.3067415552332));
#52943=CARTESIAN_POINT('Ctrl Pts',(2.48546192830491,43.528628365131,-16.4625297245561));
#52944=CARTESIAN_POINT('Ctrl Pts',(2.41119452256951,43.9381353686842,-16.3231663545269));
#52945=CARTESIAN_POINT('Ctrl Pts',(2.3356478240054,43.7447042632128,-16.3342999073));
#52946=CARTESIAN_POINT('Ctrl Pts',(2.3038736575641,43.6083197721399,-16.4879921624111));
#52947=CARTESIAN_POINT('Ctrl Pts',(2.31262977609044,43.9773848957545,-16.3374408791774));
#52948=CARTESIAN_POINT('Ctrl Pts',(2.24131140491693,43.7825970865653,-16.3475093049691));
#52949=CARTESIAN_POINT('Ctrl Pts',(2.21155406016932,43.6451167254636,-16.5002466751902));
#52950=CARTESIAN_POINT('Ctrl Pts',(2.16227751834144,44.0313312810579,-16.3577844977291));
#52951=CARTESIAN_POINT('Ctrl Pts',(2.09738048924219,43.8346499499766,-16.3663562334774));
#52952=CARTESIAN_POINT('Ctrl Pts',(2.07072825413426,43.6956582712672,-16.5178019271295));
#52953=CARTESIAN_POINT('Ctrl Pts',(2.11174227376284,44.0484914663749,-16.3643876348749));
#52954=CARTESIAN_POINT('Ctrl Pts',(2.04900260649854,43.8512017716587,-16.3724769498617));
#52955=CARTESIAN_POINT('Ctrl Pts',(2.02339496711712,43.7117292100671,-16.523515913095));
#52956=CARTESIAN_POINT('Ctrl Pts',(2.03530194931424,44.072981459843,-16.3740100616474));
#52957=CARTESIAN_POINT('Ctrl Pts',(1.97581878875163,43.8748161029352,-16.3814021297576));
#52958=CARTESIAN_POINT('Ctrl Pts',(1.95179796907649,43.7346553851609,-16.5318661099767));
#52959=CARTESIAN_POINT('Ctrl Pts',(2.00971557668972,44.0809363660402,-16.3771704866985));
#52960=CARTESIAN_POINT('Ctrl Pts',(1.95132227885587,43.8824850165059,-16.3843344340238));
#52961=CARTESIAN_POINT('Ctrl Pts',(1.92783277153264,43.742100695679,-16.5346127099434));
#52962=CARTESIAN_POINT('Ctrl Pts',(1.95832824291746,44.0964258747234,-16.3833946525917));
#52963=CARTESIAN_POINT('Ctrl Pts',(1.90212235254287,43.8974148464812,-16.3901112587382));
#52964=CARTESIAN_POINT('Ctrl Pts',(1.87970138457326,43.7565946460749,-16.5400299284974));
#52965=CARTESIAN_POINT('Ctrl Pts',(1.93251110054407,44.1039650287676,-16.3864602701835));
#52966=CARTESIAN_POINT('Ctrl Pts',(1.87740326220016,43.9046802305651,-16.392957550475));
#52967=CARTESIAN_POINT('Ctrl Pts',(1.85552003909345,43.7636475423924,-16.5427021859492));
#52968=CARTESIAN_POINT('Ctrl Pts',(1.8030633147258,44.1405497707181,-16.4015192016935));
#52969=CARTESIAN_POINT('Ctrl Pts',(1.75346736507588,43.9399264952154,-16.4069429652539));
#52970=CARTESIAN_POINT('Ctrl Pts',(1.73427417901659,43.7978641021233,-16.5558492664266));
#52971=CARTESIAN_POINT('Ctrl Pts',(1.69906639420128,44.1660683153088,-16.4126226120353));
#52972=CARTESIAN_POINT('Ctrl Pts',(1.65387335486775,43.9644920355918,-16.417272571238));
#52973=CARTESIAN_POINT('Ctrl Pts',(1.63686659515066,43.8217027186776,-16.5656092158287));
#52974=CARTESIAN_POINT('Ctrl Pts',(1.49021426166529,44.2098252495483,-16.4329020282884));
#52975=CARTESIAN_POINT('Ctrl Pts',(1.45386135654879,44.0065631227143,-16.4361701532582));
#52976=CARTESIAN_POINT('Ctrl Pts',(1.44124751778221,43.862520976467,-16.5835644832772));
#52977=CARTESIAN_POINT('Ctrl Pts',(1.38535902634819,44.2280633796216,-16.4420780728859));
#52978=CARTESIAN_POINT('Ctrl Pts',(1.35343204203413,44.0240714574058,-16.4447394017829));
#52979=CARTESIAN_POINT('Ctrl Pts',(1.34303600264843,43.8795003686096,-16.5917598520244));
#52980=CARTESIAN_POINT('Ctrl Pts',(1.17479908853176,44.2573750378148,-16.4584628106134));
#52981=CARTESIAN_POINT('Ctrl Pts',(1.15176493152459,44.0521448192979,-16.4600782830589));
#52982=CARTESIAN_POINT('Ctrl Pts',(1.14581732809311,43.906712349358,-16.6065414193849));
#52983=CARTESIAN_POINT('Ctrl Pts',(1.06909438111656,44.2684484921629,-16.4656715398477));
#52984=CARTESIAN_POINT('Ctrl Pts',(1.05051664045048,44.0627110998794,-16.4668487116589));
#52985=CARTESIAN_POINT('Ctrl Pts',(1.04681016412825,43.9169448659429,-16.6131276573267));
#52986=CARTESIAN_POINT('Ctrl Pts',(0.856834555596582,44.2834493850702,-16.4780804888865));
#52987=CARTESIAN_POINT('Ctrl Pts',(0.847217272305147,44.0769219395685,-16.4785516187993));
#52988=CARTESIAN_POINT('Ctrl Pts',(0.847999308275245,43.9306827648361,-16.6246496409757));
#52989=CARTESIAN_POINT('Ctrl Pts',(0.750279450442107,44.2873769285557,-16.4832807449414));
#52990=CARTESIAN_POINT('Ctrl Pts',(0.745156101872444,44.0805664549735,-16.483484482518));
#52991=CARTESIAN_POINT('Ctrl Pts',(0.748195628510673,43.9341882452755,-16.62958541764));
#52992=CARTESIAN_POINT('Ctrl Pts',(0.58980086051462,44.2878495874714,-16.4895421642784));
#52993=CARTESIAN_POINT('Ctrl Pts',(0.591467911154747,44.0807865596362,-16.4894752008505));
#52994=CARTESIAN_POINT('Ctrl Pts',(0.597885103513613,43.9343461853688,-16.6357218580272));
#52995=CARTESIAN_POINT('Ctrl Pts',(0.536200263354332,44.2871032596941,-16.4913727887242));
#52996=CARTESIAN_POINT('Ctrl Pts',(0.540132926138202,44.0799845128224,-16.4912375073698));
#52997=CARTESIAN_POINT('Ctrl Pts',(0.547680687440361,43.9335480497144,-16.6375561481366));
#52998=CARTESIAN_POINT('Ctrl Pts',(0.455636014550893,44.284613337201,-16.4937296454446));
#52999=CARTESIAN_POINT('Ctrl Pts',(0.462979747202555,44.0774546459417,-16.4935249270376));
#53000=CARTESIAN_POINT('Ctrl Pts',(0.47222106046037,43.9310609294277,-16.6399872269088));
#53001=CARTESIAN_POINT('Ctrl Pts',(0.428754034222533,44.2835549068502,-16.4944504159164));
#53002=CARTESIAN_POINT('Ctrl Pts',(0.437235366462993,44.0763900837954,-16.4942280935165));
#53003=CARTESIAN_POINT('Ctrl Pts',(0.447042346105144,43.9300168543709,-16.6407441942414));
#53004=CARTESIAN_POINT('Ctrl Pts',(0.388389950057066,44.2816222765731,-16.4954337434013));
#53005=CARTESIAN_POINT('Ctrl Pts',(0.398580882778724,44.0744592385522,-16.4951933304063));
#53006=CARTESIAN_POINT('Ctrl Pts',(0.409235765892974,43.9281260198428,-16.6417991152495));
#53007=CARTESIAN_POINT('Ctrl Pts',(0.374928402732455,44.2809205658472,-16.4957452143992));
#53008=CARTESIAN_POINT('Ctrl Pts',(0.385689351820399,44.0737599283669,-16.4955001651808));
#53009=CARTESIAN_POINT('Ctrl Pts',(0.396627154075427,43.9274416182168,-16.6421373338812));
#53010=CARTESIAN_POINT('Ctrl Pts',(0.347991554057913,44.2794017185444,-16.4963354525741));
#53011=CARTESIAN_POINT('Ctrl Pts',(0.359893363301771,44.072249540534,-16.4960839175124));
#53012=CARTESIAN_POINT('Ctrl Pts',(0.371397047876984,43.9259641674669,-16.6427868545954));
#53013=CARTESIAN_POINT('Ctrl Pts',(0.334532328343637,44.2785856289167,-16.4966139069159));
#53014=CARTESIAN_POINT('Ctrl Pts',(0.347004279162573,44.0714394948401,-16.496360523009));
#53015=CARTESIAN_POINT('Ctrl Pts',(0.358790610672238,43.925172130238,-16.6430978003365));
#53016=CARTESIAN_POINT('Ctrl Pts',(0.321034048597817,44.2777095070773,-16.496876587392));
#53017=CARTESIAN_POINT('Ctrl Pts',(0.334078182671872,44.0705712895835,-16.4966227447236));
#53018=CARTESIAN_POINT('Ctrl Pts',(0.346147593727982,43.9243235322772,-16.6433959637249));
#53019=CARTESIAN_POINT('',(0.730430568056981,29.0999736046314,-17.3364718010719));
#53020=CARTESIAN_POINT('Origin',(0.753473624776453,28.7467958754239,-16.9832940708441));
#53021=CARTESIAN_POINT('',(0.500000000000003,43.9319757376251,-16.6390920749471));
#53022=CARTESIAN_POINT('Ctrl Pts',(0.499999999999999,43.9319757373861,-16.6390920747081));
#53023=CARTESIAN_POINT('Ctrl Pts',(0.54757507396084,43.9335156191108,-16.637552201127));
#53024=CARTESIAN_POINT('Ctrl Pts',(0.595061829101537,43.9342864984895,-16.6358212644215));
#53025=CARTESIAN_POINT('Ctrl Pts',(0.642461141705286,43.9342958947873,-16.6339011638695));
#53026=CARTESIAN_POINT('Ctrl Pts',(0.644303763883716,43.9342962600632,-16.6338265210178));
#53027=CARTESIAN_POINT('Ctrl Pts',(0.646146253911932,43.9342954745885,-16.6337515922788));
#53028=CARTESIAN_POINT('Ctrl Pts',(0.647988611841277,43.9342935388005,-16.6336763777689));
#53029=CARTESIAN_POINT('Ctrl Pts',(0.748182861165585,43.9341882634795,-16.6295859340796));
#53030=CARTESIAN_POINT('Ctrl Pts',(0.847986714017941,43.9306837682061,-16.6246502377895));
#53031=CARTESIAN_POINT('Ctrl Pts',(0.947404736988193,43.9238138935806,-16.6188885708602));
#53032=CARTESIAN_POINT('Ctrl Pts',(0.94901269818106,43.9237027820189,-16.6187953831609));
#53033=CARTESIAN_POINT('Ctrl Pts',(0.950620558440654,43.923590790085,-16.618701979389));
#53034=CARTESIAN_POINT('Ctrl Pts',(0.952228317766542,43.923477917725,-16.6186083596307));
#53035=CARTESIAN_POINT('Ctrl Pts',(1.05000098985128,43.9166138106022,-16.6129150610295));
#53036=CARTESIAN_POINT('Ctrl Pts',(1.14740041286262,43.9064940712208,-16.6064226132333));
#53037=CARTESIAN_POINT('Ctrl Pts',(1.24442667068965,43.8931064533492,-16.5991505402067));
#53038=CARTESIAN_POINT('Ctrl Pts',(1.24945646130347,43.8924124462194,-16.5987735597328));
#53039=CARTESIAN_POINT('Ctrl Pts',(1.25448524909501,43.8917096574055,-16.5983944840538));
#53040=CARTESIAN_POINT('Ctrl Pts',(1.25951303346151,43.8909980790404,-16.5980133161075));
#53041=CARTESIAN_POINT('Ctrl Pts',(1.35304288501814,43.8777608727477,-16.5909226020196));
#53042=CARTESIAN_POINT('Ctrl Pts',(1.44622544709215,43.8614824877767,-16.5831073592102));
#53043=CARTESIAN_POINT('Ctrl Pts',(1.53905706853458,43.8421119644684,-16.5745867290311));
#53044=CARTESIAN_POINT('Ctrl Pts',(1.54747921114386,43.8403545750445,-16.5738136954314));
#53045=CARTESIAN_POINT('Ctrl Pts',(1.55589846523983,43.8385717359699,-16.573034855426));
#53046=CARTESIAN_POINT('Ctrl Pts',(1.56431482499405,43.836763377988,-16.5722502247802));
#53047=CARTESIAN_POINT('Ctrl Pts',(1.61490694532871,43.8258930412507,-16.5675336811424));
#53048=CARTESIAN_POINT('Ctrl Pts',(1.66539452408273,43.8141007838391,-16.5626077013854));
#53049=CARTESIAN_POINT('Ctrl Pts',(1.71577613901276,43.801371606282,-16.5574757157637));
#53050=CARTESIAN_POINT('Ctrl Pts',(1.74096694647778,43.7950070175034,-16.5549097229528));
#53051=CARTESIAN_POINT('Ctrl Pts',(1.76613180612446,43.7884080514811,-16.5522921712238));
#53052=CARTESIAN_POINT('Ctrl Pts',(1.79126896359321,43.7815732750681,-16.5496236439717));
#53053=CARTESIAN_POINT('Ctrl Pts',(1.80462156274624,43.7779427122307,-16.5482061497792));
#53054=CARTESIAN_POINT('Ctrl Pts',(1.81795404850408,43.774248976217,-16.5467755794718));
#53055=CARTESIAN_POINT('Ctrl Pts',(1.83127086873843,43.7704908653263,-16.5453315904083));
#53056=CARTESIAN_POINT('Ctrl Pts',(1.8430238497748,43.7671740820963,-16.5440571738599));
#53057=CARTESIAN_POINT('Ctrl Pts',(1.85475472764573,43.7638098150535,-16.542773365422));
#53058=CARTESIAN_POINT('Ctrl Pts',(1.8664611512278,43.7603990665573,-16.5414805958159));
#53059=CARTESIAN_POINT('Ctrl Pts',(1.87892371112219,43.7567680124509,-16.5401043241876));
#53060=CARTESIAN_POINT('Ctrl Pts',(1.89136121499753,43.7530834984364,-16.5387175946662));
#53061=CARTESIAN_POINT('Ctrl Pts',(1.90376708010395,43.7493476834398,-16.5373213058091));
#53062=CARTESIAN_POINT('Ctrl Pts',(1.92783628123464,43.7420996534339,-16.5346123002663));
#53063=CARTESIAN_POINT('Ctrl Pts',(1.95180155045399,43.7346542585673,-16.5318656721187));
#53064=CARTESIAN_POINT('Ctrl Pts',(1.9756636395166,43.727013352029,-16.5290826838497));
#53065=CARTESIAN_POINT('Ctrl Pts',(2.02341050023379,43.711724275734,-16.523514061886));
#53066=CARTESIAN_POINT('Ctrl Pts',(2.07074432095206,43.6956525615114,-16.5177998678728));
#53067=CARTESIAN_POINT('Ctrl Pts',(2.11767019917302,43.6788111378344,-16.5119501232939));
#53068=CARTESIAN_POINT('Ctrl Pts',(2.1320820175734,43.6736388203661,-16.5101535568842));
#53069=CARTESIAN_POINT('Ctrl Pts',(2.14645538566519,43.6683939604828,-16.5083442063354));
#53070=CARTESIAN_POINT('Ctrl Pts',(2.16079040024107,43.6630768264416,-16.5065223583721));
#53071=CARTESIAN_POINT('Ctrl Pts',(2.2399049257387,43.6337317194346,-16.4964676328341));
#53072=CARTESIAN_POINT('Ctrl Pts',(2.31785505285204,43.6021840003903,-16.4860316105865));
#53073=CARTESIAN_POINT('Ctrl Pts',(2.39466780777821,43.5684741281802,-16.4752608753432));
#53074=CARTESIAN_POINT('Ctrl Pts',(2.41141236199445,43.5611256509202,-16.4729129428885));
#53075=CARTESIAN_POINT('Ctrl Pts',(2.4281028618955,43.5536744165793,-16.4705491005035));
#53076=CARTESIAN_POINT('Ctrl Pts',(2.44473947828146,43.5461206147242,-16.4681698275028));
#53077=CARTESIAN_POINT('Ctrl Pts',(2.51837530250979,43.5126865069253,-16.4576388562759));
#53078=CARTESIAN_POINT('Ctrl Pts',(2.59095573626851,43.4772437713182,-16.4468047325651));
#53079=CARTESIAN_POINT('Ctrl Pts',(2.66249507797947,43.4398078078865,-16.4357102161998));
#53080=CARTESIAN_POINT('Ctrl Pts',(2.6812634654843,43.4299864613169,-16.4327995634409));
#53081=CARTESIAN_POINT('Ctrl Pts',(2.69996035641465,43.4200282774449,-16.4298709581876));
#53082=CARTESIAN_POINT('Ctrl Pts',(2.71858578544062,43.4099330595632,-16.4269251921389));
#53083=CARTESIAN_POINT('Ctrl Pts',(2.80820564226487,43.3613579647343,-16.4127510686246));
#53084=CARTESIAN_POINT('Ctrl Pts',(2.89617177777919,43.3096119447071,-16.3981772518944));
#53085=CARTESIAN_POINT('Ctrl Pts',(2.98248669111425,43.2546769047821,-16.3832893654412));
#53086=CARTESIAN_POINT('Ctrl Pts',(3.04624678339623,43.2140968580695,-16.3722918103552));
#53087=CARTESIAN_POINT('Ctrl Pts',(3.10910599739674,43.1717766342996,-16.3611228479354));
#53088=CARTESIAN_POINT('Ctrl Pts',(3.17106608205426,43.1277091532017,-16.3498164193575));
#53089=CARTESIAN_POINT('Ctrl Pts',(3.19298415920671,43.1121204971184,-16.3458168255019));
#53090=CARTESIAN_POINT('Ctrl Pts',(3.21478940308917,43.0963124984015,-16.3418000833344));
#53091=CARTESIAN_POINT('Ctrl Pts',(3.23648155363809,43.0802841038743,-16.337767760884));
#53092=CARTESIAN_POINT('Ctrl Pts',(3.25526256696086,43.0664067572977,-16.3342765855167));
#53093=CARTESIAN_POINT('Ctrl Pts',(3.27395704672654,43.0523655430299,-16.3307740629455));
#53094=CARTESIAN_POINT('Ctrl Pts',(3.29257008801342,43.0381557703974,-16.327260208633));
#53095=CARTESIAN_POINT('Ctrl Pts',(3.29452482545658,43.036663463246,-16.326891184437));
#53096=CARTESIAN_POINT('Ctrl Pts',(3.29647814310812,43.0351696939639,-16.3265221337238));
#53097=CARTESIAN_POINT('Ctrl Pts',(3.2984300462081,43.0336744612953,-16.3261530570622));
#53098=CARTESIAN_POINT('Ctrl Pts',(3.31896800193379,43.0179415991738,-16.32226962651));
#53099=CARTESIAN_POINT('Ctrl Pts',(3.33933859097246,43.0020550620894,-16.31838528869));
#53100=CARTESIAN_POINT('Ctrl Pts',(3.35954417450593,42.9860167729483,-16.3145016519096));
#53101=CARTESIAN_POINT('Ctrl Pts',(3.37686185179866,42.9722707747091,-16.311173088378));
#53102=CARTESIAN_POINT('Ctrl Pts',(3.3940591510392,42.9584126400607,-16.3078448597278));
#53103=CARTESIAN_POINT('Ctrl Pts',(3.41113553968154,42.9444451416336,-16.3045182205045));
#53104=CARTESIAN_POINT('Ctrl Pts',(3.43390726592552,42.9258191863946,-16.3000820765813));
#53105=CARTESIAN_POINT('Ctrl Pts',(3.45646665672014,42.9069969381795,-16.2956483038387));
#53106=CARTESIAN_POINT('Ctrl Pts',(3.47881642783259,42.8879810486537,-16.2912189212696));
#53107=CARTESIAN_POINT('Ctrl Pts',(3.53295111922232,42.8419215473818,-16.2804902539728));
#53108=CARTESIAN_POINT('Ctrl Pts',(3.58585566131758,42.7947261750183,-16.2697875919548));
#53109=CARTESIAN_POINT('Ctrl Pts',(3.63757222655503,42.7464282781409,-16.2591399074602));
#53110=CARTESIAN_POINT('Ctrl Pts',(3.66058117518797,42.7249403115052,-16.2544027014128));
#53111=CARTESIAN_POINT('Ctrl Pts',(3.6833554158427,42.703234527098,-16.2496764460396));
#53112=CARTESIAN_POINT('Ctrl Pts',(3.70589760765789,42.6813128786821,-16.2449634978511));
#53113=CARTESIAN_POINT('Ctrl Pts',(3.77910724856877,42.6101185590761,-16.2296573888739));
#53114=CARTESIAN_POINT('Ctrl Pts',(3.84987008319856,42.5366475241466,-16.2144909403196));
#53115=CARTESIAN_POINT('Ctrl Pts',(3.91827600714043,42.4609673017849,-16.1995435117613));
#53116=CARTESIAN_POINT('Ctrl Pts',(3.96306685152826,42.4114133908412,-16.189756231538));
#53117=CARTESIAN_POINT('Ctrl Pts',(4.00684717481627,42.3609123166451,-16.1800628313719));
#53118=CARTESIAN_POINT('Ctrl Pts',(4.04964204923807,42.3094828811653,-16.1704852557369));
#53119=CARTESIAN_POINT('Ctrl Pts',(4.07220479342806,42.2823677368346,-16.1654356699645));
#53120=CARTESIAN_POINT('Ctrl Pts',(4.0944930048392,42.2549939657261,-16.1604181756657));
#53121=CARTESIAN_POINT('Ctrl Pts',(4.11650923860563,42.2273632732543,-16.1554357947868));
#53122=CARTESIAN_POINT('Ctrl Pts',(4.15730666926082,42.1761619064796,-16.1462031376228));
#53123=CARTESIAN_POINT('Ctrl Pts',(4.19717010962387,42.1240783986472,-16.1370910810339));
#53124=CARTESIAN_POINT('Ctrl Pts',(4.23611561389655,42.0711237796144,-16.1281187379831));
#53125=CARTESIAN_POINT('Ctrl Pts',(4.25804971753198,42.0412997441184,-16.1230655153839));
#53126=CARTESIAN_POINT('Ctrl Pts',(4.27969252966859,42.0111992773893,-16.1180565875598));
#53127=CARTESIAN_POINT('Ctrl Pts',(4.30104638713536,41.9808238526934,-16.1130952728204));
#53128=CARTESIAN_POINT('Ctrl Pts',(4.30893484767529,41.9696026792137,-16.1112624828616));
#53129=CARTESIAN_POINT('Ctrl Pts',(4.31678390039683,41.9583439471152,-16.1094361833301));
#53130=CARTESIAN_POINT('Ctrl Pts',(4.3245935860754,41.947047841699,-16.1076165589678));
#53131=CARTESIAN_POINT('Ctrl Pts',(4.33908272363761,41.9260904265059,-16.1042406500284));
#53132=CARTESIAN_POINT('Ctrl Pts',(4.35343634228928,41.9050043553989,-16.1008877162269));
#53133=CARTESIAN_POINT('Ctrl Pts',(4.36765465067981,41.8837907656036,-16.0975589201664));
#53134=CARTESIAN_POINT('Ctrl Pts',(4.37456285478427,41.8734837864561,-16.095941568652));
#53135=CARTESIAN_POINT('Ctrl Pts',(4.38144114610487,41.8631435705445,-16.0943294377919));
#53136=CARTESIAN_POINT('Ctrl Pts',(4.38828623834093,41.8527753534199,-16.0927234372925));
#53137=CARTESIAN_POINT('Ctrl Pts',(4.3954180381469,41.8419728621857,-16.0910501692552));
#53138=CARTESIAN_POINT('Ctrl Pts',(4.40251835272474,41.831132964736,-16.0893825383176));
#53139=CARTESIAN_POINT('Ctrl Pts',(4.40957575112323,41.8202734186026,-16.0877232796263));
#53140=CARTESIAN_POINT('Ctrl Pts',(4.40969417252988,41.8200911980936,-16.0876954376742));
#53141=CARTESIAN_POINT('Ctrl Pts',(4.40981258274751,41.8199089706728,-16.0876675978901));
#53142=CARTESIAN_POINT('Ctrl Pts',(4.40993098176058,41.8197267363653,-16.0876397602783));
#53143=CARTESIAN_POINT('Ctrl Pts',(4.41686864658674,41.8090486022141,-16.0860085978618));
#53144=CARTESIAN_POINT('Ctrl Pts',(4.42376480089258,41.7983519052827,-16.0843856692356));
#53145=CARTESIAN_POINT('Ctrl Pts',(4.4306200950024,41.7876363110569,-16.082770920866));
#53146=CARTESIAN_POINT('Ctrl Pts',(4.50034296874691,41.6786516327428,-16.0663478622927));
#53147=CARTESIAN_POINT('Ctrl Pts',(4.56582956218176,41.5677267230489,-16.0507749291748));
#53148=CARTESIAN_POINT('Ctrl Pts',(4.62741559217832,41.4550012090001,-16.0361118852648));
#53149=CARTESIAN_POINT('Ctrl Pts',(4.6574401945597,41.4000449350247,-16.0289633149945));
#53150=CARTESIAN_POINT('Ctrl Pts',(4.686537451899,41.3446609425631,-16.022030998685));
#53151=CARTESIAN_POINT('Ctrl Pts',(4.71474554668843,41.288865313039,-16.0153218476222));
#53152=CARTESIAN_POINT('Ctrl Pts',(4.73282548062373,41.2531031921583,-16.0110216278136));
#53153=CARTESIAN_POINT('Ctrl Pts',(4.75053975868617,41.2171717968373,-16.0068130360076));
#53154=CARTESIAN_POINT('Ctrl Pts',(4.76789567688245,41.1810741471843,-16.0026974052181));
#53155=CARTESIAN_POINT('Ctrl Pts',(4.81233008924746,41.088657380065,-15.9921606169265));
#53156=CARTESIAN_POINT('Ctrl Pts',(4.85441591615076,40.9951507454576,-15.9822329668367));
#53157=CARTESIAN_POINT('Ctrl Pts',(4.89427385518969,40.9006052087616,-15.972936464702));
#53158=CARTESIAN_POINT('Ctrl Pts',(4.91825289509361,40.8437254188921,-15.9673435715162));
#53159=CARTESIAN_POINT('Ctrl Pts',(4.9414255696942,40.7864694656732,-15.9619791627489));
#53160=CARTESIAN_POINT('Ctrl Pts',(4.96381780586936,40.7288483629628,-15.9568479803831));
#53161=CARTESIAN_POINT('Ctrl Pts',(5.01586628024736,40.5949139731774,-15.9449210691176));
#53162=CARTESIAN_POINT('Ctrl Pts',(5.0636960184238,40.4590057943956,-15.934253853083));
#53163=CARTESIAN_POINT('Ctrl Pts',(5.10754371538125,40.3212231356076,-15.9248891748567));
#53164=CARTESIAN_POINT('Ctrl Pts',(5.12646876530576,40.2617549336898,-15.9208472977399));
#53165=CARTESIAN_POINT('Ctrl Pts',(5.1446505915391,40.201942005203,-15.9170483417049));
#53166=CARTESIAN_POINT('Ctrl Pts',(5.16211022828596,40.1417848426849,-15.9134952669358));
#53167=CARTESIAN_POINT('Ctrl Pts',(5.16936875516642,40.1167755949256,-15.9120181406304));
#53168=CARTESIAN_POINT('Ctrl Pts',(5.17650218662148,40.0917067297718,-15.9105834629293));
#53169=CARTESIAN_POINT('Ctrl Pts',(5.18351176949454,40.0665781629916,-15.9091914163543));
#53170=CARTESIAN_POINT('Ctrl Pts',(5.18757716154722,40.0520041893995,-15.9083840623097));
#53171=CARTESIAN_POINT('Ctrl Pts',(5.1916022197332,40.0374051221726,-15.9075907944438));
#53172=CARTESIAN_POINT('Ctrl Pts',(5.19558417075906,40.0227922606481,-15.9068122242068));
#53173=CARTESIAN_POINT('Ctrl Pts',(5.19847150744282,40.0121963867007,-15.9062476782363));
#53174=CARTESIAN_POINT('Ctrl Pts',(5.2013361339774,40.0015934265861,-15.9056908682819));
#53175=CARTESIAN_POINT('Ctrl Pts',(5.20417699410974,39.9909876901929,-15.9051420258653));
#53176=CARTESIAN_POINT('Ctrl Pts',(5.20806662989904,39.9764665768945,-15.9043905643337));
#53177=CARTESIAN_POINT('Ctrl Pts',(5.21191164472706,39.9619408105056,-15.9036540441075));
#53178=CARTESIAN_POINT('Ctrl Pts',(5.21571252195769,39.9474103684272,-15.9029324020479));
#53179=CARTESIAN_POINT('Ctrl Pts',(5.22228943303246,39.9222673765261,-15.9016836967186));
#53180=CARTESIAN_POINT('Ctrl Pts',(5.22873447988942,39.8971092606892,-15.9004794946389));
#53181=CARTESIAN_POINT('Ctrl Pts',(5.23505001568631,39.871936285293,-15.8993195153678));
#53182=CARTESIAN_POINT('Ctrl Pts',(5.23777825743765,39.8610618377893,-15.898818417127));
#53183=CARTESIAN_POINT('Ctrl Pts',(5.24048232982734,39.85018461934,-15.8983255720336));
#53184=CARTESIAN_POINT('Ctrl Pts',(5.24316242206404,39.8393046514301,-15.8978409575634));
#53185=CARTESIAN_POINT('Ctrl Pts',(5.25289048130553,39.7998131104588,-15.8960819291946));
#53186=CARTESIAN_POINT('Ctrl Pts',(5.26230280240304,39.7602853708674,-15.8944313398567));
#53187=CARTESIAN_POINT('Ctrl Pts',(5.27140738538964,39.7207223269442,-15.8928881139419));
#53188=CARTESIAN_POINT('Ctrl Pts',(5.28567394755738,39.6587284249165,-15.890469933067));
#53189=CARTESIAN_POINT('Ctrl Pts',(5.29918490214635,39.5966478567417,-15.8883153733681));
#53190=CARTESIAN_POINT('Ctrl Pts',(5.31197079084341,39.5344841787339,-15.8864203519859));
#53191=CARTESIAN_POINT('Ctrl Pts',(5.3408154874063,39.3942442257785,-15.8821452235183));
#53192=CARTESIAN_POINT('Ctrl Pts',(5.36597777759522,39.2535822868239,-15.8791908920713));
#53193=CARTESIAN_POINT('Ctrl Pts',(5.38773152176282,39.1125293717576,-15.8775113110921));
#53194=CARTESIAN_POINT('Ctrl Pts',(5.39764940999791,39.0482210377034,-15.8767455626166));
#53195=CARTESIAN_POINT('Ctrl Pts',(5.40685871578436,38.9838314856836,-15.8762448282014));
#53196=CARTESIAN_POINT('Ctrl Pts',(5.41538504850589,38.9193637310051,-15.8760048072301));
#53197=CARTESIAN_POINT('Ctrl Pts',(5.43385000474362,38.7797498656116,-15.8754850085222));
#53198=CARTESIAN_POINT('Ctrl Pts',(5.44911004070475,38.6397690160481,-15.8761878337851));
#53199=CARTESIAN_POINT('Ctrl Pts',(5.4613515310083,38.4994423268314,-15.8780708774594));
#53200=CARTESIAN_POINT('Ctrl Pts',(5.4672180666783,38.4321930371347,-15.8789732955971));
#53201=CARTESIAN_POINT('Ctrl Pts',(5.47239129984161,38.3648642685655,-15.8801468135981));
#53202=CARTESIAN_POINT('Ctrl Pts',(5.47689147490033,38.2974584401977,-15.8815868411561));
#53203=CARTESIAN_POINT('Ctrl Pts',(5.48611772124094,38.1592631990796,-15.8845391816348));
#53204=CARTESIAN_POINT('Ctrl Pts',(5.49251394881542,38.0207439405754,-15.8886116481605));
#53205=CARTESIAN_POINT('Ctrl Pts',(5.49620058929051,37.8819144998199,-15.893766360599));
#53206=CARTESIAN_POINT('Ctrl Pts',(5.49808097420446,37.8111040186317,-15.8963955411688));
#53207=CARTESIAN_POINT('Ctrl Pts',(5.49925641419002,37.7402128223893,-15.8993062934152));
#53208=CARTESIAN_POINT('Ctrl Pts',(5.49974268802741,37.6692427040055,-15.9024936677521));
#53209=CARTESIAN_POINT('Ctrl Pts',(5.49996561172688,37.6367076998042,-15.9039548635314));
#53210=CARTESIAN_POINT('Ctrl Pts',(5.50004339710141,37.6041560699435,-15.9054742042386));
#53211=CARTESIAN_POINT('Ctrl Pts',(5.49997719383551,37.5715879387439,-15.9070512284576));
#53212=CARTESIAN_POINT('Ctrl Pts',(5.49993631495294,37.5514779216182,-15.9080250019866));
#53213=CARTESIAN_POINT('Ctrl Pts',(5.4998405483016,37.531364539371,-15.9090206118804));
#53214=CARTESIAN_POINT('Ctrl Pts',(5.49969017010503,37.5112446362526,-15.9100381108086));
#53215=CARTESIAN_POINT('Ctrl Pts',(5.49945316022283,37.4795338166206,-15.9116417827945));
#53216=CARTESIAN_POINT('Ctrl Pts',(5.49908009391674,37.4477923382831,-15.9133006740155));
#53217=CARTESIAN_POINT('Ctrl Pts',(5.49857262658559,37.4160475576214,-15.9150128293562));
#53218=CARTESIAN_POINT('Ctrl Pts',(5.49823619185712,37.3950017759391,-15.9161479339861));
#53219=CARTESIAN_POINT('Ctrl Pts',(5.49784081050823,37.373963120172,-15.9173059703468));
#53220=CARTESIAN_POINT('Ctrl Pts',(5.49738703265501,37.3529405554518,-15.9184862796528));
#53221=CARTESIAN_POINT('Ctrl Pts',(5.49672206742468,37.3221341278296,-15.920215902736));
#53222=CARTESIAN_POINT('Ctrl Pts',(5.49593195327599,37.2913564447323,-15.92199354696));
#53223=CARTESIAN_POINT('Ctrl Pts',(5.4950180497321,37.2605988957863,-15.9238189832608));
#53224=CARTESIAN_POINT('Ctrl Pts',(5.49280147822436,37.1859998780916,-15.9282463761961));
#53225=CARTESIAN_POINT('Ctrl Pts',(5.48985732942819,37.1115441622757,-15.93295352956));
#53226=CARTESIAN_POINT('Ctrl Pts',(5.48620799883168,37.0372271498164,-15.9379304121376));
#53227=CARTESIAN_POINT('Ctrl Pts',(5.47973167176091,36.9053395975987,-15.9467626948023));
#53228=CARTESIAN_POINT('Ctrl Pts',(5.47103846329943,36.7738881771258,-15.9564438277391));
#53229=CARTESIAN_POINT('Ctrl Pts',(5.46021917404937,36.6428531857779,-15.9669233415353));
#53230=CARTESIAN_POINT('Ctrl Pts',(5.45380509725103,36.5651707726035,-15.9731359868158));
#53231=CARTESIAN_POINT('Ctrl Pts',(5.44664379103562,36.4876348301111,-15.9796292274412));
#53232=CARTESIAN_POINT('Ctrl Pts',(5.43875405388885,36.4102412795673,-15.9863926024135));
#53233=CARTESIAN_POINT('Ctrl Pts',(5.4258362108228,36.2835250504138,-15.9974662560553));
#53234=CARTESIAN_POINT('Ctrl Pts',(5.41096503287305,36.1571906423008,-16.0092641942867));
#53235=CARTESIAN_POINT('Ctrl Pts',(5.39418796878771,36.0312262694519,-16.0217459585996));
#53236=CARTESIAN_POINT('Ctrl Pts',(5.38340841350248,35.9502919704478,-16.0297657091224));
#53237=CARTESIAN_POINT('Ctrl Pts',(5.37184204285196,35.8695104675066,-16.0380677347448));
#53238=CARTESIAN_POINT('Ctrl Pts',(5.35950133781401,35.7888786668574,-16.0466413856611));
#53239=CARTESIAN_POINT('Ctrl Pts',(5.34090443967194,35.6673700999583,-16.0595614994072));
#53240=CARTESIAN_POINT('Ctrl Pts',(5.32054889691846,35.5462015292645,-16.0730985401622));
#53241=CARTESIAN_POINT('Ctrl Pts',(5.29844924191254,35.4253672803131,-16.0872199870259));
#53242=CARTESIAN_POINT('Ctrl Pts',(5.28302942198048,35.3410563550991,-16.0970730896087));
#53243=CARTESIAN_POINT('Ctrl Pts',(5.26676046322358,35.2569081691998,-16.1072106103974));
#53244=CARTESIAN_POINT('Ctrl Pts',(5.24964719740389,35.1729207936882,-16.1176215804705));
#53245=CARTESIAN_POINT('Ctrl Pts',(5.22595810725155,35.0566610142215,-16.132032997393));
#53246=CARTESIAN_POINT('Ctrl Pts',(5.20065131757863,34.9407093519288,-16.146968454176));
#53247=CARTESIAN_POINT('Ctrl Pts',(5.17371469820154,34.8250650313396,-16.1624016697516));
#53248=CARTESIAN_POINT('Ctrl Pts',(5.15327132250656,34.7372975108614,-16.1741146104059));
#53249=CARTESIAN_POINT('Ctrl Pts',(5.13188915865321,34.6497070193824,-16.186114219127));
#53250=CARTESIAN_POINT('Ctrl Pts',(5.10956274419647,34.5622931135843,-16.1983889759437));
#53251=CARTESIAN_POINT('Ctrl Pts',(5.08367992517983,34.4609549292693,-16.212618995268));
#53252=CARTESIAN_POINT('Ctrl Pts',(5.0565259540986,34.3598544368731,-16.2272190066503));
#53253=CARTESIAN_POINT('Ctrl Pts',(5.0280786240926,34.258993325232,-16.2421722431811));
#53254=CARTESIAN_POINT('Ctrl Pts',(5.02537462849238,34.2494062039783,-16.2435935887267));
#53255=CARTESIAN_POINT('Ctrl Pts',(5.02265894191753,34.2398212464829,-16.245018126109));
#53256=CARTESIAN_POINT('Ctrl Pts',(5.01993153885963,34.2302384553135,-16.246445841369));
#53257=CARTESIAN_POINT('Ctrl Pts',(5.00830961335107,34.18940456213,-16.2525295774528));
#53258=CARTESIAN_POINT('Ctrl Pts',(4.99647652389308,34.1486153304945,-16.2586702191085));
#53259=CARTESIAN_POINT('Ctrl Pts',(4.98442562639818,34.1078551593912,-16.2648690928362));
#53260=CARTESIAN_POINT('Ctrl Pts',(4.98191519828605,34.0993640507882,-16.2661604345703));
#53261=CARTESIAN_POINT('Ctrl Pts',(4.97939577749796,34.0908757952992,-16.2674540642285));
#53262=CARTESIAN_POINT('Ctrl Pts',(4.97686741013458,34.082390567841,-16.2687499417094));
#53263=CARTESIAN_POINT('Ctrl Pts',(4.96441142163706,34.0405881394636,-16.2751340752931));
#53264=CARTESIAN_POINT('Ctrl Pts',(4.95174642038967,33.9988861356218,-16.2815686233584));
#53265=CARTESIAN_POINT('Ctrl Pts',(4.93887533693539,33.9572960334576,-16.2880501468107));
#53266=CARTESIAN_POINT('Ctrl Pts',(4.9365923183524,33.9499189562716,-16.289199812147));
#53267=CARTESIAN_POINT('Ctrl Pts',(4.93430269704837,33.9425449476634,-16.2903510225307));
#53268=CARTESIAN_POINT('Ctrl Pts',(4.93200641902833,33.9351738636263,-16.2915037921635));
#53269=CARTESIAN_POINT('Ctrl Pts',(4.90152218935013,33.8373190669505,-16.3068073808168));
#53270=CARTESIAN_POINT('Ctrl Pts',(4.86988434782216,33.7400428634163,-16.3223755709518));
#53271=CARTESIAN_POINT('Ctrl Pts',(4.83707663711256,33.6433485724266,-16.3381886662497));
#53272=CARTESIAN_POINT('Ctrl Pts',(4.80536763875374,33.5498925205417,-16.3534721896045));
#53273=CARTESIAN_POINT('Ctrl Pts',(4.77256571792549,33.4569804742511,-16.3689838092686));
#53274=CARTESIAN_POINT('Ctrl Pts',(4.73865560426316,33.3646155432662,-16.3847048733899));
#53275=CARTESIAN_POINT('Ctrl Pts',(4.70239552922545,33.2658497484442,-16.4015154028498));
#53276=CARTESIAN_POINT('Ctrl Pts',(4.66486875936597,33.1677093269555,-16.4185655478469));
#53277=CARTESIAN_POINT('Ctrl Pts',(4.62603635930902,33.0702085181134,-16.4358333229825));
#53278=CARTESIAN_POINT('Ctrl Pts',(4.58826245515966,32.9753653922111,-16.4526304120599));
#53279=CARTESIAN_POINT('Ctrl Pts',(4.54925308469861,32.8811275612641,-16.4696332423119));
#53280=CARTESIAN_POINT('Ctrl Pts',(4.50897156414357,32.7875075156098,-16.4868216505679));
#53281=CARTESIAN_POINT('Ctrl Pts',(4.46911625428267,32.6948780448914,-16.5038281917218));
#53282=CARTESIAN_POINT('Ctrl Pts',(4.42801637606486,32.602852958373,-16.5210165527185));
#53283=CARTESIAN_POINT('Ctrl Pts',(4.38561383431928,32.5114558651078,-16.5383669400771));
#53284=CARTESIAN_POINT('Ctrl Pts',(4.34125546095837,32.415843049926,-16.5565176199356));
#53285=CARTESIAN_POINT('Ctrl Pts',(4.29547149890815,32.3209175705842,-16.5748455228508));
#53286=CARTESIAN_POINT('Ctrl Pts',(4.24819390138341,32.2267055569911,-16.5933281017443));
#53287=CARTESIAN_POINT('Ctrl Pts',(4.20460210136336,32.1398383837197,-16.6103697647129));
#53288=CARTESIAN_POINT('Ctrl Pts',(4.15974189040682,32.0535770633788,-16.6275431186279));
#53289=CARTESIAN_POINT('Ctrl Pts',(4.11353180757193,31.9679563275417,-16.6448290878375));
#53290=CARTESIAN_POINT('Ctrl Pts',(4.06536813475078,31.8787158662706,-16.6628458433664));
#53291=CARTESIAN_POINT('Ctrl Pts',(4.01573942477214,31.7901709205017,-16.6809872025155));
#53292=CARTESIAN_POINT('Ctrl Pts',(3.96454901579434,31.7023606031743,-16.6992276878768));
#53293=CARTESIAN_POINT('Ctrl Pts',(3.96088789420439,31.6960804375142,-16.7005322415247));
#53294=CARTESIAN_POINT('Ctrl Pts',(3.95721878771191,31.6898040285205,-16.7018373092452));
#53295=CARTESIAN_POINT('Ctrl Pts',(3.95354166156699,31.6835313901512,-16.7031428835095));
#53296=CARTESIAN_POINT('Ctrl Pts',(3.90580460039334,31.6020989590209,-16.720092065034));
#53297=CARTESIAN_POINT('Ctrl Pts',(3.85671222537039,31.5213038976113,-16.7371264023128));
#53298=CARTESIAN_POINT('Ctrl Pts',(3.80616156422669,31.4411903127911,-16.7542275028122));
#53299=CARTESIAN_POINT('Ctrl Pts',(3.80152842925821,31.4338476382764,-16.755794875126));
#53300=CARTESIAN_POINT('Ctrl Pts',(3.79688303941635,31.4265106877601,-16.7573628044737));
#53301=CARTESIAN_POINT('Ctrl Pts',(3.79222531430233,31.4191794949343,-16.7589312766305));
#53302=CARTESIAN_POINT('Ctrl Pts',(3.76951630087782,31.3834358320465,-16.7665784551122));
#53303=CARTESIAN_POINT('Ctrl Pts',(3.74651379434752,31.3478291722543,-16.7742385163404));
#53304=CARTESIAN_POINT('Ctrl Pts',(3.72320690339818,31.3123642118345,-16.7819096840143));
#53305=CARTESIAN_POINT('Ctrl Pts',(3.71807526776141,31.304555651905,-16.7835986968259));
#53306=CARTESIAN_POINT('Ctrl Pts',(3.71292915379114,31.2967543834909,-16.7852881565976));
#53307=CARTESIAN_POINT('Ctrl Pts',(3.70776825174835,31.2889601585938,-16.7869781081522));
#53308=CARTESIAN_POINT('Ctrl Pts',(3.69880543936009,31.2754241187919,-16.789913005696));
#53309=CARTESIAN_POINT('Ctrl Pts',(3.68979574239286,31.261906155841,-16.7928500917675));
#53310=CARTESIAN_POINT('Ctrl Pts',(3.68074182945706,31.2484112412283,-16.7957882205531));
#53311=CARTESIAN_POINT('Ctrl Pts',(3.66647455761765,31.2271457821284,-16.8004181614838));
#53312=CARTESIAN_POINT('Ctrl Pts',(3.65209323029816,31.2059313524667,-16.8050520521899));
#53313=CARTESIAN_POINT('Ctrl Pts',(3.63762484959751,31.1848118870779,-16.8096800639383));
#53314=CARTESIAN_POINT('Ctrl Pts',(3.63200035761215,31.1766018277581,-16.8114791743934));
#53315=CARTESIAN_POINT('Ctrl Pts',(3.62636141820263,31.1684042483615,-16.8132777791051));
#53316=CARTESIAN_POINT('Ctrl Pts',(3.62070890280921,31.1602206821355,-16.8150755350487));
#53317=CARTESIAN_POINT('Ctrl Pts',(3.5681995469857,31.0841989889676,-16.8317758887778));
#53318=CARTESIAN_POINT('Ctrl Pts',(3.51445248319197,31.0092691764222,-16.8484279478469));
#53319=CARTESIAN_POINT('Ctrl Pts',(3.45940003185614,30.9355222948858,-16.8650025248823));
#53320=CARTESIAN_POINT('Ctrl Pts',(3.39842130654987,30.8538367255372,-16.8833613182801));
#53321=CARTESIAN_POINT('Ctrl Pts',(3.33583572143396,30.7735927411555,-16.9016283924899));
#53322=CARTESIAN_POINT('Ctrl Pts',(3.2715207048759,30.6948919828411,-16.919757436288));
#53323=CARTESIAN_POINT('Ctrl Pts',(3.26416317733215,30.6858887511232,-16.921831367793));
#53324=CARTESIAN_POINT('Ctrl Pts',(3.25678303217922,30.6769057057008,-16.923903524439));
#53325=CARTESIAN_POINT('Ctrl Pts',(3.24938008678968,30.667942991644,-16.9259738497194));
#53326=CARTESIAN_POINT('Ctrl Pts',(3.19207100052512,30.5985591280577,-16.9420010448216));
#53327=CARTESIAN_POINT('Ctrl Pts',(3.13339174267546,30.5303974813926,-16.9579178841127));
#53328=CARTESIAN_POINT('Ctrl Pts',(3.07322940139954,30.4635532861489,-16.9736929964154));
#53329=CARTESIAN_POINT('Ctrl Pts',(3.06515238212777,30.4545792029975,-16.9758108642274));
#53330=CARTESIAN_POINT('Ctrl Pts',(3.05704861784992,30.4456288810808,-16.9779261567944));
#53331=CARTESIAN_POINT('Ctrl Pts',(3.0489178282833,30.4367025507343,-16.9800387987298));
#53332=CARTESIAN_POINT('Ctrl Pts',(2.98866251080745,30.3705516727029,-16.9956950778016));
#53333=CARTESIAN_POINT('Ctrl Pts',(2.92692378235327,30.3057176256009,-17.0112059694983));
#53334=CARTESIAN_POINT('Ctrl Pts',(2.86356125520061,30.242320131431,-17.026535619822));
#53335=CARTESIAN_POINT('Ctrl Pts',(2.85491055641671,30.2336646587035,-17.028628531727));
#53336=CARTESIAN_POINT('Ctrl Pts',(2.84622956753871,30.2250359814179,-17.0307180375992));
#53337=CARTESIAN_POINT('Ctrl Pts',(2.83751792073732,30.2164344038661,-17.0328040472932));
#53338=CARTESIAN_POINT('Ctrl Pts',(2.77381031096406,30.1535317221342,-17.0480588773613));
#53339=CARTESIAN_POINT('Ctrl Pts',(2.70846431693196,30.0920771826219,-17.0631269955375));
#53340=CARTESIAN_POINT('Ctrl Pts',(2.64130079839515,30.0322245558024,-17.0779660058408));
#53341=CARTESIAN_POINT('Ctrl Pts',(2.63227265442548,30.0241791444889,-17.0799606708658));
#53342=CARTESIAN_POINT('Ctrl Pts',(2.62321161946429,30.0161626708754,-17.0819511802079));
#53343=CARTESIAN_POINT('Ctrl Pts',(2.61411725538389,30.0081755240293,-17.0839374247674));
#53344=CARTESIAN_POINT('Ctrl Pts',(2.57585134947034,29.9745684013068,-17.0922948477565));
#53345=CARTESIAN_POINT('Ctrl Pts',(2.53699459987065,29.9414812576612,-17.1005766119967));
#53346=CARTESIAN_POINT('Ctrl Pts',(2.49750822445488,29.9089491590999,-17.1087733255147));
#53347=CARTESIAN_POINT('Ctrl Pts',(2.47779485825612,29.8927076792123,-17.1128654918254));
#53348=CARTESIAN_POINT('Ctrl Pts',(2.45792448501533,29.8766046168504,-17.1169364445262));
#53349=CARTESIAN_POINT('Ctrl Pts',(2.43789178185496,29.8606448267007,-17.1209849104469));
#53350=CARTESIAN_POINT('Ctrl Pts',(2.42694070914223,29.8519202516391,-17.1231980438576));
#53351=CARTESIAN_POINT('Ctrl Pts',(2.41593835595827,29.8432363635108,-17.1254050014128));
#53352=CARTESIAN_POINT('Ctrl Pts',(2.40488856363168,29.8345976778537,-17.1276046266254));
#53353=CARTESIAN_POINT('Ctrl Pts',(2.39574786529823,29.8274515146267,-17.1294242183354));
#53354=CARTESIAN_POINT('Ctrl Pts',(2.38657107919022,29.8203334707193,-17.131239509796));
#53355=CARTESIAN_POINT('Ctrl Pts',(2.37736544561913,29.8132500786786,-17.1330488320748));
#53356=CARTESIAN_POINT('Ctrl Pts',(2.37632716664283,29.8124511616915,-17.1332529007323));
#53357=CARTESIAN_POINT('Ctrl Pts',(2.37528863153933,29.8116527691013,-17.1334568720052));
#53358=CARTESIAN_POINT('Ctrl Pts',(2.3742498473769,29.8108549069625,-17.133660744308));
#53359=CARTESIAN_POINT('Ctrl Pts',(2.36400095054056,29.8029830053244,-17.1356721979616));
#53360=CARTESIAN_POINT('Ctrl Pts',(2.35372330622806,29.7951592975047,-17.1376748836086));
#53361=CARTESIAN_POINT('Ctrl Pts',(2.34341659203281,29.7873843072001,-17.1396686375351));
#53362=CARTESIAN_POINT('Ctrl Pts',(2.32280316364232,29.7718343265909,-17.1436561453881));
#53363=CARTESIAN_POINT('Ctrl Pts',(2.30207345556508,29.7564792140062,-17.1476079243563));
#53364=CARTESIAN_POINT('Ctrl Pts',(2.28122498144331,29.7413230169235,-17.1515229111162));
#53365=CARTESIAN_POINT('Ctrl Pts',(2.23952803319974,29.7110106227581,-17.1593528846361));
#53366=CARTESIAN_POINT('Ctrl Pts',(2.19735604974939,29.6814938543918,-17.1670356542043));
#53367=CARTESIAN_POINT('Ctrl Pts',(2.15468743215846,29.6528077790857,-17.1745600211926));
#53368=CARTESIAN_POINT('Ctrl Pts',(2.14610634444727,29.6470387211178,-17.1760732469952));
#53369=CARTESIAN_POINT('Ctrl Pts',(2.13750517566442,29.6413032676407,-17.1775800661172));
#53370=CARTESIAN_POINT('Ctrl Pts',(2.12888374364691,29.6356017004686,-17.1790803938992));
#53371=CARTESIAN_POINT('Ctrl Pts',(2.05176672426468,29.5846022997628,-17.1925005318074));
#53372=CARTESIAN_POINT('Ctrl Pts',(1.97302948507885,29.536311980985,-17.2054018294005));
#53373=CARTESIAN_POINT('Ctrl Pts',(1.892517709225,29.4909836117988,-17.2177138548144));
#53374=CARTESIAN_POINT('Ctrl Pts',(1.88526198991242,29.4868986202528,-17.2188234142499));
#53375=CARTESIAN_POINT('Ctrl Pts',(1.87799185081891,29.4828377056425,-17.2199281748248));
#53376=CARTESIAN_POINT('Ctrl Pts',(1.87070717006779,29.4788010572599,-17.2210280840153));
#53377=CARTESIAN_POINT('Ctrl Pts',(1.78812182725007,29.4330381745882,-17.2334975910074));
#53378=CARTESIAN_POINT('Ctrl Pts',(1.70366911987935,29.3903907672498,-17.2453443608244));
#53379=CARTESIAN_POINT('Ctrl Pts',(1.61713745716078,29.3512072939032,-17.2564775264755));
#53380=CARTESIAN_POINT('Ctrl Pts',(1.61212632952938,29.3489381431691,-17.2571222582681));
#53381=CARTESIAN_POINT('Ctrl Pts',(1.60710821712393,29.3466806272549,-17.2577645818538));
#53382=CARTESIAN_POINT('Ctrl Pts',(1.60208307676273,29.3444348146711,-17.2584044808196));
#53383=CARTESIAN_POINT('Ctrl Pts',(1.55989433998816,29.3255800187584,-17.2637767743458));
#53384=CARTESIAN_POINT('Ctrl Pts',(1.51721051394536,29.3075495812703,-17.2689782885513));
#53385=CARTESIAN_POINT('Ctrl Pts',(1.47400118885662,29.2903942144724,-17.2739973129508));
#53386=CARTESIAN_POINT('Ctrl Pts',(1.46191218168413,29.2855945247794,-17.2754015242371));
#53387=CARTESIAN_POINT('Ctrl Pts',(1.4497820516811,29.2808633184437,-17.2767914781327));
#53388=CARTESIAN_POINT('Ctrl Pts',(1.43761008083042,29.2762017723702,-17.2781668632123));
#53389=CARTESIAN_POINT('Ctrl Pts',(1.42543810997977,29.2715402262967,-17.2795422482919));
#53390=CARTESIAN_POINT('Ctrl Pts',(1.41321940491667,29.2669465835128,-17.280903591134));
#53391=CARTESIAN_POINT('Ctrl Pts',(1.40097815995123,29.2624310609538,-17.2822478952774));
#53392=CARTESIAN_POINT('Ctrl Pts',(1.37649567002035,29.2534000158358,-17.2849365035642));
#53393=CARTESIAN_POINT('Ctrl Pts',(1.35191025614907,29.2446764670801,-17.2875582881031));
#53394=CARTESIAN_POINT('Ctrl Pts',(1.32722006320831,29.2362657864039,-17.2901114789568));
#53395=CARTESIAN_POINT('Ctrl Pts',(1.32550120392183,29.2356802593236,-17.2902892246641));
#53396=CARTESIAN_POINT('Ctrl Pts',(1.32378183755517,29.2350962472779,-17.29046663934));
#53397=CARTESIAN_POINT('Ctrl Pts',(1.3220619635894,29.2345137519665,-17.2906437224965));
#53398=CARTESIAN_POINT('Ctrl Pts',(1.27437230137859,29.2183619843406,-17.2955539869008));
#53399=CARTESIAN_POINT('Ctrl Pts',(1.22629149643725,29.2033782518924,-17.3002089905994));
#53400=CARTESIAN_POINT('Ctrl Pts',(1.17780400163588,29.1896084456524,-17.3045965622765));
#53401=CARTESIAN_POINT('Ctrl Pts',(1.17767327582233,29.189571321253,-17.3046083914889));
#53402=CARTESIAN_POINT('Ctrl Pts',(1.17754254712066,29.189534205695,-17.3046202187513));
#53403=CARTESIAN_POINT('Ctrl Pts',(1.17741181552952,29.1894970989791,-17.3046320440637));
#53404=CARTESIAN_POINT('Ctrl Pts',(1.15299541258929,29.1825667731042,-17.3068406272224));
#53405=CARTESIAN_POINT('Ctrl Pts',(1.12847817746668,29.1759449661951,-17.3089811700638));
#53406=CARTESIAN_POINT('Ctrl Pts',(1.10385096834405,29.1696362782663,-17.311052643283));
#53407=CARTESIAN_POINT('Ctrl Pts',(1.10327398297119,29.1694884734282,-17.3111011753656));
#53408=CARTESIAN_POINT('Ctrl Pts',(1.10269696617672,29.1693408482817,-17.3111496670085));
#53409=CARTESIAN_POINT('Ctrl Pts',(1.10211991879364,29.1691934030318,-17.3111981181411));
#53410=CARTESIAN_POINT('Ctrl Pts',(1.0780259363015,29.1630369878481,-17.3132211422025));
#53411=CARTESIAN_POINT('Ctrl Pts',(1.05386293703712,29.1571899569309,-17.3151748891896));
#53412=CARTESIAN_POINT('Ctrl Pts',(1.02966713626784,29.1516639253954,-17.3170555760385));
#53413=CARTESIAN_POINT('Ctrl Pts',(1.02841708067243,29.1513784276469,-17.3171527401349));
#53414=CARTESIAN_POINT('Ctrl Pts',(1.02716688202533,29.1510937723588,-17.317249713827));
#53415=CARTESIAN_POINT('Ctrl Pts',(1.0259165361847,29.1508099590767,-17.3173464973055));
#53416=CARTESIAN_POINT('Ctrl Pts',(0.928167679757507,29.1286221588217,-17.3249127833967));
#53417=CARTESIAN_POINT('Ctrl Pts',(0.829681073359833,29.1116166132758,-17.3313043848515));
#53418=CARTESIAN_POINT('Ctrl Pts',(0.730430567978592,29.099973605139,-17.3364718005591));
#53419=CARTESIAN_POINT('',(0.346147593750904,43.9243235319994,-16.6433959640037));
#53420=CARTESIAN_POINT('Origin',(0.600919835348839,39.755200147935,-15.5793615221956));
#53421=CARTESIAN_POINT('Origin',(0.330762353100779,44.2777095070772,-16.996781938525));
#53422=CARTESIAN_POINT('Origin',(9.,24.,-29.5));
#53423=CARTESIAN_POINT('',(9.,26.1794494717703,-23.3762756430421));
#53424=CARTESIAN_POINT('',(8.9999999999999,26.1794494717706,-35.6237243569579));
#53425=CARTESIAN_POINT('Origin',(9.,24.,-29.5));
#53426=CARTESIAN_POINT('',(9.5,26.0117995124034,-23.847331362808));
#53427=CARTESIAN_POINT('Origin',(9.,26.0117995124034,-23.847331362808));
#53428=CARTESIAN_POINT('',(9.5,26.0117995124036,-35.1526686371918));
#53429=CARTESIAN_POINT('Origin',(9.5,24.,-29.5));
#53430=CARTESIAN_POINT('Origin',(9.,26.0117995124036,-35.1526686371918));
#53431=CARTESIAN_POINT('Origin',(-42.5,41.0197988065678,-24.9401265742657));
#53432=CARTESIAN_POINT('',(-44.9819347291981,45.7897031282913,-29.7473377789847));
#53433=CARTESIAN_POINT('',(-44.9819347291981,47.3983418014005,-27.2150894461039));
#53434=CARTESIAN_POINT('Origin',(-42.5,46.5940224648459,-28.4812136125442));
#53435=CARTESIAN_POINT('',(-45.2221315177632,45.635768184996,-29.057189944653));
#53436=CARTESIAN_POINT('Ctrl Pts',(-44.9819347291982,45.7897031282913,-29.7473377789846));
#53437=CARTESIAN_POINT('Ctrl Pts',(-45.0186376354568,45.8222670575131,-29.6960770721134));
#53438=CARTESIAN_POINT('Ctrl Pts',(-45.0556916549072,45.8482062072712,-29.6333175979576));
#53439=CARTESIAN_POINT('Ctrl Pts',(-45.1195835420918,45.8719268666396,-29.4987828001409));
#53440=CARTESIAN_POINT('Ctrl Pts',(-45.1465267698371,45.8695622104315,-29.4270318030083));
#53441=CARTESIAN_POINT('Ctrl Pts',(-45.1843416183679,45.8393623668559,-29.3030188626678));
#53442=CARTESIAN_POINT('Ctrl Pts',(-45.1988644063568,45.8129304583389,-29.2426178063836));
#53443=CARTESIAN_POINT('Ctrl Pts',(-45.2176939546586,45.7373723936762,-29.1363548938651));
#53444=CARTESIAN_POINT('Ctrl Pts',(-45.2221315177632,45.6882381055569,-29.0905220402035));
#53445=CARTESIAN_POINT('Ctrl Pts',(-45.2221315177632,45.635768184996,-29.0571899446529));
#53446=CARTESIAN_POINT('',(-45.2221315177632,43.1035198521152,-27.4485512715437));
#53447=CARTESIAN_POINT('',(-45.2221315177632,40.4835859155314,-25.7842093518926));
#53448=CARTESIAN_POINT('',(-44.9819347291981,42.4133720177836,-27.602486214839));
#53449=CARTESIAN_POINT('Ctrl Pts',(-45.2221315177632,43.1035198521152,-27.4485512715437));
#53450=CARTESIAN_POINT('Ctrl Pts',(-45.2221315177632,43.0496138985403,-27.4143069201879));
#53451=CARTESIAN_POINT('Ctrl Pts',(-45.2174539674018,42.9854710022637,-27.3889839513675));
#53452=CARTESIAN_POINT('Ctrl Pts',(-45.1976418506297,42.8537496937191,-27.3664815814561));
#53453=CARTESIAN_POINT('Ctrl Pts',(-45.182361508012,42.7861963762066,-27.3692838789625));
#53454=CARTESIAN_POINT('Ctrl Pts',(-45.1436039433344,42.6618963628359,-27.3970085410682));
#53455=CARTESIAN_POINT('Ctrl Pts',(-45.1169018514096,42.5979765578451,-27.4255404391954));
#53456=CARTESIAN_POINT('Ctrl Pts',(-45.0540257957218,42.4896281746961,-27.5033321310102));
#53457=CARTESIAN_POINT('Ctrl Pts',(-45.0177578429344,42.4451553684532,-27.5524542604343));
#53458=CARTESIAN_POINT('Ctrl Pts',(-44.9819347291981,42.4133720177835,-27.602486214839));
#53459=CARTESIAN_POINT('',(-44.9819347291981,44.0220106908928,-25.0702378819582));
#53460=CARTESIAN_POINT('Origin',(-42.5,43.2176913543382,-26.3363620483986));
#53461=CARTESIAN_POINT('',(-45.2221315177632,44.1759456341881,-25.7603857162899));
#53462=CARTESIAN_POINT('Ctrl Pts',(-44.9819347291982,44.0220106908928,-25.0702378819583));
#53463=CARTESIAN_POINT('Ctrl Pts',(-45.0186376354568,43.989446761671,-25.1214985888295));
#53464=CARTESIAN_POINT('Ctrl Pts',(-45.0556916549072,43.963507611913,-25.1842580629853));
#53465=CARTESIAN_POINT('Ctrl Pts',(-45.1195835420918,43.9397869525445,-25.318792860802));
#53466=CARTESIAN_POINT('Ctrl Pts',(-45.1465267698372,43.9421516087526,-25.3905438579346));
#53467=CARTESIAN_POINT('Ctrl Pts',(-45.1843416183679,43.9723514523282,-25.5145567982751));
#53468=CARTESIAN_POINT('Ctrl Pts',(-45.1988644063568,43.9987833608452,-25.5749578545593));
#53469=CARTESIAN_POINT('Ctrl Pts',(-45.2176939546586,44.0743414255079,-25.6812207670778));
#53470=CARTESIAN_POINT('Ctrl Pts',(-45.2221315177633,44.1234757136272,-25.7270536207394));
#53471=CARTESIAN_POINT('Ctrl Pts',(-45.2221315177633,44.1759456341881,-25.76038571629));
#53472=CARTESIAN_POINT('',(-45.2221315177632,46.7081939670689,-27.3690243893992));
#53473=CARTESIAN_POINT('',(-45.2221315177632,41.5560116976042,-24.0960437966388));
#53474=CARTESIAN_POINT('Ctrl Pts',(-45.2221315177632,46.7081939670689,-27.3690243893992));
#53475=CARTESIAN_POINT('Ctrl Pts',(-45.2221315177632,46.7606638876298,-27.4023564849497));
#53476=CARTESIAN_POINT('Ctrl Pts',(-45.2176939546586,46.8230322141941,-27.427356896653));
#53477=CARTESIAN_POINT('Ctrl Pts',(-45.1988644063568,46.9513316276602,-27.4505966947741));
#53478=CARTESIAN_POINT('Ctrl Pts',(-45.1843416183679,47.0172399166597,-27.4488557670715));
#53479=CARTESIAN_POINT('Ctrl Pts',(-45.1465267698371,47.1423318988987,-27.4234936712708));
#53480=CARTESIAN_POINT('Ctrl Pts',(-45.1195835420918,47.208286923191,-27.3951435044439));
#53481=CARTESIAN_POINT('Ctrl Pts',(-45.0556916549071,47.3199898635242,-27.3165004206706));
#53482=CARTESIAN_POINT('Ctrl Pts',(-45.0186376354568,47.3657778721787,-27.2663501529751));
#53483=CARTESIAN_POINT('Ctrl Pts',(-44.9819347291982,47.3983418014006,-27.2150894461039));
#53484=CARTESIAN_POINT('Origin',(-50.,46.9763004125871,-26.9469830005857));
#53485=CARTESIAN_POINT('',(-50.,46.7081939670689,-27.3690243893992));
#53486=CARTESIAN_POINT('',(-45.2221315177632,46.7081939670689,-27.3690243893992));
#53487=CARTESIAN_POINT('',(-49.5,47.3983418014005,-27.2150894461039));
#53488=CARTESIAN_POINT('Origin',(-49.5000000000004,46.9763004125864,-26.9469830005858));
#53489=CARTESIAN_POINT('',(-50.,47.3983418014005,-27.2150894461039));
#53490=CARTESIAN_POINT('Origin',(0.,12.,0.));
#53491=CARTESIAN_POINT('',(2.38806125833734E-15,12.,19.5));
#53492=CARTESIAN_POINT('Origin',(6.61325378140121E-15,20.5440037453176,
8.67361737988404E-16));
#53493=CARTESIAN_POINT('Ctrl Pts',(-12.9440892692056,20.5440037453176,10.2323288156136));
#53494=CARTESIAN_POINT('Ctrl Pts',(-12.9496367646674,20.4508539796772,10.2253111290467));
#53495=CARTESIAN_POINT('Ctrl Pts',(-12.9610165600406,20.3590140095801,10.2178819495937));
#53496=CARTESIAN_POINT('Ctrl Pts',(-12.9946219649296,20.1777741261809,10.2022098463961));
#53497=CARTESIAN_POINT('Ctrl Pts',(-13.0168498220794,20.0883747060241,10.1939668938316));
#53498=CARTESIAN_POINT('Ctrl Pts',(-13.0579271737774,19.9560174404499,10.1810048619498));
#53499=CARTESIAN_POINT('Ctrl Pts',(-13.0729108743488,19.912189091234,10.1765846465299));
#53500=CARTESIAN_POINT('Ctrl Pts',(-13.093226641434,19.857760815908,10.1709368410215));
#53501=CARTESIAN_POINT('Ctrl Pts',(-13.0973704642225,19.846889820709,10.1698008100038));
#53502=CARTESIAN_POINT('Ctrl Pts',(-13.1057990120293,19.8252268576759,10.1675211517166));
#53503=CARTESIAN_POINT('Ctrl Pts',(-13.1186586370485,19.7928359778532,10.1640887306089));
#53504=CARTESIAN_POINT('Ctrl Pts',(-13.1681680547971,19.6751954927419,10.1513630815639));
#53505=CARTESIAN_POINT('Ctrl Pts',(-13.2201296869753,19.5715707888266,10.1393814591848));
#53506=CARTESIAN_POINT('Ctrl Pts',(-13.2658111744658,19.4906334205523,10.1295681579593));
#53507=CARTESIAN_POINT('',(12.2613197119475,20.1060921583966,11.0892507440724));
#53508=CARTESIAN_POINT('Ctrl Pts',(12.3247145835032,19.4906334206159,11.2557233274532));
#53509=CARTESIAN_POINT('Ctrl Pts',(12.3240848130916,19.4937421807176,11.2546841768212));
#53510=CARTESIAN_POINT('Ctrl Pts',(12.3234588554608,19.49685286589,11.2536485098443));
#53511=CARTESIAN_POINT('Ctrl Pts',(12.3228366936365,19.4999654675381,11.252616310886));
#53512=CARTESIAN_POINT('Ctrl Pts',(12.3222145318121,19.5030780691863,11.2515841119277));
#53513=CARTESIAN_POINT('Ctrl Pts',(12.3215948199724,19.5062100227993,11.2505473287028));
#53514=CARTESIAN_POINT('Ctrl Pts',(12.320980850292,19.5093388049001,11.2495147887444));
#53515=CARTESIAN_POINT('Ctrl Pts',(12.3197529109312,19.5155963691016,11.2474497088275));
#53516=CARTESIAN_POINT('Ctrl Pts',(12.3185447508262,19.5218607187377,11.2453943141538));
#53517=CARTESIAN_POINT('Ctrl Pts',(12.3173562624689,19.5281318609459,11.2433486881666));
#53518=CARTESIAN_POINT('Ctrl Pts',(12.3168434298913,19.5308378580248,11.2424660008089));
#53519=CARTESIAN_POINT('Ctrl Pts',(12.3163342607863,19.5335451203528,11.2415851313079));
#53520=CARTESIAN_POINT('Ctrl Pts',(12.3158287470122,19.5362536487047,11.240706086076));
#53521=CARTESIAN_POINT('Ctrl Pts',(12.3139912066935,19.5460991372083,11.2375107605708));
#53522=CARTESIAN_POINT('Ctrl Pts',(12.3122019380873,19.5559613346833,11.2343395764923));
#53523=CARTESIAN_POINT('Ctrl Pts',(12.3104605724095,19.5658402918111,11.2311928321139));
#53524=CARTESIAN_POINT('Ctrl Pts',(12.3060197294663,19.5910336774419,11.2231679825694));
#53525=CARTESIAN_POINT('Ctrl Pts',(12.3018924452675,19.6163256808546,11.2153056087511));
#53526=CARTESIAN_POINT('Ctrl Pts',(12.2980766065538,19.6416802262003,11.2076214964828));
#53527=CARTESIAN_POINT('Ctrl Pts',(12.2904449291265,19.6923893168918,11.1922532719461));
#53528=CARTESIAN_POINT('Ctrl Pts',(12.284050670942,19.7433903721453,11.1775842317797));
#53529=CARTESIAN_POINT('Ctrl Pts',(12.2788349799084,19.7946878523301,11.1636514510574));
#53530=CARTESIAN_POINT('Ctrl Pts',(12.2717832670323,19.864043015281,11.144814068132));
#53531=CARTESIAN_POINT('Ctrl Pts',(12.2668823557172,19.933938143891,11.1273231458003));
#53532=CARTESIAN_POINT('Ctrl Pts',(12.2640266900014,20.0043963659391,11.1112869549714));
#53533=CARTESIAN_POINT('Ctrl Pts',(12.2626580572155,20.0381648256718,11.1036013017073));
#53534=CARTESIAN_POINT('Ctrl Pts',(12.26175954294,20.0720626786387,11.0962505061429));
#53535=CARTESIAN_POINT('Ctrl Pts',(12.2613198608839,20.1060920634664,11.0892508104087));
#53536=CARTESIAN_POINT('Ctrl Pts',(12.2613195356308,20.1060921539105,11.0892505197455));
#53537=CARTESIAN_POINT('Ctrl Pts',(12.2392211623119,20.1414234900087,11.1059128816441));
#53538=CARTESIAN_POINT('Ctrl Pts',(12.2176741954609,20.1770688828304,11.122757035389));
#53539=CARTESIAN_POINT('Ctrl Pts',(12.1967039557601,20.2130404789298,11.1397962358671));
#53540=CARTESIAN_POINT('Ctrl Pts',(12.1862188142041,20.2310263142123,11.1483158537427));
#53541=CARTESIAN_POINT('Ctrl Pts',(12.1758744707651,20.249099975504,11.1568872553953));
#53542=CARTESIAN_POINT('Ctrl Pts',(12.1656907253532,20.267233703068,11.1654983955483));
#53543=CARTESIAN_POINT('Ctrl Pts',(12.1555069799413,20.2853674306321,11.1741095357013));
#53544=CARTESIAN_POINT('Ctrl Pts',(12.1454820134063,20.30356413516,11.1827617704007));
#53545=CARTESIAN_POINT('Ctrl Pts',(12.1356187555891,20.3218245820165,11.1914566941426));
#53546=CARTESIAN_POINT('Ctrl Pts',(12.125569551754,20.3404292820032,11.2003155380087));
#53547=CARTESIAN_POINT('Ctrl Pts',(12.1156883444925,20.3591001188471,11.2092185790426));
#53548=CARTESIAN_POINT('Ctrl Pts',(12.1059782546267,20.3778380797799,11.2181678242057));
#53549=CARTESIAN_POINT('Ctrl Pts',(12.0966275071673,20.395882602849,11.2267858836294));
#53550=CARTESIAN_POINT('Ctrl Pts',(12.0874354743147,20.4139893872255,11.2354467144436));
#53551=CARTESIAN_POINT('Ctrl Pts',(12.0784054764407,20.432159179516,11.2441518495297));
#53552=CARTESIAN_POINT('Ctrl Pts',(12.0692019704499,20.4506780977408,11.2530242506126));
#53553=CARTESIAN_POINT('Ctrl Pts',(12.0601666863676,20.4692625077711,11.261942764992));
#53554=CARTESIAN_POINT('Ctrl Pts',(12.0513032693893,20.4879134104374,11.2709092728905));
#53555=CARTESIAN_POINT('Ctrl Pts',(12.0468715609001,20.4972388617706,11.2753925268398));
#53556=CARTESIAN_POINT('Ctrl Pts',(12.0424826470527,20.5065813207882,11.2798879696857));
#53557=CARTESIAN_POINT('Ctrl Pts',(12.0381381742578,20.5159383696529,11.2843946238478));
#53558=CARTESIAN_POINT('Ctrl Pts',(12.0359659378604,20.5206168940852,11.2866479509288));
#53559=CARTESIAN_POINT('Ctrl Pts',(12.0338048104555,20.5252990659819,11.2889040796134));
#53560=CARTESIAN_POINT('Ctrl Pts',(12.03165476243,20.5299850803084,11.2911631287932));
#53561=CARTESIAN_POINT('Ctrl Pts',(12.0305797384172,20.5323280874717,11.2922926533832));
#53562=CARTESIAN_POINT('Ctrl Pts',(12.0295073044338,20.5346731862636,11.2934231138684));
#53563=CARTESIAN_POINT('Ctrl Pts',(12.0284443643625,20.5370058241997,11.2945471759878));
#53564=CARTESIAN_POINT('Ctrl Pts',(12.0273814242911,20.5393384621358,11.2956712381073));
#53565=CARTESIAN_POINT('Ctrl Pts',(12.0263202972797,20.5416711025003,11.2967970058409));
#53566=CARTESIAN_POINT('Ctrl Pts',(12.0252610013046,20.5440037453176,11.2979244960981));
#53567=CARTESIAN_POINT('Origin',(-27.5,24.,-29.5));
#53568=CARTESIAN_POINT('',(-0.479749284976033,24.449552064594,-35.9844354373545));
#53569=CARTESIAN_POINT('',(-4.5,19.4038059222875,-34.0961940777126));
#53570=CARTESIAN_POINT('Ctrl Pts',(-0.479749284976206,24.4495520645939,
-35.9844354373545));
#53571=CARTESIAN_POINT('Ctrl Pts',(-0.487787721497241,24.4471112388692,
-35.9846046545909));
#53572=CARTESIAN_POINT('Ctrl Pts',(-0.495820774766061,24.4446422966896,
-35.9847744365369));
#53573=CARTESIAN_POINT('Ctrl Pts',(-0.83210386168481,24.3400450302139,-35.9919059041802));
#53574=CARTESIAN_POINT('Ctrl Pts',(-1.15106142213831,24.1908654782632,-35.9997450345785));
#53575=CARTESIAN_POINT('Ctrl Pts',(-2.0591668517866,23.6449502530038,-36.0004916773265));
#53576=CARTESIAN_POINT('Ctrl Pts',(-2.6011888924699,23.1493978597753,-35.964858749013));
#53577=CARTESIAN_POINT('Ctrl Pts',(-3.4592693304692,22.1493428393408,-35.7514047764218));
#53578=CARTESIAN_POINT('Ctrl Pts',(-3.84102577827634,21.5700258352893,-35.5628511467763));
#53579=CARTESIAN_POINT('Ctrl Pts',(-4.36201868849172,20.429896659423,-34.9696711241991));
#53580=CARTESIAN_POINT('Ctrl Pts',(-4.5,19.8699310744596,-34.5623192298848));
#53581=CARTESIAN_POINT('Ctrl Pts',(-4.5,19.4038059222874,-34.0961940777125));
#53582=CARTESIAN_POINT('',(5.47974928497604,19.0969304167095,-33.767306956549));
#53583=CARTESIAN_POINT('Ctrl Pts',(-4.5,19.4038059222874,-34.0961940777125));
#53584=CARTESIAN_POINT('Ctrl Pts',(-4.50000000000002,18.9376807701152,-33.6300689255403));
#53585=CARTESIAN_POINT('Ctrl Pts',(-4.36201868849172,18.5303288758009,-33.0701033405769));
#53586=CARTESIAN_POINT('Ctrl Pts',(-3.84102577827634,17.9371488532237,-31.9299741647106));
#53587=CARTESIAN_POINT('Ctrl Pts',(-3.4592693304692,17.7485952235782,-31.3506571606591));
#53588=CARTESIAN_POINT('Ctrl Pts',(-2.6011888924699,17.535141250987,-30.3506021402247));
#53589=CARTESIAN_POINT('Ctrl Pts',(-2.0591668517866,17.4995083226735,-29.8550497469961));
#53590=CARTESIAN_POINT('Ctrl Pts',(-1.15106142213831,17.5002549654215,-29.3091345217367));
#53591=CARTESIAN_POINT('Ctrl Pts',(-0.832103861684809,17.5080940958198,
-29.159954969786));
#53592=CARTESIAN_POINT('Ctrl Pts',(-0.175592799682984,17.5220165545405,
-28.9557542080835));
#53593=CARTESIAN_POINT('Ctrl Pts',(0.16214713396049,17.5276310629496,-28.9013011251849));
#53594=CARTESIAN_POINT('Ctrl Pts',(0.837852866039515,17.5276310629496,-28.9013011251849));
#53595=CARTESIAN_POINT('Ctrl Pts',(1.17559279968299,17.5220165545405,-28.9557542080835));
#53596=CARTESIAN_POINT('Ctrl Pts',(1.83210386168481,17.5080940958198,-29.159954969786));
#53597=CARTESIAN_POINT('Ctrl Pts',(2.15106142213831,17.5002549654215,-29.3091345217367));
#53598=CARTESIAN_POINT('Ctrl Pts',(3.05916685178659,17.4995083226735,-29.8550497469961));
#53599=CARTESIAN_POINT('Ctrl Pts',(3.6011888924699,17.535141250987,-30.3506021402247));
#53600=CARTESIAN_POINT('Ctrl Pts',(4.4592693304692,17.7485952235782,-31.3506571606591));
#53601=CARTESIAN_POINT('Ctrl Pts',(4.84102577827634,17.9371488532237,-31.9299741647106));
#53602=CARTESIAN_POINT('Ctrl Pts',(5.30317151084732,18.4633280213185,-32.9413234995576));
#53603=CARTESIAN_POINT('Ctrl Pts',(5.43322575640614,18.7577882106247,-33.3776378158014));
#53604=CARTESIAN_POINT('Ctrl Pts',(5.47974928497605,19.0969304167095,-33.767306956549));
#53605=CARTESIAN_POINT('',(6.46850196850286,19.4038059222874,-34.0961940777125));
#53606=CARTESIAN_POINT('Ctrl Pts',(6.46850196850286,19.4038059222874,-34.0961940777125));
#53607=CARTESIAN_POINT('Ctrl Pts',(6.42969677477097,19.387186062691,-34.0795742181161));
#53608=CARTESIAN_POINT('Ctrl Pts',(6.39051727695282,19.3709872335019,-34.0631950428732));
#53609=CARTESIAN_POINT('Ctrl Pts',(6.35094365239953,19.3552171637802,-34.0470861662623));
#53610=CARTESIAN_POINT('Ctrl Pts',(6.33115684012288,19.3473321289194,-34.0390317279569));
#53611=CARTESIAN_POINT('Ctrl Pts',(6.31127148089585,19.3395543228797,-34.0310448643094));
#53612=CARTESIAN_POINT('Ctrl Pts',(6.29128481869646,19.3318848880616,-34.023129591521));
#53613=CARTESIAN_POINT('Ctrl Pts',(6.27129815649708,19.3242154532436,-34.0152143187326));
#53614=CARTESIAN_POINT('Ctrl Pts',(6.25120089560369,19.3166511660681,-34.0073671890898));
#53615=CARTESIAN_POINT('Ctrl Pts',(6.23106051252081,19.3092186682823,-33.9996189280884));
#53616=CARTESIAN_POINT('Ctrl Pts',(6.15049898018926,19.279488677139,-33.9686258840826));
#53617=CARTESIAN_POINT('Ctrl Pts',(6.0690345181408,19.251780884441,-33.9391267241935));
#53618=CARTESIAN_POINT('Ctrl Pts',(5.98660180893713,19.226111117583,-33.9113473005207));
#53619=CARTESIAN_POINT('Ctrl Pts',(5.90416909973346,19.200441350725,-33.8835678768478));
#53620=CARTESIAN_POINT('Ctrl Pts',(5.82076819215945,19.1768094474068,-33.857508189391));
#53621=CARTESIAN_POINT('Ctrl Pts',(5.73632102160145,19.1552595186588,-33.8334154664541));
#53622=CARTESIAN_POINT('Ctrl Pts',(5.65187385104345,19.1337095899108,-33.8093227435172));
#53623=CARTESIAN_POINT('Ctrl Pts',(5.56638048594122,19.1142413799255,-33.7871969851001));
#53624=CARTESIAN_POINT('Ctrl Pts',(5.47974928497605,19.0969304167095,-33.767306956549));
#53625=CARTESIAN_POINT('',(9.,21.8205505282297,-35.623724356958));
#53626=CARTESIAN_POINT('Ctrl Pts',(9.00000000000001,21.8205505282297,-35.623724356958));
#53627=CARTESIAN_POINT('Ctrl Pts',(8.95346014289149,21.7244577489746,-35.5895246861726));
#53628=CARTESIAN_POINT('Ctrl Pts',(8.90405895499889,21.6302929744456,-35.5534659740372));
#53629=CARTESIAN_POINT('Ctrl Pts',(8.85183957948243,21.5379901961101,-35.515689114795));
#53630=CARTESIAN_POINT('Ctrl Pts',(8.8287249881567,21.4971329285086,-35.4989674161091));
#53631=CARTESIAN_POINT('Ctrl Pts',(8.8050575608266,21.4566406978177,-35.4819090745412));
#53632=CARTESIAN_POINT('Ctrl Pts',(8.78083801363281,21.416508970204,-35.4645263096883));
#53633=CARTESIAN_POINT('Ctrl Pts',(8.76110421713693,21.3838101199976,-35.4503630414241));
#53634=CARTESIAN_POINT('Ctrl Pts',(8.74100391086643,21.35135072485,-35.4359841712445));
#53635=CARTESIAN_POINT('Ctrl Pts',(8.72053669502811,21.3191288718177,-35.4213959497807));
#53636=CARTESIAN_POINT('Ctrl Pts',(8.70006947918979,21.2869070187855,-35.4068077283168));
#53637=CARTESIAN_POINT('Ctrl Pts',(8.67929735859121,21.2550205867036,-35.3920543871654));
#53638=CARTESIAN_POINT('Ctrl Pts',(8.65823682537814,21.2234794248792,-35.3771535198539));
#53639=CARTESIAN_POINT('Ctrl Pts',(8.61611575895202,21.1603971012304,-35.3473517852309));
#53640=CARTESIAN_POINT('Ctrl Pts',(8.57282604017638,21.0986702165659,-35.3169489172681));
#53641=CARTESIAN_POINT('Ctrl Pts',(8.52839379871621,21.0382364371097,-35.2860138780974));
#53642=CARTESIAN_POINT('Ctrl Pts',(8.46854242649671,20.9568305815868,-35.2443435845631));
#53643=CARTESIAN_POINT('Ctrl Pts',(8.40661847193035,20.8777689016067,-35.2017079160559));
#53644=CARTESIAN_POINT('Ctrl Pts',(8.34265344218604,20.8009353674463,-35.1582674769016));
#53645=CARTESIAN_POINT('Ctrl Pts',(8.31164622513931,20.7636901089089,-35.1372096093317));
#53646=CARTESIAN_POINT('Ctrl Pts',(8.28015866509545,20.7269687611952,-35.115962632633));
#53647=CARTESIAN_POINT('Ctrl Pts',(8.24819049410234,20.6907602051346,-35.0945448411895));
#53648=CARTESIAN_POINT('Ctrl Pts',(8.18110789572019,20.6147795046832,-35.0496013534325));
#53649=CARTESIAN_POINT('Ctrl Pts',(8.11191331368323,20.5410566675232,-35.003903946791));
#53650=CARTESIAN_POINT('Ctrl Pts',(8.04057741178885,20.469516804865,-34.9576259860006));
#53651=CARTESIAN_POINT('Ctrl Pts',(8.00778951765573,20.4366351648935,-34.9363553937911));
#53652=CARTESIAN_POINT('Ctrl Pts',(7.97454868755145,20.4042151472244,-34.914962155559));
#53653=CARTESIAN_POINT('Ctrl Pts',(7.94084935210846,20.3722519745585,-34.8934631048989));
#53654=CARTESIAN_POINT('Ctrl Pts',(7.8873402320094,20.3214996014792,-34.8593260731544));
#53655=CARTESIAN_POINT('Ctrl Pts',(7.83267546585817,20.2718982517448,-34.8249228107028));
#53656=CARTESIAN_POINT('Ctrl Pts',(7.77682107172572,20.2234349384799,-34.7903266757456));
#53657=CARTESIAN_POINT('Ctrl Pts',(7.76285747319261,20.2113191101637,-34.7816776420063));
#53658=CARTESIAN_POINT('Ctrl Pts',(7.74883069321957,20.1992842918547,-34.7730235674644));
#53659=CARTESIAN_POINT('Ctrl Pts',(7.73475444641459,20.1873416529407,-34.7643742580291));
#53660=CARTESIAN_POINT('Ctrl Pts',(7.72067819960961,20.1753990140267,-34.7557249485937));
#53661=CARTESIAN_POINT('Ctrl Pts',(7.70654820889115,20.1635448369695,-34.7470777562327));
#53662=CARTESIAN_POINT('Ctrl Pts',(7.6923643113654,20.1517783193376,-34.7384339183794));
#53663=CARTESIAN_POINT('Ctrl Pts',(7.66399651631389,20.1282452840736,-34.7211462426727));
#53664=CARTESIAN_POINT('Ctrl Pts',(7.63541313595312,20.1050628364807,-34.7038719849967));
#53665=CARTESIAN_POINT('Ctrl Pts',(7.60661239183694,20.0822251919125,-34.6866213041936));
#53666=CARTESIAN_POINT('Ctrl Pts',(7.52978950224896,20.0213082294883,-34.6406069671573));
#53667=CARTESIAN_POINT('Ctrl Pts',(7.45142280256881,19.9628419279767,-34.5947564545559));
#53668=CARTESIAN_POINT('Ctrl Pts',(7.37145495609334,19.9067437857951,-34.54928088283));
#53669=CARTESIAN_POINT('Ctrl Pts',(7.33150367449569,19.8787176130997,-34.5265616593933));
#53670=CARTESIAN_POINT('Ctrl Pts',(7.29115221492108,19.8512831242448,-34.5039360181928));
#53671=CARTESIAN_POINT('Ctrl Pts',(7.25039045889862,19.8244338918418,-34.4814302842056));
#53672=CARTESIAN_POINT('Ctrl Pts',(7.18921452103797,19.7841381064446,-34.4476532952272));
#53673=CARTESIAN_POINT('Ctrl Pts',(7.1271146527043,19.7451597465569,-34.4141481991929));
#53674=CARTESIAN_POINT('Ctrl Pts',(7.06404548727158,19.7074866640624,-34.3810173460166));
#53675=CARTESIAN_POINT('Ctrl Pts',(7.00097632183886,19.6698135815678,-34.3478864928404));
#53676=CARTESIAN_POINT('Ctrl Pts',(6.93693791838452,19.6334456770075,-34.3151298825222));
#53677=CARTESIAN_POINT('Ctrl Pts',(6.87187092606532,19.5983834435419,-34.2828624501986));
#53678=CARTESIAN_POINT('Ctrl Pts',(6.80680393374611,19.5633212100763,-34.250595017875));
#53679=CARTESIAN_POINT('Ctrl Pts',(6.74070843553403,19.5295644892472,-34.218816763546));
#53680=CARTESIAN_POINT('Ctrl Pts',(6.67350874794502,19.4971276142215,-34.1876584164691));
#53681=CARTESIAN_POINT('Ctrl Pts',(6.606309060356,19.4646907391959,-34.1565000693923));
#53682=CARTESIAN_POINT('Ctrl Pts',(6.53800530034302,19.4335734741426,-34.1259616295677));
#53683=CARTESIAN_POINT('Ctrl Pts',(6.46850196850286,19.4038059222874,-34.0961940777125));
#53684=CARTESIAN_POINT('',(9.,21.8205505282297,-23.3762756430421));
#53685=CARTESIAN_POINT('Origin',(9.,24.,-29.5));
#53686=CARTESIAN_POINT('',(-0.4749371855331,23.5,-23.0192593015922));
#53687=CARTESIAN_POINT('Ctrl Pts',(-0.474937185533098,23.5,-23.0192593015921));
#53688=CARTESIAN_POINT('Ctrl Pts',(-0.424823582743024,23.0013759479572,
-23.0577289823931));
#53689=CARTESIAN_POINT('Ctrl Pts',(-0.296594058108877,22.5028914382015,
-23.1564811915671));
#53690=CARTESIAN_POINT('Ctrl Pts',(0.15897422172366,21.4311680507649,-23.4946656308148));
#53691=CARTESIAN_POINT('Ctrl Pts',(0.540730669530802,20.8882015186037,-23.7709770626967));
#53692=CARTESIAN_POINT('Ctrl Pts',(1.3988111075301,20.0301210806044,-24.3271879977151));
#53693=CARTESIAN_POINT('Ctrl Pts',(1.9408331482134,19.6545163376753,-24.6524001701562));
#53694=CARTESIAN_POINT('Ctrl Pts',(2.84893857786169,19.2690239360916,-25.0389484840403));
#53695=CARTESIAN_POINT('Ctrl Pts',(3.16789613831519,19.1690811655562,-25.1499774591023));
#53696=CARTESIAN_POINT('Ctrl Pts',(3.82440720031701,19.0345340872051,-25.3042138673978));
#53697=CARTESIAN_POINT('Ctrl Pts',(4.16214713396049,19.,-25.346688068541));
#53698=CARTESIAN_POINT('Ctrl Pts',(4.83785286603951,19.,-25.346688068541));
#53699=CARTESIAN_POINT('Ctrl Pts',(5.17559279968299,19.0345340872051,-25.3042138673978));
#53700=CARTESIAN_POINT('Ctrl Pts',(5.83210386168481,19.1690811655562,-25.1499774591023));
#53701=CARTESIAN_POINT('Ctrl Pts',(6.15106142213831,19.2690239360916,-25.0389484840403));
#53702=CARTESIAN_POINT('Ctrl Pts',(7.0591668517866,19.6545163376753,-24.6524001701562));
#53703=CARTESIAN_POINT('Ctrl Pts',(7.6011888924699,20.0301210806044,-24.3271879977151));
#53704=CARTESIAN_POINT('Ctrl Pts',(8.40704600281358,20.8359781909481,-23.8048284181393));
#53705=CARTESIAN_POINT('Ctrl Pts',(8.74715233812993,21.2984854410813,-23.5620799693133));
#53706=CARTESIAN_POINT('Ctrl Pts',(9.00000000000001,21.8205505282297,-23.376275643042));
#53707=CARTESIAN_POINT('',(-27.5,23.5,-23.0192593015922));
#53708=CARTESIAN_POINT('',(-27.5,23.5,-23.0192593015922));
#53709=CARTESIAN_POINT('',(-27.5,24.5,-23.0192593015922));
#53710=CARTESIAN_POINT('Origin',(-27.5,24.,-29.5));
#53711=CARTESIAN_POINT('',(-2.16746515426235,24.5,-23.0192593015922));
#53712=CARTESIAN_POINT('',(-27.5,24.5,-23.0192593015922));
#53713=CARTESIAN_POINT('',(5.47974928497604,28.9030695832906,-25.2326930434511));
#53714=CARTESIAN_POINT('Ctrl Pts',(-2.16746515426287,24.5000000000004,-23.0192593015922));
#53715=CARTESIAN_POINT('Ctrl Pts',(-2.4880924621126,24.7655201130862,-23.0397446230579));
#53716=CARTESIAN_POINT('Ctrl Pts',(-2.78031808130512,25.0593693334481,-23.0797009860313));
#53717=CARTESIAN_POINT('Ctrl Pts',(-3.4592693304692,25.8506571606591,-23.2485952235782));
#53718=CARTESIAN_POINT('Ctrl Pts',(-3.84102577827635,26.4299741647106,-23.4371488532237));
#53719=CARTESIAN_POINT('Ctrl Pts',(-4.36201868849172,27.570103340577,-24.0303288758009));
#53720=CARTESIAN_POINT('Ctrl Pts',(-4.5,28.1300689255403,-24.4376807701152));
#53721=CARTESIAN_POINT('Ctrl Pts',(-4.5,29.0623192298848,-25.3699310744596));
#53722=CARTESIAN_POINT('Ctrl Pts',(-4.36201868849172,29.4696711241991,-25.929896659423));
#53723=CARTESIAN_POINT('Ctrl Pts',(-3.84102577827634,30.0628511467763,-27.0700258352893));
#53724=CARTESIAN_POINT('Ctrl Pts',(-3.4592693304692,30.2514047764218,-27.6493428393408));
#53725=CARTESIAN_POINT('Ctrl Pts',(-2.6011888924699,30.464858749013,-28.6493978597753));
#53726=CARTESIAN_POINT('Ctrl Pts',(-2.05916685178659,30.5004916773265,-29.1449502530038));
#53727=CARTESIAN_POINT('Ctrl Pts',(-1.1510614221383,30.4997450345785,-29.6908654782632));
#53728=CARTESIAN_POINT('Ctrl Pts',(-0.832103861684804,30.4919059041802,
-29.8400450302139));
#53729=CARTESIAN_POINT('Ctrl Pts',(-0.17559279968298,30.4779834454595,-30.0442457919164));
#53730=CARTESIAN_POINT('Ctrl Pts',(0.162147133960491,30.4723689370504,-30.098698874815));
#53731=CARTESIAN_POINT('Ctrl Pts',(0.500000000000003,30.4723689370504,-30.098698874815));
#53732=CARTESIAN_POINT('Ctrl Pts',(0.837852866039515,30.4723689370504,-30.098698874815));
#53733=CARTESIAN_POINT('Ctrl Pts',(1.17559279968299,30.4779834454595,-30.0442457919164));
#53734=CARTESIAN_POINT('Ctrl Pts',(1.83210386168481,30.4919059041802,-29.8400450302139));
#53735=CARTESIAN_POINT('Ctrl Pts',(2.15106142213831,30.4997450345785,-29.6908654782632));
#53736=CARTESIAN_POINT('Ctrl Pts',(3.05916685178659,30.5004916773265,-29.1449502530038));
#53737=CARTESIAN_POINT('Ctrl Pts',(3.6011888924699,30.464858749013,-28.6493978597753));
#53738=CARTESIAN_POINT('Ctrl Pts',(4.4592693304692,30.2514047764218,-27.6493428393408));
#53739=CARTESIAN_POINT('Ctrl Pts',(4.84102577827634,30.0628511467763,-27.0700258352893));
#53740=CARTESIAN_POINT('Ctrl Pts',(5.30317151084787,29.5366719786809,-26.0586765004412));
#53741=CARTESIAN_POINT('Ctrl Pts',(5.43322575640683,29.2422117893737,-25.6223621841961));
#53742=CARTESIAN_POINT('Ctrl Pts',(5.47974928497643,28.9030695832877,-25.2326930434478));
#53743=CARTESIAN_POINT('Ctrl Pts',(9.00000000000001,26.1794494717703,-23.3762756430421));
#53744=CARTESIAN_POINT('Ctrl Pts',(8.95705829231163,26.2681130022172,-23.4078312247981));
#53745=CARTESIAN_POINT('Ctrl Pts',(8.91168036869606,26.3551343885975,-23.4409704863788));
#53746=CARTESIAN_POINT('Ctrl Pts',(8.86390090675223,26.4405673266778,-23.4755804326099));
#53747=CARTESIAN_POINT('Ctrl Pts',(8.84001117578032,26.4832837957179,-23.4928854057254));
#53748=CARTESIAN_POINT('Ctrl Pts',(8.81552054185688,26.5256028638167,-23.5105582058587));
#53749=CARTESIAN_POINT('Ctrl Pts',(8.79043025746389,26.5675295920083,-23.528585446793));
#53750=CARTESIAN_POINT('Ctrl Pts',(8.7778851152674,26.5884929561041,-23.5375990672602));
#53751=CARTESIAN_POINT('Ctrl Pts',(8.76519002979884,26.609358216606,-23.5467012979276));
#53752=CARTESIAN_POINT('Ctrl Pts',(8.75234496374892,26.6301259112976,-23.5558905048174));
#53753=CARTESIAN_POINT('Ctrl Pts',(8.73949989769899,26.6508936059893,-23.5650797117071));
#53754=CARTESIAN_POINT('Ctrl Pts',(8.72649859393935,26.6715735006014,-23.5743603460415));
#53755=CARTESIAN_POINT('Ctrl Pts',(8.71336126912799,26.6921342492179,-23.5837162691274));
#53756=CARTESIAN_POINT('Ctrl Pts',(8.66081196988253,26.7743772436841,-23.6211399614708));
#53757=CARTESIAN_POINT('Ctrl Pts',(8.60632596649448,26.8543516336304,-23.6595986599364));
#53758=CARTESIAN_POINT('Ctrl Pts',(8.54996616236301,26.9321961195859,-23.6989459256624));
#53759=CARTESIAN_POINT('Ctrl Pts',(8.49360635823154,27.0100406055414,-23.7382931913885));
#53760=CARTESIAN_POINT('Ctrl Pts',(8.43537241023437,27.0857549441919,-23.778529024375));
#53761=CARTESIAN_POINT('Ctrl Pts',(8.3752944761572,27.1594450023802,-23.8195149862323));
#53762=CARTESIAN_POINT('Ctrl Pts',(8.31521654208003,27.2331350605686,-23.8605009480896));
#53763=CARTESIAN_POINT('Ctrl Pts',(8.25329445818045,27.30480070874,-23.9022370388178));
#53764=CARTESIAN_POINT('Ctrl Pts',(8.18952758291043,27.374520145879,-23.9445867313424));
#53765=CARTESIAN_POINT('Ctrl Pts',(8.1257607076404,27.4442395830179,-23.986936423867));
#53766=CARTESIAN_POINT('Ctrl Pts',(8.060149019676,27.5120127958191,-24.0298997181881));
#53767=CARTESIAN_POINT('Ctrl Pts',(7.99266073026277,27.5778933778524,-24.0733361102385));
#53768=CARTESIAN_POINT('Ctrl Pts',(7.92517244084954,27.6437739598858,-24.116772502289));
#53769=CARTESIAN_POINT('Ctrl Pts',(7.8558076658742,27.7077620280224,-24.1606819920687));
#53770=CARTESIAN_POINT('Ctrl Pts',(7.78450056732235,27.7698880650835,-24.2049132229263));
#53771=CARTESIAN_POINT('Ctrl Pts',(7.76667379268438,27.7854195743488,-24.2159710306407));
#53772=CARTESIAN_POINT('Ctrl Pts',(7.74873232686828,27.8008282864164,-24.22704452449));
#53773=CARTESIAN_POINT('Ctrl Pts',(7.73071339035289,27.8160832000095,-24.2381078488242));
#53774=CARTESIAN_POINT('Ctrl Pts',(7.71269445383749,27.8313381136026,-24.2491711731584));
#53775=CARTESIAN_POINT('Ctrl Pts',(7.69458755981618,27.8464484150864,-24.260230837196));
#53776=CARTESIAN_POINT('Ctrl Pts',(7.67639234498307,27.8614157598908,-24.2712842197217));
#53777=CARTESIAN_POINT('Ctrl Pts',(7.64000191531686,27.8913504494995,-24.2933909847731));
#53778=CARTESIAN_POINT('Ctrl Pts',(7.6032583061425,27.9207134511579,-24.315472623777));
#53779=CARTESIAN_POINT('Ctrl Pts',(7.5661573924812,27.9495162798162,-24.3375080087296));
#53780=CARTESIAN_POINT('Ctrl Pts',(7.49195556515859,28.0071219371326,-24.3815787786349));
#53781=CARTESIAN_POINT('Ctrl Pts',(7.41632621823999,28.0624890532935,-24.4254645323354));
#53782=CARTESIAN_POINT('Ctrl Pts',(7.33921485459175,28.1156845128685,-24.4689819138322));
#53783=CARTESIAN_POINT('Ctrl Pts',(7.26210349094351,28.1688799724435,-24.512499295329));
#53784=CARTESIAN_POINT('Ctrl Pts',(7.18351019104125,28.2199038792518,-24.555648304622));
#53785=CARTESIAN_POINT('Ctrl Pts',(7.10334918914321,28.2687905780663,-24.5982222579908));
#53786=CARTESIAN_POINT('Ctrl Pts',(7.02318818724517,28.3176772768808,-24.6407962113595));
#53787=CARTESIAN_POINT('Ctrl Pts',(6.94145966183726,28.3644270716961,-24.6827951088039));
#53788=CARTESIAN_POINT('Ctrl Pts',(6.85804161637582,28.4090406819896,-24.7239807093605));
#53789=CARTESIAN_POINT('Ctrl Pts',(6.77462357091438,28.4536542922832,-24.7651663099171));
#53790=CARTESIAN_POINT('Ctrl Pts',(6.68951653676254,28.4961321630524,-24.8055391316471));
#53791=CARTESIAN_POINT('Ctrl Pts',(6.60255363933461,28.536437830911,-24.8448166731826));
#53792=CARTESIAN_POINT('Ctrl Pts',(6.52294885299043,28.5733331526315,-24.88077086048));
#53793=CARTESIAN_POINT('Ctrl Pts',(6.44178967661408,28.6084080323174,-24.9158082171533));
#53794=CARTESIAN_POINT('Ctrl Pts',(6.35890495094121,28.6416023508446,-24.9496674442389));
#53795=CARTESIAN_POINT('Ctrl Pts',(6.35124366514855,28.6446706020678,-24.9527971549704));
#53796=CARTESIAN_POINT('Ctrl Pts',(6.34356763132479,28.6477227494887,-24.9559167999232));
#53797=CARTESIAN_POINT('Ctrl Pts',(6.33587671150817,28.6507587230625,-24.9590261727403));
#53798=CARTESIAN_POINT('Ctrl Pts',(6.31315265014489,28.6597289959861,-24.9682133155503));
#53799=CARTESIAN_POINT('Ctrl Pts',(6.29029836457671,28.6685582033252,-24.9773104490501));
#53800=CARTESIAN_POINT('Ctrl Pts',(6.26730968071364,28.6772445405875,-24.9863115407082));
#53801=CARTESIAN_POINT('Ctrl Pts',(6.24432099685057,28.6859308778499,-24.9953126323663));
#53802=CARTESIAN_POINT('Ctrl Pts',(6.22124816944649,28.6944552549752,-25.004197914353));
#53803=CARTESIAN_POINT('Ctrl Pts',(6.19810571453666,28.7028116039512,-25.0129560936244));
#53804=CARTESIAN_POINT('Ctrl Pts',(6.15182080471699,28.7195243019031,-25.0304724521673));
#53805=CARTESIAN_POINT('Ctrl Pts',(6.10523671422342,28.7355729176463,-25.0474882640567));
#53806=CARTESIAN_POINT('Ctrl Pts',(6.05834147324056,28.7509548359018,-25.0639622925458));
#53807=CARTESIAN_POINT('Ctrl Pts',(5.96455099127483,28.7817186724127,-25.0969103495238));
#53808=CARTESIAN_POINT('Ctrl Pts',(5.86951700719543,28.8098189622502,-25.1276912729003));
#53809=CARTESIAN_POINT('Ctrl Pts',(5.77312645725412,28.8351989642454,-25.1559407325179));
#53810=CARTESIAN_POINT('Ctrl Pts',(5.6767359073128,28.8605789662405,-25.1841901921354));
#53811=CARTESIAN_POINT('Ctrl Pts',(5.578988930962,28.8832391545062,-25.209908187994));
#53812=CARTESIAN_POINT('Ctrl Pts',(5.47974928497603,28.9030695832906,-25.2326930434511));
#53813=CARTESIAN_POINT('Ctrl Pts',(-0.479749284976029,24.449552064594,-35.9844354373545));
#53814=CARTESIAN_POINT('Ctrl Pts',(-0.433225756406109,24.9648995101448,
-35.9487074992219));
#53815=CARTESIAN_POINT('Ctrl Pts',(-0.303171510847291,25.4816351185375,
-35.848401484125));
#53816=CARTESIAN_POINT('Ctrl Pts',(0.158974221723663,26.5688319492351,-35.5053343691852));
#53817=CARTESIAN_POINT('Ctrl Pts',(0.540730669530803,27.1117984813963,-35.2290229373034));
#53818=CARTESIAN_POINT('Ctrl Pts',(1.3988111075301,27.9698789193956,-34.6728120022849));
#53819=CARTESIAN_POINT('Ctrl Pts',(1.9408331482134,28.3454836623247,-34.3475998298438));
#53820=CARTESIAN_POINT('Ctrl Pts',(2.84893857786169,28.7309760639084,-33.9610515159597));
#53821=CARTESIAN_POINT('Ctrl Pts',(3.16789613831519,28.8309188344438,-33.8500225408978));
#53822=CARTESIAN_POINT('Ctrl Pts',(3.82440720031702,28.965465912795,-33.6957861326022));
#53823=CARTESIAN_POINT('Ctrl Pts',(4.16214713396049,29.,-33.653311931459));
#53824=CARTESIAN_POINT('Ctrl Pts',(4.5,29.,-33.653311931459));
#53825=CARTESIAN_POINT('Ctrl Pts',(4.83785286603951,29.,-33.653311931459));
#53826=CARTESIAN_POINT('Ctrl Pts',(5.17559279968299,28.965465912795,-33.6957861326022));
#53827=CARTESIAN_POINT('Ctrl Pts',(5.83210386168481,28.8309188344438,-33.8500225408978));
#53828=CARTESIAN_POINT('Ctrl Pts',(6.15106142213831,28.7309760639084,-33.9610515159597));
#53829=CARTESIAN_POINT('Ctrl Pts',(7.05916685178659,28.3454836623247,-34.3475998298438));
#53830=CARTESIAN_POINT('Ctrl Pts',(7.6011888924699,27.9698789193956,-34.6728120022849));
#53831=CARTESIAN_POINT('Ctrl Pts',(8.40704600281352,27.164021809052,-35.1951715818606));
#53832=CARTESIAN_POINT('Ctrl Pts',(8.74715233812982,26.7015145589189,-35.4379200306866));
#53833=CARTESIAN_POINT('Ctrl Pts',(8.99999999999988,26.1794494717706,-35.6237243569579));
#53834=CARTESIAN_POINT('Origin',(4.5,24.,6.93889390390723E-15));
#53835=CARTESIAN_POINT('',(-0.4682273254511,23.4372236299906,-37.));
#53836=CARTESIAN_POINT('',(9.20487219075894,22.3076118445749,-37.));
#53837=CARTESIAN_POINT('Origin',(4.5,24.,-37.));
#53838=CARTESIAN_POINT('Ctrl Pts',(-0.468227325451101,23.4372236299906,
-37.));
#53839=CARTESIAN_POINT('Ctrl Pts',(-0.489596442334827,23.6258716189257,
-36.8053870417944));
#53840=CARTESIAN_POINT('Ctrl Pts',(-0.5,23.8141368149253,-36.6140664153501));
#53841=CARTESIAN_POINT('Ctrl Pts',(-0.5,24.1465968404519,-36.2816063898235));
#53842=CARTESIAN_POINT('Ctrl Pts',(-0.49353975798667,24.2967931218089,-36.1332972845454));
#53843=CARTESIAN_POINT('Ctrl Pts',(-0.479749284976031,24.449552064594,-35.9844354373545));
#53844=CARTESIAN_POINT('',(9.5,23.9999999737538,-35.9999999933889));
#53845=CARTESIAN_POINT('Ctrl Pts',(8.9999999999999,26.1794494717706,-35.6237243569579));
#53846=CARTESIAN_POINT('Ctrl Pts',(9.00499129300368,26.1691437423086,-35.6273921929549));
#53847=CARTESIAN_POINT('Ctrl Pts',(9.00995373459336,26.1588072269372,-35.6310416269391));
#53848=CARTESIAN_POINT('Ctrl Pts',(9.0148783576886,26.148458372271,-35.6346659517895));
#53849=CARTESIAN_POINT('Ctrl Pts',(9.01980298078383,26.1381095176048,-35.6382902766398));
#53850=CARTESIAN_POINT('Ctrl Pts',(9.02469199992633,26.1277437765558,-35.6418911200617));
#53851=CARTESIAN_POINT('Ctrl Pts',(9.02954542600208,26.117361124825,-35.6454683632644));
#53852=CARTESIAN_POINT('Ctrl Pts',(9.03782625969404,26.0996464195997,-35.6515717952679));
#53853=CARTESIAN_POINT('Ctrl Pts',(9.04600352023965,26.0818824635388,-35.6576065392216));
#53854=CARTESIAN_POINT('Ctrl Pts',(9.05407713254688,26.0640691586593,-35.6635718950109));
#53855=CARTESIAN_POINT('Ctrl Pts',(9.05546746601008,26.0610015808612,-35.6645991717067));
#53856=CARTESIAN_POINT('Ctrl Pts',(9.05685472633728,26.0579325366857,-35.665624391158));
#53857=CARTESIAN_POINT('Ctrl Pts',(9.05823891476301,26.0548620249938,-35.6666475507992));
#53858=CARTESIAN_POINT('Ctrl Pts',(9.07474419566317,26.018248759747,-35.6788478675838));
#53859=CARTESIAN_POINT('Ctrl Pts',(9.09081329757223,25.981425963608,-35.6907557840418));
#53860=CARTESIAN_POINT('Ctrl Pts',(9.10644398031607,25.9443956270176,-35.702364507792));
#53861=CARTESIAN_POINT('Ctrl Pts',(9.1086589941613,25.9391480821991,-35.7040095724545));
#53862=CARTESIAN_POINT('Ctrl Pts',(9.11086526354452,25.9338961913387,-35.7056486746972));
#53863=CARTESIAN_POINT('Ctrl Pts',(9.11306274833671,25.9286400605162,-35.7072817699926));
#53864=CARTESIAN_POINT('Ctrl Pts',(9.12802360671024,25.8928554083961,-35.7184001665852));
#53865=CARTESIAN_POINT('Ctrl Pts',(9.14258366284676,25.8568594685192,-35.7292449494624));
#53866=CARTESIAN_POINT('Ctrl Pts',(9.15672841971636,25.8206816235516,-35.7398011083539));
#53867=CARTESIAN_POINT('Ctrl Pts',(9.17322261740404,25.7784946469701,-35.752110642776));
#53868=CARTESIAN_POINT('Ctrl Pts',(9.1891563977555,25.7360515257514,-35.764030863753));
#53869=CARTESIAN_POINT('Ctrl Pts',(9.20453378247886,25.6933291108338,-35.7755585793107));
#53870=CARTESIAN_POINT('Ctrl Pts',(9.20718005181626,25.6859770793506,-35.7775423652899));
#53871=CARTESIAN_POINT('Ctrl Pts',(9.20980980902294,25.6786167048553,-35.7795145037213));
#53872=CARTESIAN_POINT('Ctrl Pts',(9.21242308500116,25.671247870195,-35.7814749876001));
#53873=CARTESIAN_POINT('Ctrl Pts',(9.23546015598842,25.6062886509707,-35.7987574356316));
#53874=CARTESIAN_POINT('Ctrl Pts',(9.2572083241211,25.5407013867059,-35.815128565412));
#53875=CARTESIAN_POINT('Ctrl Pts',(9.277647393158,25.4744769808417,-35.8305539170307));
#53876=CARTESIAN_POINT('Ctrl Pts',(9.28233239040935,25.4592971720703,-35.8340896812969));
#53877=CARTESIAN_POINT('Ctrl Pts',(9.28694852685422,25.4440836909435,-35.8375757061078));
#53878=CARTESIAN_POINT('Ctrl Pts',(9.29149540308989,25.42883609634,-35.8410114797098));
#53879=CARTESIAN_POINT('Ctrl Pts',(9.29365149253119,25.4216058186668,-35.8426406938784));
#53880=CARTESIAN_POINT('Ctrl Pts',(9.29579199751469,25.4143678777838,-35.84425859878));
#53881=CARTESIAN_POINT('Ctrl Pts',(9.29791690448527,25.4071222569905,-35.8458651628086));
#53882=CARTESIAN_POINT('Ctrl Pts',(9.31795789316064,25.3387854280019,-35.8610174174481));
#53883=CARTESIAN_POINT('Ctrl Pts',(9.33661353358467,25.269768592517,-35.8751629726986));
#53884=CARTESIAN_POINT('Ctrl Pts',(9.35385081458509,25.2000533307043,-35.888260097332));
#53885=CARTESIAN_POINT('Ctrl Pts',(9.35769303751339,25.1845136654066,-35.8911794714816));
#53886=CARTESIAN_POINT('Ctrl Pts',(9.36146465902595,25.1689391689937,-35.8940466623285));
#53887=CARTESIAN_POINT('Ctrl Pts',(9.36516507939256,25.1533294331882,-35.8968610404086));
#53888=CARTESIAN_POINT('Ctrl Pts',(9.36652977322614,25.1475726520426,-35.8978989669225));
#53889=CARTESIAN_POINT('Ctrl Pts',(9.36788477789201,25.1418110869741,-35.8989297055837));
#53890=CARTESIAN_POINT('Ctrl Pts',(9.36923008056749,25.1360447261538,-35.8999532391271));
#53891=CARTESIAN_POINT('Ctrl Pts',(9.3854250434066,25.0666283777718,-35.91227469511));
#53892=CARTESIAN_POINT('Ctrl Pts',(9.4002170109659,24.9965192841531,-35.9235542818067));
#53893=CARTESIAN_POINT('Ctrl Pts',(9.41356185655924,24.9256911858039,-35.9337460644235));
#53894=CARTESIAN_POINT('Ctrl Pts',(9.4170731352871,24.9070549870312,-35.9364277132482));
#53895=CARTESIAN_POINT('Ctrl Pts',(9.42048401358903,24.8883689383346,-35.9390338894768));
#53896=CARTESIAN_POINT('Ctrl Pts',(9.42379321375125,24.8696324419433,-35.9415633947187));
#53897=CARTESIAN_POINT('Ctrl Pts',(9.42449386001647,24.8656654240609,-35.942098958696));
#53898=CARTESIAN_POINT('Ctrl Pts',(9.42518994700153,24.8616961500279,-35.942631084413));
#53899=CARTESIAN_POINT('Ctrl Pts',(9.425881468401,24.8577246142275,-35.9431597654671));
#53900=CARTESIAN_POINT('Ctrl Pts',(9.42997413403971,24.8342196755289,-35.9462886849565));
#53901=CARTESIAN_POINT('Ctrl Pts',(9.43390864964311,24.8106232721573,-35.9492982524213));
#53902=CARTESIAN_POINT('Ctrl Pts',(9.43767033422769,24.7870207768946,-35.9521769341472));
#53903=CARTESIAN_POINT('Ctrl Pts',(9.44143201881227,24.763418281632,-35.9550556158731));
#53904=CARTESIAN_POINT('Ctrl Pts',(9.4450238707641,24.739793515833,-35.9578057016672));
#53905=CARTESIAN_POINT('Ctrl Pts',(9.44844616386937,24.7161465195238,-35.9604270560455));
#53906=CARTESIAN_POINT('Ctrl Pts',(9.45496209937026,24.6711234025667,-35.9654180300881));
#53907=CARTESIAN_POINT('Ctrl Pts',(9.46086375084294,24.6260198076498,-35.9699425212052));
#53908=CARTESIAN_POINT('Ctrl Pts',(9.46614854505997,24.5808346182974,-35.9739964724846));
#53909=CARTESIAN_POINT('Ctrl Pts',(9.46641509947409,24.5785555680298,-35.9742009456511));
#53910=CARTESIAN_POINT('Ctrl Pts',(9.46668008379669,24.576276311642,-35.9744042210618));
#53911=CARTESIAN_POINT('Ctrl Pts',(9.46694349854552,24.5739968483365,-35.9746062989503));
#53912=CARTESIAN_POINT('Ctrl Pts',(9.47560463179607,24.499047607582,-35.9812506631203));
#53913=CARTESIAN_POINT('Ctrl Pts',(9.48257224643251,24.4238758991093,-35.9866025262799));
#53914=CARTESIAN_POINT('Ctrl Pts',(9.48784091893968,24.3484791237477,-35.9906514402046));
#53915=CARTESIAN_POINT('Ctrl Pts',(9.48920116350454,24.3290134891398,-35.9916967724305));
#53916=CARTESIAN_POINT('Ctrl Pts',(9.4904479529791,24.3095328743889,-35.992655092703));
#53917=CARTESIAN_POINT('Ctrl Pts',(9.49158074820727,24.2900373108998,-35.9935258759464));
#53918=CARTESIAN_POINT('Ctrl Pts',(9.49161858693997,24.2893861010455,-35.9935549626988));
#53919=CARTESIAN_POINT('Ctrl Pts',(9.49165629872179,24.2887348743351,-35.9935839519911));
#53920=CARTESIAN_POINT('Ctrl Pts',(9.49169388354752,24.2880836307525,-35.9936128438172));
#53921=CARTESIAN_POINT('Ctrl Pts',(9.49444525199611,24.2404098419077,-35.9957278478682));
#53922=CARTESIAN_POINT('Ctrl Pts',(9.49651672032079,24.1926463019363,-35.9973208722724));
#53923=CARTESIAN_POINT('Ctrl Pts',(9.4979030806664,24.1447922723031,-35.9983871160602));
#53924=CARTESIAN_POINT('Ctrl Pts',(9.49790768768555,24.1446332484015,-35.9983906592989));
#53925=CARTESIAN_POINT('Ctrl Pts',(9.49791228713675,24.1444742234989,-35.9983941967189));
#53926=CARTESIAN_POINT('Ctrl Pts',(9.49791687901979,24.1443151975952,-35.9983977283201));
#53927=CARTESIAN_POINT('Ctrl Pts',(9.49860889038041,24.1203494887779,-35.998929951839));
#53928=CARTESIAN_POINT('Ctrl Pts',(9.49912904440715,24.0963610829959,-35.9993300507007));
#53929=CARTESIAN_POINT('Ctrl Pts',(9.49947652234889,24.072349866447,-35.9995973318569));
#53930=CARTESIAN_POINT('Ctrl Pts',(9.49947711854897,24.0723086681791,-35.9995977904559));
#53931=CARTESIAN_POINT('Ctrl Pts',(9.49947771424067,24.072267469844,-35.9995982486639));
#53932=CARTESIAN_POINT('Ctrl Pts',(9.49947830942397,24.0722262714417,-35.9995987064809));
#53933=CARTESIAN_POINT('Ctrl Pts',(9.49965176461951,24.060219756981,-35.9997321287929));
#53934=CARTESIAN_POINT('Ctrl Pts',(9.49978204199234,24.0482075968042,-35.9998323411043));
#53935=CARTESIAN_POINT('Ctrl Pts',(9.4998690295622,24.0361896019762,-35.9998992537352));
#53936=CARTESIAN_POINT('Ctrl Pts',(9.49986917252243,24.0361698509338,-35.9998993637031));
#53937=CARTESIAN_POINT('Ctrl Pts',(9.49986931536621,24.0361500999239,-35.9998994735815));
#53938=CARTESIAN_POINT('Ctrl Pts',(9.49986945809355,24.0361303489459,-35.9998995833703));
#53939=CARTESIAN_POINT('Ctrl Pts',(9.49991295239155,24.0301114956676,-35.9999330400806));
#53940=CARTESIAN_POINT('Ctrl Pts',(9.49994564654914,24.024091208166,-35.9999581449458));
#53941=CARTESIAN_POINT('Ctrl Pts',(9.49996740821826,24.0180694839239,-35.9999748847169));
#53942=CARTESIAN_POINT('Ctrl Pts',(9.49997828905281,24.0150586218028,-35.9999832546024));
#53943=CARTESIAN_POINT('Ctrl Pts',(9.49998644052914,24.0120474005484,-35.9999895333668));
#53944=CARTESIAN_POINT('Ctrl Pts',(9.49999186825306,24.0090358199681,-35.9999937197092));
#53945=CARTESIAN_POINT('Ctrl Pts',(9.49999458211502,24.0075300296779,-35.9999958128805));
#53946=CARTESIAN_POINT('Ctrl Pts',(9.49999661789029,24.0060222106567,-35.999997382956));
#53947=CARTESIAN_POINT('Ctrl Pts',(9.49999797235682,24.0045152712213,-35.9999984297334));
#53948=CARTESIAN_POINT('Ctrl Pts',(9.49999932682335,24.0030083317859,-35.9999994765107));
#53949=CARTESIAN_POINT('Ctrl Pts',(9.5,24.0015022719398,-36.));
#53950=CARTESIAN_POINT('Ctrl Pts',(9.5,24.,-36.));
#53951=CARTESIAN_POINT('Ctrl Pts',(9.5,23.9999999737538,-36.));
#53952=CARTESIAN_POINT('Ctrl Pts',(9.49999999993673,23.9879832282049,-35.999999999951));
#53953=CARTESIAN_POINT('Ctrl Pts',(9.49995667919472,23.9759763925916,-35.9999666761675));
#53954=CARTESIAN_POINT('Ctrl Pts',(9.4998702522827,23.9639797232321,-35.9999001945923));
#53955=CARTESIAN_POINT('Ctrl Pts',(9.49986975477033,23.9639106649817,-35.9998998118944));
#53956=CARTESIAN_POINT('Ctrl Pts',(9.49986925582743,23.9638416067762,-35.999899428096));
#53957=CARTESIAN_POINT('Ctrl Pts',(9.49986875545392,23.9637725486055,-35.9998990431972));
#53958=CARTESIAN_POINT('Ctrl Pts',(9.4997819986771,23.9517989644353,-35.9998323078902));
#53959=CARTESIAN_POINT('Ctrl Pts',(9.49965230110543,23.9398353051175,-35.999732542221));
#53960=CARTESIAN_POINT('Ctrl Pts',(9.49947986548288,23.9278815245469,-35.9995999050319));
#53961=CARTESIAN_POINT('Ctrl Pts',(9.49913150351934,23.9037319758056,-35.9993319455991));
#53962=CARTESIAN_POINT('Ctrl Pts',(9.49860871944609,23.8796227420958,-35.9989298298439));
#53963=CARTESIAN_POINT('Ctrl Pts',(9.4979130841039,23.8555534571282,-35.9983948168954));
#53964=CARTESIAN_POINT('Ctrl Pts',(9.49652417723533,23.8074966762467,-35.9973266090085));
#53965=CARTESIAN_POINT('Ctrl Pts',(9.49444633029436,23.7595991165855,-35.9957286757378));
#53966=CARTESIAN_POINT('Ctrl Pts',(9.49169052182656,23.7118581368826,-35.9936102643782));
#53967=CARTESIAN_POINT('Ctrl Pts',(9.49166437530495,23.7114051806732,-35.9935901653441));
#53968=CARTESIAN_POINT('Ctrl Pts',(9.49163816771039,23.7109522385841,-35.9935700194233));
#53969=CARTESIAN_POINT('Ctrl Pts',(9.49161189904947,23.7104993106094,-35.9935498266216));
#53970=CARTESIAN_POINT('Ctrl Pts',(9.48730051343738,23.6361617888405,-35.9902356510239));
#53971=CARTESIAN_POINT('Ctrl Pts',(9.48134411968866,23.5622032194035,-35.985658281014));
#53972=CARTESIAN_POINT('Ctrl Pts',(9.4737793415769,23.4886172124655,-35.9798518103728));
#53973=CARTESIAN_POINT('Ctrl Pts',(9.47168117086805,23.4682073601132,-35.9782413247193));
#53974=CARTESIAN_POINT('Ctrl Pts',(9.46945903056611,23.4478260956439,-35.9765361006218));
#53975=CARTESIAN_POINT('Ctrl Pts',(9.46711315648697,23.4274731548101,-35.9747364429526));
#53976=CARTESIAN_POINT('Ctrl Pts',(9.46682390991277,23.4249636346004,-35.9745145449317));
#53977=CARTESIAN_POINT('Ctrl Pts',(9.46653278205061,23.4224545465678,-35.9742912113484));
#53978=CARTESIAN_POINT('Ctrl Pts',(9.46623977303,23.4199458895996,-35.9740664425365));
#53979=CARTESIAN_POINT('Ctrl Pts',(9.45768749974971,23.3467238436917,-35.9675059472304));
#53980=CARTESIAN_POINT('Ctrl Pts',(9.44753564796578,23.2738705364315,-35.9597251325201));
#53981=CARTESIAN_POINT('Ctrl Pts',(9.43580765437234,23.2013794401489,-35.9507515376106));
#53982=CARTESIAN_POINT('Ctrl Pts',(9.43285767755637,23.1831455409151,-35.9484943828186));
#53983=CARTESIAN_POINT('Ctrl Pts',(9.42980777681206,23.1649345853686,-35.9461616054021));
#53984=CARTESIAN_POINT('Ctrl Pts',(9.4266579217613,23.1467465545623,-35.9437533337836));
#53985=CARTESIAN_POINT('Ctrl Pts',(9.42576245566971,23.1415759150893,-35.9430686909861));
#53986=CARTESIAN_POINT('Ctrl Pts',(9.42485891395591,23.1364071539974,-35.9423779507369));
#53987=CARTESIAN_POINT('Ctrl Pts',(9.42394729195393,23.1312402617232,-35.9416811131217));
#53988=CARTESIAN_POINT('Ctrl Pts',(9.41145567335541,23.0604402508758,-35.9321326054124));
#53989=CARTESIAN_POINT('Ctrl Pts',(9.3974493622803,22.989987995806,-35.9214411733268));
#53990=CARTESIAN_POINT('Ctrl Pts',(9.38193889031453,22.919878173417,-35.9096276267171));
#53991=CARTESIAN_POINT('Ctrl Pts',(9.37822780110102,22.9031034546204,-35.9068010766616));
#53992=CARTESIAN_POINT('Ctrl Pts',(9.37443043919327,22.8863484537643,-35.9039101676379));
#53993=CARTESIAN_POINT('Ctrl Pts',(9.37054664849344,22.869613341837,-35.9009549643899));
#53994=CARTESIAN_POINT('Ctrl Pts',(9.36883796974234,22.8622507076588,-35.8996548188916));
#53995=CARTESIAN_POINT('Ctrl Pts',(9.36711255863853,22.8548919158162,-35.8983422262096));
#53996=CARTESIAN_POINT('Ctrl Pts',(9.36537039239681,22.847536978434,-35.8970171856514));
#53997=CARTESIAN_POINT('Ctrl Pts',(9.3491022086485,22.7788572681249,-35.8846440821217));
#53998=CARTESIAN_POINT('Ctrl Pts',(9.33137622497279,22.7105113237437,-35.8711879248514));
#53999=CARTESIAN_POINT('Ctrl Pts',(9.31218977679271,22.6424941274949,-35.8566633015094));
#54000=CARTESIAN_POINT('Ctrl Pts',(9.3078168676122,22.6269918824146,-35.8533528993881));
#54001=CARTESIAN_POINT('Ctrl Pts',(9.30336798785164,22.61150688569,-35.8499869250491));
#54002=CARTESIAN_POINT('Ctrl Pts',(9.29884292932156,22.5960394019589,-35.8465654366677));
#54003=CARTESIAN_POINT('Ctrl Pts',(9.29649960113552,22.5880294744954,-35.8447935987767));
#54004=CARTESIAN_POINT('Ctrl Pts',(9.29413504811975,22.5800215351618,-35.8430062534732));
#54005=CARTESIAN_POINT('Ctrl Pts',(9.29175146133901,22.5720231168623,-35.841205088392));
#54006=CARTESIAN_POINT('Ctrl Pts',(9.29076497192281,22.5687128304224,-35.8404596444653));
#54007=CARTESIAN_POINT('Ctrl Pts',(9.28977522583305,22.5654041754969,-35.8397118364184));
#54008=CARTESIAN_POINT('Ctrl Pts',(9.28878238789472,22.5620976773719,-35.8389617909375));
#54009=CARTESIAN_POINT('Ctrl Pts',(9.28539062367664,22.5508019143933,-35.8363994619553));
#54010=CARTESIAN_POINT('Ctrl Pts',(9.28196280007465,22.5395313504075,-35.83381102518));
#54011=CARTESIAN_POINT('Ctrl Pts',(9.27849919458226,22.5282857541102,-35.8311967941509));
#54012=CARTESIAN_POINT('Ctrl Pts',(9.27157198359749,22.5057945615158,-35.8259683320927));
#54013=CARTESIAN_POINT('Ctrl Pts',(9.26450166607527,22.4834032284448,-35.8206367170279));
#54014=CARTESIAN_POINT('Ctrl Pts',(9.25729019799672,22.4611101419525,-35.8152042084262));
#54015=CARTESIAN_POINT('Ctrl Pts',(9.24286726183961,22.416523968968,-35.8043391912229));
#54016=CARTESIAN_POINT('Ctrl Pts',(9.22787987878537,22.3723306029726,-35.7930710047512));
#54017=CARTESIAN_POINT('Ctrl Pts',(9.21234040799164,22.328519572134,-35.7814132280349));
#54018=CARTESIAN_POINT('Ctrl Pts',(9.20984952418266,22.3214969271019,-35.7795445564658));
#54019=CARTESIAN_POINT('Ctrl Pts',(9.20734448156848,22.3144842554121,-35.777665909801));
#54020=CARTESIAN_POINT('Ctrl Pts',(9.20482529266609,22.3074814655873,-35.7757773219761));
#54021=CARTESIAN_POINT('Ctrl Pts',(9.18941669728238,22.2646489670536,-35.7642257921909));
#54022=CARTESIAN_POINT('Ctrl Pts',(9.17347821168039,22.2221793804084,-35.7523018030587));
#54023=CARTESIAN_POINT('Ctrl Pts',(9.15702114870064,22.1800673676922,-35.740019618893));
#54024=CARTESIAN_POINT('Ctrl Pts',(9.14259793406756,22.143159773744,-35.7292553301129));
#54025=CARTESIAN_POINT('Ctrl Pts',(9.12777686460726,22.1065281322112,-35.7182162688711));
#54026=CARTESIAN_POINT('Ctrl Pts',(9.11256256614464,22.0701639208216,-35.7069100481183));
#54027=CARTESIAN_POINT('Ctrl Pts',(9.11062517609986,22.0655332990874,-35.7054703130175));
#54028=CARTESIAN_POINT('Ctrl Pts',(9.10868143263058,22.0609070795274,-35.7040262625053));
#54029=CARTESIAN_POINT('Ctrl Pts',(9.10673134009715,22.056285242096,-35.7025779089919));
#54030=CARTESIAN_POINT('Ctrl Pts',(9.08972898401151,22.0159886282527,-35.6899500865939));
#54031=CARTESIAN_POINT('Ctrl Pts',(9.07224401686274,21.9760239385094,-35.6769951131352));
#54032=CARTESIAN_POINT('Ctrl Pts',(9.05428095101055,21.9363805796518,-35.6637224850983));
#54033=CARTESIAN_POINT('Ctrl Pts',(9.03664587444707,21.8974610725676,-35.6506922032102));
#54034=CARTESIAN_POINT('Ctrl Pts',(9.01854981494461,21.8588511000046,-35.6373556303559));
#54035=CARTESIAN_POINT('Ctrl Pts',(9.00000000000002,21.8205505282297,-35.6237243569579));
#54036=CARTESIAN_POINT('Origin',(4.5000000000009,23.9999999999992,-38.6923881554236));
#54037=CARTESIAN_POINT('Origin',(0.5,48.5249973351313,-4.97500266486866));
#54038=CARTESIAN_POINT('',(0.499999999643868,29.0827333318928,-17.3461988580058));
#54039=CARTESIAN_POINT('Origin',(0.39600932023275,31.6849458844993,-16.7453161466531));
#54040=CARTESIAN_POINT('',(0.500000000000045,27.0000000000001,-19.4289321881344));
#54041=CARTESIAN_POINT('',(0.500000000000001,44.9894634291986,-1.43946875893592));
#54042=CARTESIAN_POINT('Ctrl Pts',(0.500000000000087,27.0000000000001,-19.4289321881344));
#54043=CARTESIAN_POINT('Ctrl Pts',(0.630063764891852,27.1734183531891,-19.2555138349454));
#54044=CARTESIAN_POINT('Ctrl Pts',(0.773900537595572,27.3419476067783,-19.0939257507809));
#54045=CARTESIAN_POINT('Ctrl Pts',(1.0711763811429,27.6443407962334,-18.8281986778164));
#54046=CARTESIAN_POINT('Ctrl Pts',(1.23509725261859,27.7938951449731,-18.7069951671099));
#54047=CARTESIAN_POINT('Ctrl Pts',(1.59835434231765,28.0784412787328,-18.5182617650791));
#54048=CARTESIAN_POINT('Ctrl Pts',(1.79823937131942,28.2134034590434,-18.4517453020891));
#54049=CARTESIAN_POINT('Ctrl Pts',(2.13279052698853,28.4069534387743,-18.406567444179));
#54050=CARTESIAN_POINT('Ctrl Pts',(2.27824207369039,28.4822099736569,-18.4051451043186));
#54051=CARTESIAN_POINT('Ctrl Pts',(2.5740138256679,28.6170327901994,-18.4449321123119));
#54052=CARTESIAN_POINT('Ctrl Pts',(2.72431574730796,28.6766212956434,-18.4862020423829));
#54053=CARTESIAN_POINT('Ctrl Pts',(3.16223201946421,28.8276016861915,-18.6686564412896));
#54054=CARTESIAN_POINT('Ctrl Pts',(3.43743466557115,28.8911112631435,-18.8720368348926));
#54055=CARTESIAN_POINT('Ctrl Pts',(4.00248687235112,28.9871400474885,-19.4284741379288));
#54056=CARTESIAN_POINT('Ctrl Pts',(4.27125162606028,28.9999868518442,-19.8261269612256));
#54057=CARTESIAN_POINT('Ctrl Pts',(4.72816585783078,29.0000131311922,-20.6874933896537));
#54058=CARTESIAN_POINT('Ctrl Pts',(4.91347393380979,28.9851063276177,-21.1527100259297));
#54059=CARTESIAN_POINT('Ctrl Pts',(5.35782996082894,28.9348711666866,-22.6030865324071));
#54060=CARTESIAN_POINT('Ctrl Pts',(5.5,28.8989794855664,-23.6390951228936));
#54061=CARTESIAN_POINT('Ctrl Pts',(5.5,28.8989794855664,-24.8083397544018));
#54062=CARTESIAN_POINT('Ctrl Pts',(5.49353975798667,28.900313920569,-25.0194149375122));
#54063=CARTESIAN_POINT('Ctrl Pts',(5.47974928497603,28.9030695832906,-25.2326930434511));
#54064=CARTESIAN_POINT('',(-0.474937185533102,24.5,-22.0646561030811));
#54065=CARTESIAN_POINT('Origin',(0.500000000032158,24.5000000000003,-29.0000000001026));
#54066=CARTESIAN_POINT('Ctrl Pts',(-0.4749371855331,24.5,-22.0646561030811));
#54067=CARTESIAN_POINT('Ctrl Pts',(-0.430283424779195,24.944299309697,-21.6078023728738));
#54068=CARTESIAN_POINT('Ctrl Pts',(-0.32422833575544,25.394363859076,-21.1270657168025));
#54069=CARTESIAN_POINT('Ctrl Pts',(0.00642096108058736,26.2359626137404,
-20.2237995433534));
#54070=CARTESIAN_POINT('Ctrl Pts',(0.22196880373164,26.6292917383089,-19.7996404498256));
#54071=CARTESIAN_POINT('Ctrl Pts',(0.500000000000088,27.0000000000001,-19.4289321881344));
#54072=CARTESIAN_POINT('Ctrl Pts',(0.499999999661276,29.0827333318934,-17.3461988580053));
#54073=CARTESIAN_POINT('Ctrl Pts',(0.494640286720631,29.0825598614636,-17.3463723338252));
#54074=CARTESIAN_POINT('Ctrl Pts',(0.489278323252304,29.0824021998227,-17.346542198886));
#54075=CARTESIAN_POINT('Ctrl Pts',(0.483914104352405,29.0822603694729,-17.3467084484518));
#54076=CARTESIAN_POINT('Ctrl Pts',(0.47082609449057,29.0819143215112,-17.3471140761857));
#54077=CARTESIAN_POINT('Ctrl Pts',(0.457724658694381,29.081662489745,-17.3474981872329));
#54078=CARTESIAN_POINT('Ctrl Pts',(0.444609710549237,29.0815054764053,-17.347860648805));
#54079=CARTESIAN_POINT('Ctrl Pts',(0.438786451655717,29.0814357598256,-17.3480215878762));
#54080=CARTESIAN_POINT('Ctrl Pts',(0.432961830886728,29.0813847595728,-17.3481782214898));
#54081=CARTESIAN_POINT('Ctrl Pts',(0.427137031146438,29.081352531438,-17.3483305042711));
#54082=CARTESIAN_POINT('Ctrl Pts',(0.419843412498221,29.0813121764498,-17.3485211876565));
#54083=CARTESIAN_POINT('Ctrl Pts',(0.412554916938757,29.0813012192184,-17.3487049200745));
#54084=CARTESIAN_POINT('Ctrl Pts',(0.405272700896496,29.0813195495914,-17.3488816941982));
#54085=CARTESIAN_POINT('Ctrl Pts',(0.310866975848777,29.0815571822215,-17.3511733715135));
#54086=CARTESIAN_POINT('Ctrl Pts',(0.217320839007321,29.0867132990217,-17.3523038451532));
#54087=CARTESIAN_POINT('Ctrl Pts',(0.124594312162254,29.0965585511847,-17.3523322354303));
#54088=CARTESIAN_POINT('Ctrl Pts',(0.114401347256358,29.0976407906818,-17.352335356232));
#54089=CARTESIAN_POINT('Ctrl Pts',(0.104218288490283,29.0987797030209,-17.3523251576095));
#54090=CARTESIAN_POINT('Ctrl Pts',(0.0940450941988781,29.0999750546262,
-17.3523017088945));
#54091=CARTESIAN_POINT('Ctrl Pts',(0.0043183856975315,29.11051795413,-17.3520948932218));
#54092=CARTESIAN_POINT('Ctrl Pts',(-0.0846413778766092,29.1254494642378,
-17.3508590735705));
#54093=CARTESIAN_POINT('Ctrl Pts',(-0.172861973304381,29.1446114053705,
-17.3486408804781));
#54094=CARTESIAN_POINT('Ctrl Pts',(-0.185637033054331,29.147386210298,-17.348319668077));
#54095=CARTESIAN_POINT('Ctrl Pts',(-0.198396589790223,29.1502497370368,
-17.3479778528971));
#54096=CARTESIAN_POINT('Ctrl Pts',(-0.211140707083288,29.1532016314949,
-17.347615561321));
#54097=CARTESIAN_POINT('Ctrl Pts',(-0.296585498060996,29.1729930379266,
-17.3451865246695));
#54098=CARTESIAN_POINT('Ctrl Pts',(-0.381332734630402,29.1967542444877,
-17.3418385994444));
#54099=CARTESIAN_POINT('Ctrl Pts',(-0.465406902219237,29.2243801498567,
-17.3376101192265));
#54100=CARTESIAN_POINT('Ctrl Pts',(-0.480467616897809,29.2293289455502,
-17.3368526459632));
#54101=CARTESIAN_POINT('Ctrl Pts',(-0.495512841578221,29.2344040610324,
-17.3360665540002));
#54102=CARTESIAN_POINT('Ctrl Pts',(-0.510530623365413,29.2396007024458,
-17.3352527344234));
#54103=CARTESIAN_POINT('Ctrl Pts',(-0.519625874270915,29.2427479553617,
-17.334759859154));
#54104=CARTESIAN_POINT('Ctrl Pts',(-0.528715062171632,29.2459411878691,
-17.33425659577));
#54105=CARTESIAN_POINT('Ctrl Pts',(-0.537788620983005,29.2491769241415,
-17.333743521862));
#54106=CARTESIAN_POINT('Ctrl Pts',(-0.553369192460061,29.2547331365738,
-17.3328625020919));
#54107=CARTESIAN_POINT('Ctrl Pts',(-0.56887579523059,29.2604044022829,-17.3319542053377));
#54108=CARTESIAN_POINT('Ctrl Pts',(-0.584317019483223,29.2661908253089,
-17.3310189205406));
#54109=CARTESIAN_POINT('Ctrl Pts',(-0.592741616178843,29.269347847026,-17.3305086373479));
#54110=CARTESIAN_POINT('Ctrl Pts',(-0.601146149580129,29.2725389392175,
-17.3299903501898));
#54111=CARTESIAN_POINT('Ctrl Pts',(-0.609530854384228,29.2757637100109,
-17.3294641714673));
#54112=CARTESIAN_POINT('Ctrl Pts',(-0.625464084497629,29.2818916556352,
-17.3284642881247));
#54113=CARTESIAN_POINT('Ctrl Pts',(-0.641325740152662,29.2881411628421,
-17.3274359196832));
#54114=CARTESIAN_POINT('Ctrl Pts',(-0.657117305180762,29.2945097885707,
-17.3263797807976));
#54115=CARTESIAN_POINT('Ctrl Pts',(-0.688504756412231,29.3071681241512,
-17.3242805900141));
#54116=CARTESIAN_POINT('Ctrl Pts',(-0.719615331526967,29.3202969521538,
-17.3220717772427));
#54117=CARTESIAN_POINT('Ctrl Pts',(-0.750460137429674,29.3338774655774,
-17.3197586170282));
#54118=CARTESIAN_POINT('Ctrl Pts',(-0.766985401130791,29.3411532956225,
-17.3185193295239));
#54119=CARTESIAN_POINT('Ctrl Pts',(-0.783434470810792,29.3485585979443,
-17.317250129809));
#54120=CARTESIAN_POINT('Ctrl Pts',(-0.799808799112829,29.3560909668914,
-17.3159517170646));
#54121=CARTESIAN_POINT('Ctrl Pts',(-0.875661422642261,29.3909839979513,
-17.3099369351898));
#54122=CARTESIAN_POINT('Ctrl Pts',(-0.949912389395401,29.4286007159882,
-17.3032985351734));
#54123=CARTESIAN_POINT('Ctrl Pts',(-1.0227011139135,29.4687058692772,-17.2961057417184));
#54124=CARTESIAN_POINT('Ctrl Pts',(-1.03999534287283,29.4782346487416,-17.2943967707522));
#54125=CARTESIAN_POINT('Ctrl Pts',(-1.05720697183354,29.4879040019624,-17.2926564778399));
#54126=CARTESIAN_POINT('Ctrl Pts',(-1.07433751090772,29.497711457383,-17.290885634723));
#54127=CARTESIAN_POINT('Ctrl Pts',(-1.14527573158552,29.5383245072059,-17.2835525053174));
#54128=CARTESIAN_POINT('Ctrl Pts',(-1.21482462488908,29.5813034463345,-17.2756979414421));
#54129=CARTESIAN_POINT('Ctrl Pts',(-1.28308743240194,29.6264749237948,-17.2673765449636));
#54130=CARTESIAN_POINT('Ctrl Pts',(-1.30068964917242,29.6381228206082,-17.2652307934192));
#54131=CARTESIAN_POINT('Ctrl Pts',(-1.31820631057408,29.6499165781555,-17.2630539809597));
#54132=CARTESIAN_POINT('Ctrl Pts',(-1.33563885933988,29.6618538487408,-17.2608469041224));
#54133=CARTESIAN_POINT('Ctrl Pts',(-1.37815754441842,29.6909693301048,-17.255463755264));
#54134=CARTESIAN_POINT('Ctrl Pts',(-1.4201760084857,29.7209380445501,-17.2499011197985));
#54135=CARTESIAN_POINT('Ctrl Pts',(-1.46171476117621,29.7517257912023,-17.2441709839974));
#54136=CARTESIAN_POINT('Ctrl Pts',(-1.48248413752148,29.7671196645284,-17.2413059160968));
#54137=CARTESIAN_POINT('Ctrl Pts',(-1.50313358222067,29.7827183009981,-17.2383989778656));
#54138=CARTESIAN_POINT('Ctrl Pts',(-1.5236655210333,29.7985176702096,-17.2354514018751));
#54139=CARTESIAN_POINT('Ctrl Pts',(-1.52663299972461,29.8008011511755,-17.2350253890654));
#54140=CARTESIAN_POINT('Ctrl Pts',(-1.52959787132464,29.8030887060471,-17.2345985510579));
#54141=CARTESIAN_POINT('Ctrl Pts',(-1.53256022149386,29.8053803805644,-17.2341708817701));
#54142=CARTESIAN_POINT('Ctrl Pts',(-1.53984609864872,29.8110167361801,-17.2331190324899));
#54143=CARTESIAN_POINT('Ctrl Pts',(-1.54711863018462,29.8166796254338,-17.2320618519711));
#54144=CARTESIAN_POINT('Ctrl Pts',(-1.55437552343597,29.8223668935654,-17.2309997792847));
#54145=CARTESIAN_POINT('Ctrl Pts',(-1.56458298234939,29.830366536632,-17.2295058805964));
#54146=CARTESIAN_POINT('Ctrl Pts',(-1.57476243074193,29.8384167611187,-17.2280018638832));
#54147=CARTESIAN_POINT('Ctrl Pts',(-1.58489488875909,29.8465016671252,-17.2264907639462));
#54148=CARTESIAN_POINT('Ctrl Pts',(-1.58769371888662,29.8487349138331,-17.2260733615723));
#54149=CARTESIAN_POINT('Ctrl Pts',(-1.59048933583235,29.850971097859,-17.2256553663614));
#54150=CARTESIAN_POINT('Ctrl Pts',(-1.59328153837513,29.8532100410182,-17.2252368133482));
#54151=CARTESIAN_POINT('Ctrl Pts',(-1.61339119892336,29.8693350843224,-17.2222223618943));
#54152=CARTESIAN_POINT('Ctrl Pts',(-1.63333460185478,29.8856111808793,-17.2191774998543));
#54153=CARTESIAN_POINT('Ctrl Pts',(-1.65311698743174,29.9020332378137,-17.216103830654));
#54154=CARTESIAN_POINT('Ctrl Pts',(-1.69274299677892,29.9349281876693,-17.2099469774278));
#54155=CARTESIAN_POINT('Ctrl Pts',(-1.7317232430286,29.9684084814715,-17.2036746162589));
#54156=CARTESIAN_POINT('Ctrl Pts',(-1.77009588134444,30.0024371988237,-17.1972985702881));
#54157=CARTESIAN_POINT('Ctrl Pts',(-1.78694210817751,30.0173763720605,-17.1944993799943));
#54158=CARTESIAN_POINT('Ctrl Pts',(-1.80367137995709,30.0324210900912,-17.1916802447701));
#54159=CARTESIAN_POINT('Ctrl Pts',(-1.82028640118399,30.0475687611652,-17.188842026926));
#54160=CARTESIAN_POINT('Ctrl Pts',(-1.87958806677336,30.1016332195985,-17.1787119739361));
#54161=CARTESIAN_POINT('Ctrl Pts',(-1.93743845715215,30.1570108336236,-17.1683398926932));
#54162=CARTESIAN_POINT('Ctrl Pts',(-1.99396211476126,30.213591260895,-17.1577624007788));
#54163=CARTESIAN_POINT('Ctrl Pts',(-2.00985737737727,30.2295024879537,-17.154787858456));
#54164=CARTESIAN_POINT('Ctrl Pts',(-2.02564765372924,30.245508900131,-17.1517970533222));
#54165=CARTESIAN_POINT('Ctrl Pts',(-2.04133516140658,30.2616086006945,-17.1487906572123));
#54166=CARTESIAN_POINT('Ctrl Pts',(-2.09731775608623,30.3190621509747,-17.1380620023916));
#54167=CARTESIAN_POINT('Ctrl Pts',(-2.15199317849248,30.3777023875684,-17.1271371965694));
#54168=CARTESIAN_POINT('Ctrl Pts',(-2.20545904914118,30.4374432811992,-17.1160465937905));
#54169=CARTESIAN_POINT('Ctrl Pts',(-2.22025249087105,30.4539729555147,-17.1129779411347));
#54170=CARTESIAN_POINT('Ctrl Pts',(-2.23495328877808,30.4705869355724,-17.1098965827622));
#54171=CARTESIAN_POINT('Ctrl Pts',(-2.24956311487717,30.487283798179,-17.1068030622022));
#54172=CARTESIAN_POINT('Ctrl Pts',(-2.30276895690595,30.5480901779536,-17.095537126173));
#54173=CARTESIAN_POINT('Ctrl Pts',(-2.35476946268512,30.6099946764907,-17.0841119019788));
#54174=CARTESIAN_POINT('Ctrl Pts',(-2.40564340906758,30.6729284032563,-17.0725540010902));
#54175=CARTESIAN_POINT('Ctrl Pts',(-2.41922701910644,30.6897320377974,-17.0694679810406));
#54176=CARTESIAN_POINT('Ctrl Pts',(-2.43273028540881,30.7066090763658,-17.0663724934113));
#54177=CARTESIAN_POINT('Ctrl Pts',(-2.44615442796957,30.7235584904524,-17.063267977535));
#54178=CARTESIAN_POINT('Ctrl Pts',(-2.49700159070261,30.7877584654149,-17.0515088783408));
#54179=CARTESIAN_POINT('Ctrl Pts',(-2.54670382627324,30.8529820325238,-17.0396241050726));
#54180=CARTESIAN_POINT('Ctrl Pts',(-2.59535135150116,30.9192065689568,-17.0276321672655));
#54181=CARTESIAN_POINT('Ctrl Pts',(-2.60764898540964,30.9359475049242,-17.0246007188965));
#54182=CARTESIAN_POINT('Ctrl Pts',(-2.61988188181737,30.9527567274417,-17.0215616539119));
#54183=CARTESIAN_POINT('Ctrl Pts',(-2.63204242319319,30.969621047708,-17.0185175583762));
#54184=CARTESIAN_POINT('Ctrl Pts',(-2.64710886066503,30.9905152841523,-17.0147460424847));
#54185=CARTESIAN_POINT('Ctrl Pts',(-2.66205735353112,31.0114844768585,-17.0109685635766));
#54186=CARTESIAN_POINT('Ctrl Pts',(-2.67687815179317,31.03250984723,-17.0071889049466));
#54187=CARTESIAN_POINT('Ctrl Pts',(-2.68005872862648,31.0370219392735,-17.0063777816546));
#54188=CARTESIAN_POINT('Ctrl Pts',(-2.68323362145371,31.041536899362,-17.005566508625));
#54189=CARTESIAN_POINT('Ctrl Pts',(-2.68640262874064,31.0460543999021,-17.0047551487455));
#54190=CARTESIAN_POINT('Ctrl Pts',(-2.69800050813871,31.0625874721551,-17.0017857475485));
#54191=CARTESIAN_POINT('Ctrl Pts',(-2.70952411185291,31.07916060295,-16.9988140852021));
#54192=CARTESIAN_POINT('Ctrl Pts',(-2.72097236568739,31.0957696486511,-16.9958410668479));
#54193=CARTESIAN_POINT('Ctrl Pts',(-2.73902544468637,31.1219609279916,-16.9911528291488));
#54194=CARTESIAN_POINT('Ctrl Pts',(-2.75689333580946,31.1482446123294,-16.9864606814935));
#54195=CARTESIAN_POINT('Ctrl Pts',(-2.77458131746985,31.174618216052,-16.9817655560967));
#54196=CARTESIAN_POINT('Ctrl Pts',(-2.78545651842152,31.1908336467217,-16.9788788258205));
#54197=CARTESIAN_POINT('Ctrl Pts',(-2.79626404107529,31.2070828865657,-16.9759910156415));
#54198=CARTESIAN_POINT('Ctrl Pts',(-2.80700482713285,31.2233655128358,-16.9731023015609));
#54199=CARTESIAN_POINT('Ctrl Pts',(-2.863425124086,31.3088965535259,-16.9579281694845));
#54200=CARTESIAN_POINT('Ctrl Pts',(-2.91800594098433,31.3953483978114,-16.942731525384));
#54201=CARTESIAN_POINT('Ctrl Pts',(-2.970888038649,31.4826568738121,-16.9275498795692));
#54202=CARTESIAN_POINT('Ctrl Pts',(-3.01520349115017,31.5558217971419,-16.9148275872679));
#54203=CARTESIAN_POINT('Ctrl Pts',(-3.05832507044605,31.6295884628099,-16.9021146309357));
#54204=CARTESIAN_POINT('Ctrl Pts',(-3.10033004290332,31.7039199616385,-16.8894266815057));
#54205=CARTESIAN_POINT('Ctrl Pts',(-3.10845004786398,31.7182890256781,-16.8869739668321));
#54206=CARTESIAN_POINT('Ctrl Pts',(-3.11652825402692,31.732679235635,-16.884522173597));
#54207=CARTESIAN_POINT('Ctrl Pts',(-3.12456502627307,31.7470904300683,-16.8820713900921));
#54208=CARTESIAN_POINT('Ctrl Pts',(-3.17417620622964,31.8360510648259,-16.866942647137));
#54209=CARTESIAN_POINT('Ctrl Pts',(-3.22221018340241,31.9258110668167,-16.8518548517033));
#54210=CARTESIAN_POINT('Ctrl Pts',(-3.26875629613443,32.0163305079745,-16.83683855778));
#54211=CARTESIAN_POINT('Ctrl Pts',(-3.30936706167238,32.09530732442,-16.8237370729089));
#54212=CARTESIAN_POINT('Ctrl Pts',(-3.34884412638437,32.1748628249438,-16.8106877954571));
#54213=CARTESIAN_POINT('Ctrl Pts',(-3.38724441489668,32.2549704657586,-16.7977087994844));
#54214=CARTESIAN_POINT('Ctrl Pts',(-3.43686926623875,32.3584939006287,-16.7809359894178));
#54215=CARTESIAN_POINT('Ctrl Pts',(-3.48469413673384,32.4629403693864,-16.7642801974446));
#54216=CARTESIAN_POINT('Ctrl Pts',(-3.53079737027302,32.5682771939252,-16.7477759907028));
#54217=CARTESIAN_POINT('Ctrl Pts',(-3.56808998530252,32.6534834873756,-16.7344258418925));
#54218=CARTESIAN_POINT('Ctrl Pts',(-3.60425597317371,32.7392723139034,-16.7211747356865));
#54219=CARTESIAN_POINT('Ctrl Pts',(-3.63933555556943,32.8256258069973,-16.7080405816169));
#54220=CARTESIAN_POINT('Ctrl Pts',(-3.67862303088125,32.9223376403865,-16.6933309494459));
#54221=CARTESIAN_POINT('Ctrl Pts',(-3.71654441512108,33.0197596234453,-16.6787677314079));
#54222=CARTESIAN_POINT('Ctrl Pts',(-3.75313710541097,33.1178772474942,-16.6643748421233));
#54223=CARTESIAN_POINT('Ctrl Pts',(-3.75552008359739,33.1242668339378,-16.6634375527102));
#54224=CARTESIAN_POINT('Ctrl Pts',(-3.7578974238126,33.1306593722572,-16.6625009854662));
#54225=CARTESIAN_POINT('Ctrl Pts',(-3.76026913405428,33.1370548597423,-16.6615651469124));
#54226=CARTESIAN_POINT('Ctrl Pts',(-3.77612087232058,33.1798002136719,-16.6553103070276));
#54227=CARTESIAN_POINT('Ctrl Pts',(-3.79172111609674,33.2226772547136,-16.6490880829375));
#54228=CARTESIAN_POINT('Ctrl Pts',(-3.80707222536322,33.265685120324,-16.6429004381211));
#54229=CARTESIAN_POINT('Ctrl Pts',(-3.80898566072384,33.2710458254961,-16.6421291806057));
#54230=CARTESIAN_POINT('Ctrl Pts',(-3.81089522494559,33.2764085634821,-16.6413584603056));
#54231=CARTESIAN_POINT('Ctrl Pts',(-3.81280092196227,33.2817733329664,-16.6405882810111));
#54232=CARTESIAN_POINT('Ctrl Pts',(-3.81968664471756,33.3011574821736,-16.6378054456246));
#54233=CARTESIAN_POINT('Ctrl Pts',(-3.82652219626237,33.3205690601755,-16.6350295440705));
#54234=CARTESIAN_POINT('Ctrl Pts',(-3.83330686070246,33.3400054236625,-16.6322611252416));
#54235=CARTESIAN_POINT('Ctrl Pts',(-3.83499337862771,33.3448368749026,-16.6315729573859));
#54236=CARTESIAN_POINT('Ctrl Pts',(-3.83667686763365,33.3496701967109,-16.6308852041413));
#54237=CARTESIAN_POINT('Ctrl Pts',(-3.83835723509096,33.3545051076029,-16.6301979077439));
#54238=CARTESIAN_POINT('Ctrl Pts',(-3.8453096925068,33.3745093703251,-16.6273542446429));
#54239=CARTESIAN_POINT('Ctrl Pts',(-3.85221059805588,33.394546274598,-16.624517627869));
#54240=CARTESIAN_POINT('Ctrl Pts',(-3.85905346708592,33.4145963041088,-16.6216909852044));
#54241=CARTESIAN_POINT('Ctrl Pts',(-3.86051784694518,33.4188870276729,-16.6210860812425));
#54242=CARTESIAN_POINT('Ctrl Pts',(-3.86197953399095,33.4231782177245,-16.6204816524728));
#54243=CARTESIAN_POINT('Ctrl Pts',(-3.86343852387851,33.4274698499442,-16.6198777034043));
#54244=CARTESIAN_POINT('Ctrl Pts',(-3.89654521281925,33.5248534810153,-16.6061731848763));
#54245=CARTESIAN_POINT('Ctrl Pts',(-3.92827659709283,33.6225047869756,-16.5927095724306));
#54246=CARTESIAN_POINT('Ctrl Pts',(-3.9586750328472,33.7204187298343,-16.5795043418062));
#54247=CARTESIAN_POINT('Ctrl Pts',(-3.98912619588366,33.818502508277,-16.5662762061901));
#54248=CARTESIAN_POINT('Ctrl Pts',(-4.01823929067579,33.9168495280274,-16.5533063835685));
#54249=CARTESIAN_POINT('Ctrl Pts',(-4.04605562710238,34.0154538256492,-16.5406106331751));
#54250=CARTESIAN_POINT('Ctrl Pts',(-4.07377563355854,34.1137166495078,-16.527958849077));
#54251=CARTESIAN_POINT('Ctrl Pts',(-4.10020721787853,34.2122350952638,-16.5155791652252));
#54252=CARTESIAN_POINT('Ctrl Pts',(-4.12537067875558,34.3110072940172,-16.5034870911201));
#54253=CARTESIAN_POINT('Ctrl Pts',(-4.15177288597136,34.414641848556,-16.4907997486376));
#54254=CARTESIAN_POINT('Ctrl Pts',(-4.17677913217847,34.5185557899405,-16.4784293163084));
#54255=CARTESIAN_POINT('Ctrl Pts',(-4.2004125186538,34.622746628846,-16.466393709337));
#54256=CARTESIAN_POINT('Ctrl Pts',(-4.22190650430602,34.7175056427041,-16.4554476198365));
#54257=CARTESIAN_POINT('Ctrl Pts',(-4.24226468159238,34.8124937403118,-16.4447784266551));
#54258=CARTESIAN_POINT('Ctrl Pts',(-4.2614894046433,34.9077119948294,-16.4343999617148));
#54259=CARTESIAN_POINT('Ctrl Pts',(-4.28354054518552,35.0169292307288,-16.4224956555561));
#54260=CARTESIAN_POINT('Ctrl Pts',(-4.30410052030379,35.1264492980322,-16.410974115389));
#54261=CARTESIAN_POINT('Ctrl Pts',(-4.3231726349224,35.2362735924075,-16.3998563832951));
#54262=CARTESIAN_POINT('Ctrl Pts',(-4.33901061063775,35.327474518055,-16.3906239319161));
#54263=CARTESIAN_POINT('Ctrl Pts',(-4.35382253124448,35.4188852436833,-16.3816699084276));
#54264=CARTESIAN_POINT('Ctrl Pts',(-4.36759808576858,35.5105089644624,-16.3730069706139));
#54265=CARTESIAN_POINT('Ctrl Pts',(-4.38486272722525,35.6253392375675,-16.362149874803));
#54266=CARTESIAN_POINT('Ctrl Pts',(-4.40049956209613,35.7405040133384,-16.3517501661194));
#54267=CARTESIAN_POINT('Ctrl Pts',(-4.41448803991512,35.8560093809796,-16.3418329438277));
#54268=CARTESIAN_POINT('Ctrl Pts',(-4.42510172471939,35.9436484780428,-16.334308302984));
#54269=CARTESIAN_POINT('Ctrl Pts',(-4.43476662696607,36.0314836189183,-16.3270613908145));
#54270=CARTESIAN_POINT('Ctrl Pts',(-4.44346276114196,36.1195196258497,-16.320103932916));
#54271=CARTESIAN_POINT('Ctrl Pts',(-4.45536348826696,36.2399975847304,-16.3105825977734));
#54272=CARTESIAN_POINT('Ctrl Pts',(-4.46544989089848,36.3608515237431,-16.3016034223743));
#54273=CARTESIAN_POINT('Ctrl Pts',(-4.47367046250997,36.4820935950479,-16.2931966280678));
#54274=CARTESIAN_POINT('Ctrl Pts',(-4.47937382151229,36.5662102588901,-16.2873640694265));
#54275=CARTESIAN_POINT('Ctrl Pts',(-4.48417755850892,36.6505140455029,-16.2818071352268));
#54276=CARTESIAN_POINT('Ctrl Pts',(-4.4880564954921,36.7350105803116,-16.2765365518856));
#54277=CARTESIAN_POINT('Ctrl Pts',(-4.48901380998959,36.7558641693518,-16.2752357816322));
#54278=CARTESIAN_POINT('Ctrl Pts',(-4.4899147950835,36.7767294974198,-16.2739524535344));
#54279=CARTESIAN_POINT('Ctrl Pts',(-4.49075907137466,36.7976066463568,-16.2726867293248));
#54280=CARTESIAN_POINT('Ctrl Pts',(-4.49200271497388,36.828359295599,-16.2708222806506));
#54281=CARTESIAN_POINT('Ctrl Pts',(-4.49312325344046,36.8591376052184,-16.2689960335866));
#54282=CARTESIAN_POINT('Ctrl Pts',(-4.49411926046787,36.8899418787816,-16.267208522195));
#54283=CARTESIAN_POINT('Ctrl Pts',(-4.49483083024889,36.9119491433798,-16.2659314839267));
#54284=CARTESIAN_POINT('Ctrl Pts',(-4.49547886796317,36.9339707312023,-16.2646741560961));
#54285=CARTESIAN_POINT('Ctrl Pts',(-4.49606277160481,36.9560037243413,-16.2634368980414));
#54286=CARTESIAN_POINT('Ctrl Pts',(-4.49616494674342,36.959859196319,-16.2632203948306));
#54287=CARTESIAN_POINT('Ctrl Pts',(-4.49626515807568,36.9637152028417,-16.2630044973421));
#54288=CARTESIAN_POINT('Ctrl Pts',(-4.49636340186868,36.9675716494597,-16.2627892113485));
#54289=CARTESIAN_POINT('Ctrl Pts',(-4.4970230827126,36.9934666590264,-16.2613436233717));
#54290=CARTESIAN_POINT('Ctrl Pts',(-4.497594172852,37.0193857201734,-16.2599253456985));
#54291=CARTESIAN_POINT('Ctrl Pts',(-4.49807566203265,37.0453111639324,-16.2585356567974));
#54292=CARTESIAN_POINT('Ctrl Pts',(-4.49850557527374,37.0684595377707,-16.2572948279615));
#54293=CARTESIAN_POINT('Ctrl Pts',(-4.49886394922953,37.0916078702396,-16.2560770264095));
#54294=CARTESIAN_POINT('Ctrl Pts',(-4.49915002334757,37.1147399926744,-16.2548832910547));
#54295=CARTESIAN_POINT('Ctrl Pts',(-4.50014552494797,37.1952368410517,-16.2507292436199));
#54296=CARTESIAN_POINT('Ctrl Pts',(-4.50027046440707,37.2756130690668,-16.2468620241585));
#54297=CARTESIAN_POINT('Ctrl Pts',(-4.49951014118622,37.3558963157756,-16.2432842876556));
#54298=CARTESIAN_POINT('Ctrl Pts',(-4.4982747451551,37.4863429490343,-16.2374710738081));
#54299=CARTESIAN_POINT('Ctrl Pts',(-4.49470199172509,37.6165098660978,-16.232423759574));
#54300=CARTESIAN_POINT('Ctrl Pts',(-4.48872744871276,37.7463892347881,-16.2281599037842));
#54301=CARTESIAN_POINT('Ctrl Pts',(-4.48523462831247,37.8223189431529,-16.2256671804988));
#54302=CARTESIAN_POINT('Ctrl Pts',(-4.4809210796152,37.8981503907366,-16.2234422645953));
#54303=CARTESIAN_POINT('Ctrl Pts',(-4.47576652607971,37.9738810433624,-16.2214883404208));
#54304=CARTESIAN_POINT('Ctrl Pts',(-4.46671418296332,38.1068779842761,-16.2180568905526));
#54305=CARTESIAN_POINT('Ctrl Pts',(-4.45506810014391,38.2395642945037,-16.2154611869477));
#54306=CARTESIAN_POINT('Ctrl Pts',(-4.44071727209931,38.3719265373697,-16.213718742802));
#54307=CARTESIAN_POINT('Ctrl Pts',(-4.43291881054213,38.4438542240094,-16.2127718717474));
#54308=CARTESIAN_POINT('Ctrl Pts',(-4.42432191601837,38.5156862467986,-16.2120770179681));
#54309=CARTESIAN_POINT('Ctrl Pts',(-4.41490107380013,38.5874194528047,-16.2116365134872));
#54310=CARTESIAN_POINT('Ctrl Pts',(-4.39718579379342,38.7223090731529,-16.2108081735106));
#54311=CARTESIAN_POINT('Ctrl Pts',(-4.37655716797495,38.8568492198562,-16.2108791369079));
#54312=CARTESIAN_POINT('Ctrl Pts',(-4.35284372957258,38.9910192878985,-16.2118651687503));
#54313=CARTESIAN_POINT('Ctrl Pts',(-4.34074034128895,39.059499969696,-16.2123684414536));
#54314=CARTESIAN_POINT('Ctrl Pts',(-4.32783379023972,39.1278842987629,-16.2131101650123));
#54315=CARTESIAN_POINT('Ctrl Pts',(-4.31409242829866,39.1961684008776,-16.2140917574815));
#54316=CARTESIAN_POINT('Ctrl Pts',(-4.28670714269265,39.332252411093,-16.2160479820706));
#54317=CARTESIAN_POINT('Ctrl Pts',(-4.25600661265602,39.4679377608591,-16.2189567983645));
#54318=CARTESIAN_POINT('Ctrl Pts',(-4.22173771426279,39.603194020185,-16.2228296072566));
#54319=CARTESIAN_POINT('Ctrl Pts',(-4.20889439562926,39.6538854435208,-16.2242810609344));
#54320=CARTESIAN_POINT('Ctrl Pts',(-4.19554849436218,39.7045164220435,-16.2258678031695));
#54321=CARTESIAN_POINT('Ctrl Pts',(-4.18168367496839,39.7550849695418,-16.2275901874348));
#54322=CARTESIAN_POINT('Ctrl Pts',(-4.17761044096032,39.7699410972387,-16.2280961928839));
#54323=CARTESIAN_POINT('Ctrl Pts',(-4.17349241277035,39.7847918356752,-16.2286139046665));
#54324=CARTESIAN_POINT('Ctrl Pts',(-4.16932914922853,39.7996371310629,-16.2291433294851));
#54325=CARTESIAN_POINT('Ctrl Pts',(-4.1664106053186,39.8100440260407,-16.2295144685121));
#54326=CARTESIAN_POINT('Ctrl Pts',(-4.16346987059635,39.820448111608,-16.2298913542028));
#54327=CARTESIAN_POINT('Ctrl Pts',(-4.16050671816335,39.8308496295917,-16.230274002705));
#54328=CARTESIAN_POINT('Ctrl Pts',(-4.15634426034634,39.8454610546936,-16.2308115242418));
#54329=CARTESIAN_POINT('Ctrl Pts',(-4.15213657764192,39.8600706185222,-16.231360554189));
#54330=CARTESIAN_POINT('Ctrl Pts',(-4.1478866429035,39.8746669388683,-16.2319206454273));
#54331=CARTESIAN_POINT('Ctrl Pts',(-4.14479843005341,39.8852733473971,-16.232327635432));
#54332=CARTESIAN_POINT('Ctrl Pts',(-4.14168818815604,39.8958718046634,-16.2327404230012));
#54333=CARTESIAN_POINT('Ctrl Pts',(-4.13855697960968,39.9064582319492,-16.2331588413834));
#54334=CARTESIAN_POINT('Ctrl Pts',(-4.13431153697064,39.920811817515,-16.2337261530824));
#54335=CARTESIAN_POINT('Ctrl Pts',(-4.13002657740077,39.9351468985181,-16.2343039441294));
#54336=CARTESIAN_POINT('Ctrl Pts',(-4.1257014773501,39.9494648091859,-16.2348922103134));
#54337=CARTESIAN_POINT('Ctrl Pts',(-4.11067135817129,39.9992208613485,-16.2369364892322));
#54338=CARTESIAN_POINT('Ctrl Pts',(-4.09515994998905,40.0487579808328,-16.2391068321293));
#54339=CARTESIAN_POINT('Ctrl Pts',(-4.07915897210243,40.0980728016392,-16.2414006596024));
#54340=CARTESIAN_POINT('Ctrl Pts',(-4.06752785387619,40.1339197676915,-16.2430680438534));
#54341=CARTESIAN_POINT('Ctrl Pts',(-4.05563806503628,40.1696492375032,-16.244800674657));
#54342=CARTESIAN_POINT('Ctrl Pts',(-4.04348641224067,40.2052599000481,-16.2465975564644));
#54343=CARTESIAN_POINT('Ctrl Pts',(-4.02220390610394,40.2676287116735,-16.2497446302605));
#54344=CARTESIAN_POINT('Ctrl Pts',(-4.00011953136804,40.3296336871105,-16.2530891515926));
#54345=CARTESIAN_POINT('Ctrl Pts',(-3.97721133125741,40.391265705422,-16.2566245299766));
#54346=CARTESIAN_POINT('Ctrl Pts',(-3.9278482247377,40.5240717692003,-16.2642426430939));
#54347=CARTESIAN_POINT('Ctrl Pts',(-3.87466018715068,40.6551461600849,-16.2727469451434));
#54348=CARTESIAN_POINT('Ctrl Pts',(-3.81742461158264,40.7843965617411,-16.2820708005939));
#54349=CARTESIAN_POINT('Ctrl Pts',(-3.79120522380902,40.843605652718,-16.2863420214068));
#54350=CARTESIAN_POINT('Ctrl Pts',(-3.7641369473265,40.9024321914955,-16.2907853454144));
#54351=CARTESIAN_POINT('Ctrl Pts',(-3.73619027274348,40.9608637952424,-16.29539225053));
#54352=CARTESIAN_POINT('Ctrl Pts',(-3.69171385851549,41.0538561906178,-16.3027240216006));
#54353=CARTESIAN_POINT('Ctrl Pts',(-3.64501276311427,41.1458483760823,-16.3104700046038));
#54354=CARTESIAN_POINT('Ctrl Pts',(-3.5959667510252,41.236790012973,-16.3185954496022));
#54355=CARTESIAN_POINT('Ctrl Pts',(-3.57775919507526,41.2705506567305,-16.3216118924918));
#54356=CARTESIAN_POINT('Ctrl Pts',(-3.5592284199418,41.3041665597948,-16.3246806590239));
#54357=CARTESIAN_POINT('Ctrl Pts',(-3.54036821085535,41.3376351406411,-16.3277999436471));
#54358=CARTESIAN_POINT('Ctrl Pts',(-3.51504025644013,41.3825811264534,-16.331988926833));
#54359=CARTESIAN_POINT('Ctrl Pts',(-3.4891166942094,41.4272607781668,-16.3362686376718));
#54360=CARTESIAN_POINT('Ctrl Pts',(-3.46257912027332,41.471666391437,-16.3406338568241));
#54361=CARTESIAN_POINT('Ctrl Pts',(-3.45564724394915,41.4832655760509,-16.3417740951656));
#54362=CARTESIAN_POINT('Ctrl Pts',(-3.44867346629616,41.4948460598394,-16.3429201660408));
#54363=CARTESIAN_POINT('Ctrl Pts',(-3.44165743709138,41.5064076958658,-16.3440719709585));
#54364=CARTESIAN_POINT('Ctrl Pts',(-3.43525505324746,41.5169581125679,-16.3451230351689));
#54365=CARTESIAN_POINT('Ctrl Pts',(-3.42881677312205,41.5274940047084,-16.3461789887384));
#54366=CARTESIAN_POINT('Ctrl Pts',(-3.42234310591756,41.5380139649604,-16.3472396330566));
#54367=CARTESIAN_POINT('Ctrl Pts',(-3.41519765756377,41.5496255956313,-16.3484103418617));
#54368=CARTESIAN_POINT('Ctrl Pts',(-3.40801236578587,41.5612124098009,-16.3495862278856));
#54369=CARTESIAN_POINT('Ctrl Pts',(-3.40079121408887,41.5727677646131,-16.3507664882365));
#54370=CARTESIAN_POINT('Ctrl Pts',(-3.39430786372305,41.5831424828011,-16.3518261587292));
#54371=CARTESIAN_POINT('Ctrl Pts',(-3.38779445712395,41.593493696068,-16.3528895361063));
#54372=CARTESIAN_POINT('Ctrl Pts',(-3.38125307744712,41.6038178373831,-16.3539561696315));
#54373=CARTESIAN_POINT('Ctrl Pts',(-3.37390786261472,41.6154106571957,-16.3551538760448));
#54374=CARTESIAN_POINT('Ctrl Pts',(-3.36652564355628,41.6269722107526,-16.356355978957));
#54375=CARTESIAN_POINT('Ctrl Pts',(-3.35910628076637,41.638502435275,-16.357562339157));
#54376=CARTESIAN_POINT('Ctrl Pts',(-3.33105272891493,41.6820996767975,-16.3621237400994));
#54377=CARTESIAN_POINT('Ctrl Pts',(-3.30247105915328,41.7252445352261,-16.3667454697368));
#54378=CARTESIAN_POINT('Ctrl Pts',(-3.27335493473435,41.7679327857555,-16.3714194616471));
#54379=CARTESIAN_POINT('Ctrl Pts',(-3.25227576109997,41.7988377589625,-16.3748032872424));
#54380=CARTESIAN_POINT('Ctrl Pts',(-3.23091649151266,41.829503356823,-16.3782145096199));
#54381=CARTESIAN_POINT('Ctrl Pts',(-3.20927471543407,41.8599279650246,-16.3816500603677));
#54382=CARTESIAN_POINT('Ctrl Pts',(-3.17113002588739,41.9135528260441,-16.387705386706));
#54383=CARTESIAN_POINT('Ctrl Pts',(-3.13210933033934,41.9664304210326,-16.3938367176048));
#54384=CARTESIAN_POINT('Ctrl Pts',(-3.09219386076608,42.0185471540337,-16.4000257673312));
#54385=CARTESIAN_POINT('Ctrl Pts',(-3.0296319451254,42.1002328435254,-16.4097262371245));
#54386=CARTESIAN_POINT('Ctrl Pts',(-2.96487183583847,42.1800495345858,-16.4195685651031));
#54387=CARTESIAN_POINT('Ctrl Pts',(-2.89784096682193,42.2579443794122,-16.4294813804493));
#54388=CARTESIAN_POINT('Ctrl Pts',(-2.87481981995416,42.2846966607014,-16.4328858473958));
#54389=CARTESIAN_POINT('Ctrl Pts',(-2.85153079730427,42.3112222445507,-16.4362986700301));
#54390=CARTESIAN_POINT('Ctrl Pts',(-2.82797091137712,42.3375190282482,-16.4397169174014));
#54391=CARTESIAN_POINT('Ctrl Pts',(-2.78293127718922,42.3877908131675,-16.4462516099563));
#54392=CARTESIAN_POINT('Ctrl Pts',(-2.7369026014617,42.4372271471467,-16.4528063924184));
#54393=CARTESIAN_POINT('Ctrl Pts',(-2.68985294718769,42.4858039179662,-16.4593577681913));
#54394=CARTESIAN_POINT('Ctrl Pts',(-2.61819198095264,42.5597908236559,-16.4693361181984));
#54395=CARTESIAN_POINT('Ctrl Pts',(-2.54416287898252,42.6317832884634,-16.4793067723326));
#54396=CARTESIAN_POINT('Ctrl Pts',(-2.46765134397022,42.7016952483703,-16.4891862846922));
#54397=CARTESIAN_POINT('Ctrl Pts',(-2.44852346021716,42.719173238347,-16.4916561627821));
#54398=CARTESIAN_POINT('Ctrl Pts',(-2.42924039812022,42.7365212099537,-16.4941203413884));
#54399=CARTESIAN_POINT('Ctrl Pts',(-2.40980030866471,42.7537378771226,-16.4965774832717));
#54400=CARTESIAN_POINT('Ctrl Pts',(-2.40468220997069,42.7582706032685,-16.4972243884566));
#54401=CARTESIAN_POINT('Ctrl Pts',(-2.3995528142902,42.7627945886819,-16.4978708622516));
#54402=CARTESIAN_POINT('Ctrl Pts',(-2.39441238378145,42.7673095437809,-16.498516841502));
#54403=CARTESIAN_POINT('Ctrl Pts',(-2.38002790183651,42.7799437560311,-16.5003244871552));
#54404=CARTESIAN_POINT('Ctrl Pts',(-2.36555579501941,42.7925074952912,-16.5021282682303));
#54405=CARTESIAN_POINT('Ctrl Pts',(-2.35102884419466,42.8049721064802,-16.5039235120036));
#54406=CARTESIAN_POINT('Ctrl Pts',(-2.34615879630707,42.8091507709586,-16.504525353591));
#54407=CARTESIAN_POINT('Ctrl Pts',(-2.34128179329844,42.8133189729222,-16.5051263396681));
#54408=CARTESIAN_POINT('Ctrl Pts',(-2.33639885646367,42.8174758102531,-16.5057263203709));
#54409=CARTESIAN_POINT('Ctrl Pts',(-2.31696011386605,42.8340239847697,-16.5081148154179));
#54410=CARTESIAN_POINT('Ctrl Pts',(-2.29741214406742,42.8504055250415,-16.5104892997636));
#54411=CARTESIAN_POINT('Ctrl Pts',(-2.27775717372585,42.8666186333273,-16.5128481934888));
#54412=CARTESIAN_POINT('Ctrl Pts',(-2.26236860104002,42.8793124502593,-16.5146950549654));
#54413=CARTESIAN_POINT('Ctrl Pts',(-2.24691444825131,42.8919030377098,-16.5165323596086));
#54414=CARTESIAN_POINT('Ctrl Pts',(-2.2313957874581,42.9043895385496,-16.5183593566189));
#54415=CARTESIAN_POINT('Ctrl Pts',(-2.2073019676343,42.9237757153255,-16.5211958988547));
#54416=CARTESIAN_POINT('Ctrl Pts',(-2.18305057305376,42.9429126314443,-16.5240078954214));
#54417=CARTESIAN_POINT('Ctrl Pts',(-2.15864142271283,42.961800356319,-16.5267930988146));
#54418=CARTESIAN_POINT('Ctrl Pts',(-2.10135766986817,43.0061263467124,-16.5333294550816));
#54419=CARTESIAN_POINT('Ctrl Pts',(-2.04320552379719,43.0490806846287,-16.5397182747111));
#54420=CARTESIAN_POINT('Ctrl Pts',(-1.98417891498175,43.0906578349874,-16.5459303792842));
#54421=CARTESIAN_POINT('Ctrl Pts',(-1.9606171900974,43.1072542378282,-16.5484100727959));
#54422=CARTESIAN_POINT('Ctrl Pts',(-1.93691615197933,43.123631187596,-16.550861606755));
#54423=CARTESIAN_POINT('Ctrl Pts',(-1.91307539225617,43.1397883575922,-16.5532831180631));
#54424=CARTESIAN_POINT('Ctrl Pts',(-1.85174084432199,43.1813555194244,-16.5595128818426));
#54425=CARTESIAN_POINT('Ctrl Pts',(-1.78948388159612,43.221472033667,-16.5655442738707));
#54426=CARTESIAN_POINT('Ctrl Pts',(-1.72628822892224,43.2601164045817,-16.5713446579823));
#54427=CARTESIAN_POINT('Ctrl Pts',(-1.63852840447744,43.3137818556649,-16.5793996533785));
#54428=CARTESIAN_POINT('Ctrl Pts',(-1.54895857244756,43.3646081409297,-16.5870091768287));
#54429=CARTESIAN_POINT('Ctrl Pts',(-1.45753509356855,43.4125380051629,-16.5940846193997));
#54430=CARTESIAN_POINT('Ctrl Pts',(-1.43588830470891,43.4238865959609,-16.5957599069002));
#54431=CARTESIAN_POINT('Ctrl Pts',(-1.41413751963647,43.4350727363855,-16.5974053637665));
#54432=CARTESIAN_POINT('Ctrl Pts',(-1.39228215387348,43.4460956894796,-16.5990197793473));
#54433=CARTESIAN_POINT('Ctrl Pts',(-1.32183313291274,43.4816272958594,-16.6042237186599));
#54434=CARTESIAN_POINT('Ctrl Pts',(-1.25029501345785,43.5154590902996,-16.6091048720554));
#54435=CARTESIAN_POINT('Ctrl Pts',(-1.17763414652208,43.5475427918415,-16.6136202138518));
#54436=CARTESIAN_POINT('Ctrl Pts',(-1.15739410693042,43.5564798637048,-16.6148779843765));
#54437=CARTESIAN_POINT('Ctrl Pts',(-1.13706740551599,43.5652810566249,-16.6161073852453));
#54438=CARTESIAN_POINT('Ctrl Pts',(-1.11665204632759,43.5739458510516,-16.6173075683168));
#54439=CARTESIAN_POINT('Ctrl Pts',(-1.11306064109996,43.5754701342011,-16.6175187007155));
#54440=CARTESIAN_POINT('Ctrl Pts',(-1.10946637251239,43.5769902275687,-16.6177289324325));
#54441=CARTESIAN_POINT('Ctrl Pts',(-1.10586955611941,43.5785059994041,-16.6179382417103));
#54442=CARTESIAN_POINT('Ctrl Pts',(-1.09384808843183,43.5835720912337,-16.6186378061155));
#54443=CARTESIAN_POINT('Ctrl Pts',(-1.0817936254975,43.5885917864702,-16.6193273211788));
#54444=CARTESIAN_POINT('Ctrl Pts',(-1.06972876207832,43.5935556457637,-16.6200053966719));
#54445=CARTESIAN_POINT('Ctrl Pts',(-1.06188552091578,43.5967825986254,-16.6204462064377));
#54446=CARTESIAN_POINT('Ctrl Pts',(-1.05403471295521,43.5999873202319,-16.6208823173579));
#54447=CARTESIAN_POINT('Ctrl Pts',(-1.04617933152838,43.6031685148794,-16.6213135432057));
#54448=CARTESIAN_POINT('Ctrl Pts',(-1.04195117477803,43.6048807919659,-16.6215456503919));
#54449=CARTESIAN_POINT('Ctrl Pts',(-1.03772102067868,43.6065865438,-16.6217763829208));
#54450=CARTESIAN_POINT('Ctrl Pts',(-1.03348881978403,43.6082857884376,-16.6220057425198));
#54451=CARTESIAN_POINT('Ctrl Pts',(-1.01416402109236,43.6160447680716,-16.623053029307));
#54452=CARTESIAN_POINT('Ctrl Pts',(-0.994800665078688,43.6236663683118,
-16.6240715200906));
#54453=CARTESIAN_POINT('Ctrl Pts',(-0.975398838645345,43.6311509959951,
-16.6250607039036));
#54454=CARTESIAN_POINT('Ctrl Pts',(-0.946227439814781,43.6424044241195,
-16.6265479801467));
#54455=CARTESIAN_POINT('Ctrl Pts',(-0.916969087203641,43.6533482686037,
-16.6279690016024));
#54456=CARTESIAN_POINT('Ctrl Pts',(-0.887623971798692,43.6639834687485,
-16.6293220547001));
#54457=CARTESIAN_POINT('Ctrl Pts',(-0.869449089231215,43.6705703746455,
-16.6301600674602));
#54458=CARTESIAN_POINT('Ctrl Pts',(-0.851240929339034,43.6770388362738,
-16.6309720567335));
#54459=CARTESIAN_POINT('Ctrl Pts',(-0.832999523055785,43.6833890388058,
-16.6317576612342));
#54460=CARTESIAN_POINT('Ctrl Pts',(-0.753158275762128,43.7111833920948,
-16.6351961923561));
#54461=CARTESIAN_POINT('Ctrl Pts',(-0.672680496364904,43.7367139705469,
-16.6381292382759));
#54462=CARTESIAN_POINT('Ctrl Pts',(-0.591564904416325,43.759978410422,-16.6405269912691));
#54463=CARTESIAN_POINT('Ctrl Pts',(-0.576024848681799,43.7644353919173,
-16.6409863507369));
#54464=CARTESIAN_POINT('Ctrl Pts',(-0.560461385298049,43.7688091891839,
-16.6414260739135));
#54465=CARTESIAN_POINT('Ctrl Pts',(-0.54487449675861,43.7730997914147,-16.6418459474937));
#54466=CARTESIAN_POINT('Ctrl Pts',(-0.460512928369039,43.7963219972201,
-16.6441184468226));
#54467=CARTESIAN_POINT('Ctrl Pts',(-0.375465187199559,43.8171072363759,
-16.6458095771723));
#54468=CARTESIAN_POINT('Ctrl Pts',(-0.289722449806869,43.8354260792837,
-16.6468857729884));
#54469=CARTESIAN_POINT('Ctrl Pts',(-0.277274221907169,43.8380856296819,
-16.6470420163181));
#54470=CARTESIAN_POINT('Ctrl Pts',(-0.264811340139473,43.8406931831398,
-16.6471853089574));
#54471=CARTESIAN_POINT('Ctrl Pts',(-0.252333773908635,43.8432486511893,
-16.6473155453024));
#54472=CARTESIAN_POINT('Ctrl Pts',(-0.213899223809915,43.8511202395231,
-16.6477167113019));
#54473=CARTESIAN_POINT('Ctrl Pts',(-0.175325354404486,43.8584976721331,
-16.6479940080683));
#54474=CARTESIAN_POINT('Ctrl Pts',(-0.136610688709363,43.8653757031155,
-16.6481443294018));
#54475=CARTESIAN_POINT('Ctrl Pts',(-0.0917379150289355,43.8733477809341,
-16.6483185614416));
#54476=CARTESIAN_POINT('Ctrl Pts',(-0.0466760171364662,43.8806488794434,
-16.6483222800481));
#54477=CARTESIAN_POINT('Ctrl Pts',(-0.00142252104673145,43.8872706258809,
-16.6481507404151));
#54478=CARTESIAN_POINT('Ctrl Pts',(0.00504226410894038,43.8882165896577,
-16.6481262347533));
#54479=CARTESIAN_POINT('Ctrl Pts',(0.0115023831731756,43.8891474722818,
-16.6480981942689));
#54480=CARTESIAN_POINT('Ctrl Pts',(0.017983572713365,43.8900669127708,-16.6480664654997));
#54481=CARTESIAN_POINT('Ctrl Pts',(0.0268684009855446,43.8913273404748,
-16.6480229696778));
#54482=CARTESIAN_POINT('Ctrl Pts',(0.0357560300500095,43.892560944674,-16.6479727334698));
#54483=CARTESIAN_POINT('Ctrl Pts',(0.0446464265659024,43.8937677392893,
-16.6479157416917));
#54484=CARTESIAN_POINT('Ctrl Pts',(0.0946198190147424,43.9005511961139,
-16.6475953878708));
#54485=CARTESIAN_POINT('Ctrl Pts',(0.144680824104186,43.9064867836914,-16.647061551913));
#54486=CARTESIAN_POINT('Ctrl Pts',(0.194824381188862,43.9115730116413,-16.6463116348634));
#54487=CARTESIAN_POINT('Ctrl Pts',(0.219976230483605,43.9141242474592,-16.6459354788483));
#54488=CARTESIAN_POINT('Ctrl Pts',(0.245148857175417,43.9164617506663,-16.6455049604648));
#54489=CARTESIAN_POINT('Ctrl Pts',(0.270341668442436,43.9185851214958,-16.6450197727132));
#54490=CARTESIAN_POINT('Ctrl Pts',(0.282958869797485,43.9196485596735,-16.644776778333));
#54491=CARTESIAN_POINT('Ctrl Pts',(0.29558113442138,43.920658285667,-16.6445200715934));
#54492=CARTESIAN_POINT('Ctrl Pts',(0.308208390846211,43.92161423551,-16.6442496152386));
#54493=CARTESIAN_POINT('Ctrl Pts',(0.315530705182528,43.9221685732857,-16.6440927825603));
#54494=CARTESIAN_POINT('Ctrl Pts',(0.322859901802196,43.9227051771392,-16.6439312040685));
#54495=CARTESIAN_POINT('Ctrl Pts',(0.330186921934994,43.9232234261787,-16.6437650852288));
#54496=CARTESIAN_POINT('Ctrl Pts',(0.335506964409879,43.9235997192492,-16.6436444687617));
#54497=CARTESIAN_POINT('Ctrl Pts',(0.340827324348622,43.9239664363589,-16.6435214329505));
#54498=CARTESIAN_POINT('Ctrl Pts',(0.346147593727981,43.9243235322772,-16.6433959637249));
#54499=CARTESIAN_POINT('Origin',(4.5,24.,-35.));
#54500=CARTESIAN_POINT('',(5.56574965699116,22.3076118445749,-37.));
#54501=CARTESIAN_POINT('',(6.5,24.,-37.));
#54502=CARTESIAN_POINT('Origin',(4.5,24.,-37.));
#54503=CARTESIAN_POINT('',(3.43425034300884,22.3076118445749,-37.));
#54504=CARTESIAN_POINT('Origin',(4.5,23.9999999999985,-38.6923881554236));
#54505=CARTESIAN_POINT('Origin',(4.5,24.,-37.));
#54506=CARTESIAN_POINT('',(6.5,24.,-35.));
#54507=CARTESIAN_POINT('',(6.5,24.,-35.));
#54508=CARTESIAN_POINT('Origin',(4.5,24.,-35.));
#54509=CARTESIAN_POINT('Origin',(-31.5,50.9282032302755,96.1658609549528));
#54510=CARTESIAN_POINT('',(-29.2705,50.9282032302755,-24.5));
#54511=CARTESIAN_POINT('Origin',(-31.5,50.9282032302755,-24.5));
#54512=CARTESIAN_POINT('',(-29.2705,50.9282032302755,-17.));
#54513=CARTESIAN_POINT('',(-29.2705,50.9282032302755,96.1658609549528));
#54514=CARTESIAN_POINT('Origin',(-31.5,50.9282032302755,-17.));
#54515=CARTESIAN_POINT('Origin',(3.49012810839377E-15,57.,-2.60208521396521E-14));
#54516=CARTESIAN_POINT('',(2.14313189850786E-15,-8.88178419700125E-15,17.5));
#54517=CARTESIAN_POINT('Origin',(-1.54074395550979E-30,-1.38777878078145E-14,
5.20417042793043E-15));
#54518=CARTESIAN_POINT('',(2.84458618865033E-15,11.4559962546824,17.5));
#54519=CARTESIAN_POINT('',(5.63326000690164E-15,57.,17.5));
#54520=CARTESIAN_POINT('Origin',(7.01454290142472E-16,11.4559962546824,
-1.07150924902746E-15));
#54521=CARTESIAN_POINT('Origin',(-49.5,46.2097438724404,-22.5588698729115));
#54522=CARTESIAN_POINT('',(-49.8535533905933,46.3993237581462,-22.2604415449401));
#54523=CARTESIAN_POINT('',(-50.,46.2097438724404,-22.5588698729115));
#54524=CARTESIAN_POINT('Origin',(-49.5,46.2097438724404,-22.5588698729115));
#54525=CARTESIAN_POINT('',(-49.5,45.787702483627,-22.2907634273934));
#54526=CARTESIAN_POINT('Origin',(-49.5,46.2097438724404,-22.5588698729115));
#54527=CARTESIAN_POINT('Origin',(-49.5,46.2097438724404,-22.5588698729115));
#54528=CARTESIAN_POINT('Origin',(-50.,41.3460650567048,-35.8098521656684));
#54529=CARTESIAN_POINT('',(-6.5,41.7681064455182,-36.0779586111866));
#54530=CARTESIAN_POINT('',(-6.5,41.0779586111866,-36.2318935544818));
#54531=CARTESIAN_POINT('Origin',(-6.5,41.3460650567048,-35.8098521656684));
#54532=CARTESIAN_POINT('',(-45.2928932188134,41.0779586111866,-36.2318935544818));
#54533=CARTESIAN_POINT('',(-50.,41.0779586111866,-36.2318935544818));
#54534=CARTESIAN_POINT('',(-45.2928932188134,41.7681064455182,-36.0779586111866));
#54535=CARTESIAN_POINT('Origin',(-45.2928932188134,41.3460650567048,-35.8098521656684));
#54536=CARTESIAN_POINT('',(-50.,41.7681064455182,-36.0779586111866));
#54537=CARTESIAN_POINT('Origin',(-47.3964466094067,42.4740175017242,-34.0342789768499));
#54538=CARTESIAN_POINT('',(-45.6464466094067,41.156485170999,-36.1082804936397));
#54539=CARTESIAN_POINT('Origin',(-45.2928932188135,41.3460650567048,-35.8098521656684));
#54540=CARTESIAN_POINT('',(-49.8535533905933,43.412390061038,-32.5571341160028));
#54541=CARTESIAN_POINT('',(-45.5,41.0779586111866,-36.2318935544818));
#54542=CARTESIAN_POINT('',(-49.5,44.0240113355571,-32.5268122335495));
#54543=CARTESIAN_POINT('Origin',(-49.5,43.6019699467437,-32.2587057880314));
#54544=CARTESIAN_POINT('',(-49.6464466094067,44.1025378953696,-32.4031991727075));
#54545=CARTESIAN_POINT('Origin',(-49.5,43.6019699467437,-32.2587057880314));
#54546=CARTESIAN_POINT('',(-50.,43.6019699467437,-32.2587057880314));
#54547=CARTESIAN_POINT('Origin',(-49.5,43.6019699467437,-32.2587057880314));
#54548=CARTESIAN_POINT('Origin',(-49.5,43.6019699467437,-32.2587057880314));
#54549=CARTESIAN_POINT('Origin',(-45.2221315177632,42.835413406597,-27.8705926603572));
#54550=CARTESIAN_POINT('',(-49.5,42.4133720177836,-27.602486214839));
#54551=CARTESIAN_POINT('',(-50.,43.1035198521152,-27.4485512715437));
#54552=CARTESIAN_POINT('Origin',(-49.5000000000041,42.8354134065986,-27.8705926603528));
#54553=CARTESIAN_POINT('',(-50.,42.4133720177836,-27.602486214839));
#54554=CARTESIAN_POINT('',(-45.2221315177632,43.1035198521152,-27.4485512715437));
#54555=CARTESIAN_POINT('Origin',(-6.5,41.3460650567048,-35.8098521656684));
#54556=CARTESIAN_POINT('',(-6.,41.3460650567048,-35.8098521656684));
#54557=CARTESIAN_POINT('Origin',(-6.5,41.3460650567048,-35.8098521656684));
#54558=CARTESIAN_POINT('Origin',(-6.5,41.3460650567048,-35.8098521656684));
#54559=CARTESIAN_POINT('Origin',(-27.5,24.,-29.5));
#54560=CARTESIAN_POINT('',(-17.5,27.3235,-29.5));
#54561=CARTESIAN_POINT('Origin',(-17.5,24.,-29.5));
#54562=CARTESIAN_POINT('',(-27.5,27.3235,-29.5));
#54563=CARTESIAN_POINT('',(-27.5,27.3235,-29.5));
#54564=CARTESIAN_POINT('Origin',(-27.5,24.,-29.5));
#54565=CARTESIAN_POINT('Origin',(-29.,21.,1.));
#54566=CARTESIAN_POINT('',(-16.9705627484772,21.5,1.));
#54567=CARTESIAN_POINT('',(-17.0000000870233,21.0000000000022,0.499999252982979));
#54568=CARTESIAN_POINT('Ctrl Pts',(-16.9705627484772,21.5,1.));
#54569=CARTESIAN_POINT('Ctrl Pts',(-16.9730813739591,21.5,0.97862875046525));
#54570=CARTESIAN_POINT('Ctrl Pts',(-16.9754128387929,21.49863561053,0.957471138975276));
#54571=CARTESIAN_POINT('Ctrl Pts',(-16.977567566868,21.4959539436567,0.936520192097311));
#54572=CARTESIAN_POINT('Ctrl Pts',(-16.9797222949432,21.4932722767835,0.915569245219347));
#54573=CARTESIAN_POINT('Ctrl Pts',(-16.9817002334104,21.4892732994039,0.894824944327382));
#54574=CARTESIAN_POINT('Ctrl Pts',(-16.9835103667152,21.4839393536879,0.874291199214557));
#54575=CARTESIAN_POINT('Ctrl Pts',(-16.9844154333676,21.4812723808299,0.864024326658143));
#54576=CARTESIAN_POINT('Ctrl Pts',(-16.9852785330442,21.4782708106201,0.853810226313161));
#54577=CARTESIAN_POINT('Ctrl Pts',(-16.9861007130495,21.4749261233953,0.843650463575198));
#54578=CARTESIAN_POINT('Ctrl Pts',(-16.9865118030522,21.4732537797829,0.838570582206216));
#54579=CARTESIAN_POINT('Ctrl Pts',(-16.9869133178517,21.4714922243147,0.833495564598339));
#54580=CARTESIAN_POINT('Ctrl Pts',(-16.987302317957,21.4696553181118,0.828466093560954));
#54581=CARTESIAN_POINT('Ctrl Pts',(-16.9876913180624,21.4678184119089,0.82343662252357));
#54582=CARTESIAN_POINT('Ctrl Pts',(-16.9880681393362,21.4659051003747,0.818448723733261));
#54583=CARTESIAN_POINT('Ctrl Pts',(-16.9884333019219,21.4639163929689,0.813501795185541));
#54584=CARTESIAN_POINT('Ctrl Pts',(-16.989893952265,21.4559615633459,0.793714080994655));
#54585=CARTESIAN_POINT('Ctrl Pts',(-16.9911680656929,21.4468050031027,0.774580106115942));
#54586=CARTESIAN_POINT('Ctrl Pts',(-16.9922828276023,21.4364710184893,0.756088025810979));
#54587=CARTESIAN_POINT('Ctrl Pts',(-16.9933975895117,21.4261370338759,0.737595945506016));
#54588=CARTESIAN_POINT('Ctrl Pts',(-16.9943528877412,21.4146260902305,0.719745496340949));
#54589=CARTESIAN_POINT('Ctrl Pts',(-16.9951723491632,21.4019047888025,0.702556657651023));
#54590=CARTESIAN_POINT('Ctrl Pts',(-16.9953772145187,21.3987244634455,0.698259447978542));
#54591=CARTESIAN_POINT('Ctrl Pts',(-16.9955735792695,21.3954682517381,0.69400371178678));
#54592=CARTESIAN_POINT('Ctrl Pts',(-16.9957617899228,21.3921349753008,0.689790133583646));
#54593=CARTESIAN_POINT('Ctrl Pts',(-16.9959500005762,21.3888016988636,0.685576555380513));
#54594=CARTESIAN_POINT('Ctrl Pts',(-16.9961295493961,21.3853997705542,0.681416137771084));
#54595=CARTESIAN_POINT('Ctrl Pts',(-16.9963002484149,21.381944233318,0.677325857685364));
#54596=CARTESIAN_POINT('Ctrl Pts',(-16.9966416464526,21.3750331588455,0.669145297513925));
#54597=CARTESIAN_POINT('Ctrl Pts',(-16.9969485933011,21.3678906232202,0.661223354235855));
#54598=CARTESIAN_POINT('Ctrl Pts',(-16.9972257305589,21.360521338635,0.65355467291949));
#54599=CARTESIAN_POINT('Ctrl Pts',(-16.9977800050746,21.3457827694648,0.638217310286761));
#54600=CARTESIAN_POINT('Ctrl Pts',(-16.9982150450431,21.3301402535137,0.623890202235327));
#54601=CARTESIAN_POINT('Ctrl Pts',(-16.9985616334457,21.3135980989733,0.61056934740525));
#54602=CARTESIAN_POINT('Ctrl Pts',(-16.9987349276469,21.3053270217032,0.603908919990211));
#54603=CARTESIAN_POINT('Ctrl Pts',(-16.9988860174545,21.2968304471392,0.597500710279847));
#54604=CARTESIAN_POINT('Ctrl Pts',(-16.9990182484227,21.2881047011117,0.591348949103243));
#54605=CARTESIAN_POINT('Ctrl Pts',(-16.9990843639068,21.2837418280979,0.588273068514941));
#54606=CARTESIAN_POINT('Ctrl Pts',(-16.9991457654173,21.2793216399187,0.585261334334855));
#54607=CARTESIAN_POINT('Ctrl Pts',(-16.9992028412883,21.2748433907653,0.58231457937545));
#54608=CARTESIAN_POINT('Ctrl Pts',(-16.9992599171592,21.2703651416119,0.579367824416043));
#54609=CARTESIAN_POINT('Ctrl Pts',(-16.9993127537119,21.2658204194787,0.576481010796243));
#54610=CARTESIAN_POINT('Ctrl Pts',(-16.9993614043243,21.2612406847754,0.573674650246304));
#54611=CARTESIAN_POINT('Ctrl Pts',(-16.9995560067739,21.2429217459622,0.562449208046549));
#54612=CARTESIAN_POINT('Ctrl Pts',(-16.9996844419683,21.2240702465873,0.552514693415452));
#54613=CARTESIAN_POINT('Ctrl Pts',(-16.9997740428036,21.204705397676,0.543824923165798));
#54614=CARTESIAN_POINT('Ctrl Pts',(-16.9998636436388,21.1853405487646,0.535135152916144));
#54615=CARTESIAN_POINT('Ctrl Pts',(-16.9999142934875,21.1654623146662,0.527690138120709));
#54616=CARTESIAN_POINT('Ctrl Pts',(-16.9999455849911,21.1450641098525,0.52150610826049));
#54617=CARTESIAN_POINT('Ctrl Pts',(-16.999961230743,21.1348650074456,0.518414093330381));
#54618=CARTESIAN_POINT('Ctrl Pts',(-16.9999719363109,21.1245355567772,0.515638162273462));
#54619=CARTESIAN_POINT('Ctrl Pts',(-16.9999795432265,21.114072442886,0.513186403367121));
#54620=CARTESIAN_POINT('Ctrl Pts',(-16.9999833466843,21.1088408859405,0.511960523913951));
#54621=CARTESIAN_POINT('Ctrl Pts',(-16.9999863636806,21.1035820426627,0.510817546177565));
#54622=CARTESIAN_POINT('Ctrl Pts',(-16.9999887849483,21.0983273296019,0.509763591729921));
#54623=CARTESIAN_POINT('Ctrl Pts',(-16.999991206216,21.093072616541,0.508709637282276));
#54624=CARTESIAN_POINT('Ctrl Pts',(-16.9999930072076,21.0878132493178,0.507742627816665));
#54625=CARTESIAN_POINT('Ctrl Pts',(-16.9999944360759,21.08254922085,0.506861453386952));
#54626=CARTESIAN_POINT('Ctrl Pts',(-17.0000001515491,21.0614931069787,0.5033367556681));
#54627=CARTESIAN_POINT('Ctrl Pts',(-16.9999999151385,21.0403633334935,0.501180364269346));
#54628=CARTESIAN_POINT('Ctrl Pts',(-16.999999983465,21.0191612004193,0.500367286323289));
#54629=CARTESIAN_POINT('Ctrl Pts',(-17.000000004027,21.0127807046791,0.500122601491195));
#54630=CARTESIAN_POINT('Ctrl Pts',(-17.0000000526406,21.0063936586163,0.499999543843031));
#54631=CARTESIAN_POINT('Ctrl Pts',(-17.0000000862986,21.0000000000001,0.499999252164641));
#54632=CARTESIAN_POINT('',(-16.9996439954592,20.7720018726588,0.555009152983013));
#54633=CARTESIAN_POINT('Ctrl Pts',(-17.0000000877479,21.,0.499999253801316));
#54634=CARTESIAN_POINT('Ctrl Pts',(-17.0000001651403,20.9851477858762,0.49999856840262));
#54635=CARTESIAN_POINT('Ctrl Pts',(-17.0000001594763,20.9702598890947,0.500660382574086));
#54636=CARTESIAN_POINT('Ctrl Pts',(-16.9999993047839,20.9499982803608,0.502477594919463));
#54637=CARTESIAN_POINT('Ctrl Pts',(-16.9999989597664,20.9446478701007,0.503044245481599));
#54638=CARTESIAN_POINT('Ctrl Pts',(-16.9999978251355,20.9339792642195,0.504348769112458));
#54639=CARTESIAN_POINT('Ctrl Pts',(-16.9999954462377,20.9180500526981,0.506558461151423));
#54640=CARTESIAN_POINT('Ctrl Pts',(-16.9999899689093,20.9023385597306,0.509515289748651));
#54641=CARTESIAN_POINT('Ctrl Pts',(-16.9999708157118,20.8712004350647,0.516406468513256));
#54642=CARTESIAN_POINT('Ctrl Pts',(-16.9999475802786,20.8508203671619,0.522300064017838));
#54643=CARTESIAN_POINT('Ctrl Pts',(-16.9998727181797,20.8208178771162,0.533088108138553));
#54644=CARTESIAN_POINT('Ctrl Pts',(-16.9998251170355,20.805958960354,0.538970501410492));
#54645=CARTESIAN_POINT('Ctrl Pts',(-16.9997329714124,20.7864371314905,0.54780774482637));
#54646=CARTESIAN_POINT('Ctrl Pts',(-16.9996756422965,20.7767738128281,0.552564173654396));
#54647=CARTESIAN_POINT('Ctrl Pts',(-16.9996439954592,20.7720018726588,0.555009152983013));
#54648=CARTESIAN_POINT('Ctrl Pts',(-16.9996439954592,20.7720018726588,0.555009152983015));
#54649=CARTESIAN_POINT('Ctrl Pts',(-16.9995764019144,20.7618096266294,0.560231312098567));
#54650=CARTESIAN_POINT('Ctrl Pts',(-16.999744036059,20.7518188801895,0.565791848329536));
#54651=CARTESIAN_POINT('Ctrl Pts',(-17.0001141476166,20.7420298241553,0.571687744309563));
#54652=CARTESIAN_POINT('Ctrl Pts',(-17.0004874229058,20.7321570907942,0.577634038694984));
#54653=CARTESIAN_POINT('Ctrl Pts',(-17.0010693506212,20.7224661626916,0.583939604181921));
#54654=CARTESIAN_POINT('Ctrl Pts',(-17.0018149866956,20.7130824637923,0.590514557747761));
#54655=CARTESIAN_POINT('Ctrl Pts',(-17.0033122137324,20.694240124774,0.603716974560899));
#54656=CARTESIAN_POINT('Ctrl Pts',(-17.0054671735487,20.6765333488168,0.618051718651848));
#54657=CARTESIAN_POINT('Ctrl Pts',(-17.0079791771995,20.6598958538764,0.633490559753894));
#54658=CARTESIAN_POINT('Ctrl Pts',(-17.0104973975899,20.6432171842449,0.648967609102669));
#54659=CARTESIAN_POINT('Ctrl Pts',(-17.0133771603985,20.6276123165059,0.665555354806171));
#54660=CARTESIAN_POINT('Ctrl Pts',(-17.0163366248286,20.6130881199025,0.683299515252358));
#54661=CARTESIAN_POINT('Ctrl Pts',(-17.0170769637466,20.6094547503342,0.687738390209771));
#54662=CARTESIAN_POINT('Ctrl Pts',(-17.0178235541468,20.6058834717914,0.692257774069122));
#54663=CARTESIAN_POINT('Ctrl Pts',(-17.018567812662,20.6023942721301,0.696833898390537));
#54664=CARTESIAN_POINT('Ctrl Pts',(-17.019312023868,20.5989052942621,0.701409731827615));
#54665=CARTESIAN_POINT('Ctrl Pts',(-17.020052498857,20.595504625966,0.706033510702339));
#54666=CARTESIAN_POINT('Ctrl Pts',(-17.0207848923251,20.5921907419765,0.710704979181601));
#54667=CARTESIAN_POINT('Ctrl Pts',(-17.02224911219,20.5855655398429,0.720044299155679));
#54668=CARTESIAN_POINT('Ctrl Pts',(-17.0236809280861,20.5792868927269,0.729573973065133));
#54669=CARTESIAN_POINT('Ctrl Pts',(-17.0250473303692,20.5733474924981,0.739293962781099));
#54670=CARTESIAN_POINT('Ctrl Pts',(-17.0277720965537,20.5615036328232,0.75867676067364));
#54671=CARTESIAN_POINT('Ctrl Pts',(-17.0302364268958,20.5510032860685,0.778813429678428));
#54672=CARTESIAN_POINT('Ctrl Pts',(-17.0321922520697,20.5418565839912,0.799738644735398));
#54673=CARTESIAN_POINT('Ctrl Pts',(-17.0331698308387,20.5372847941006,0.810197680773625));
#54674=CARTESIAN_POINT('Ctrl Pts',(-17.0340205434215,20.5330525151684,0.820854418209816));
#54675=CARTESIAN_POINT('Ctrl Pts',(-17.0347134066204,20.52916974434,0.831717884603113));
#54676=CARTESIAN_POINT('Ctrl Pts',(-17.0350598382199,20.5272283589258,0.837149617799762));
#54677=CARTESIAN_POINT('Ctrl Pts',(-17.0353668002234,20.5253734731873,0.842637732950806));
#54678=CARTESIAN_POINT('Ctrl Pts',(-17.0356284233313,20.5236226585739,0.84812956651519));
#54679=CARTESIAN_POINT('Ctrl Pts',(-17.0358900464393,20.5218718439606,0.853621400079574));
#54680=CARTESIAN_POINT('Ctrl Pts',(-17.0361071634375,20.5202207447736,0.859128525898787));
#54681=CARTESIAN_POINT('Ctrl Pts',(-17.0362776979317,20.5186679181996,0.864650722093725));
#54682=CARTESIAN_POINT('Ctrl Pts',(-17.0369593616,20.512460930786,0.886724147967845));
#54683=CARTESIAN_POINT('Ctrl Pts',(-17.0368937799335,20.5078176119001,0.909036478152388));
#54684=CARTESIAN_POINT('Ctrl Pts',(-17.0359746831307,20.5047035481734,0.931579061625702));
#54685=CARTESIAN_POINT('Ctrl Pts',(-17.0350543072948,20.5015851508547,0.954153015799173));
#54686=CARTESIAN_POINT('Ctrl Pts',(-17.0332780282032,20.5,0.976957807069396));
#54687=CARTESIAN_POINT('Ctrl Pts',(-17.0305720504421,20.5,1.));
#54688=CARTESIAN_POINT('',(-28.5,20.5,1.));
#54689=CARTESIAN_POINT('',(-29.,20.5,1.));
#54690=CARTESIAN_POINT('',(-28.5,21.5,1.));
#54691=CARTESIAN_POINT('Origin',(-28.5,21.,1.));
#54692=CARTESIAN_POINT('',(-29.,21.5,1.));
#54693=CARTESIAN_POINT('Origin',(-28.5,21.,0.));
#54694=CARTESIAN_POINT('Origin',(-28.5,21.,1.));
#54695=CARTESIAN_POINT('',(-28.5,20.5,4.01452801010865));
#54696=CARTESIAN_POINT('',(-28.5,20.5,1.));
#54697=CARTESIAN_POINT('',(-28.9999999990691,21.0000000000002,3.86712647556469));
#54698=CARTESIAN_POINT('Ctrl Pts',(-28.5,20.5,4.01452801010866));
#54699=CARTESIAN_POINT('Ctrl Pts',(-28.5164513514331,20.5,4.01507018860936));
#54700=CARTESIAN_POINT('Ctrl Pts',(-28.5328300075924,20.5008099557645,4.0150659425191));
#54701=CARTESIAN_POINT('Ctrl Pts',(-28.5491369527492,20.5024202979677,4.01452953611992));
#54702=CARTESIAN_POINT('Ctrl Pts',(-28.5495960158313,20.5024656313302,4.01451443553716));
#54703=CARTESIAN_POINT('Ctrl Pts',(-28.5500550220854,20.502511600136,4.01449891327935));
#54704=CARTESIAN_POINT('Ctrl Pts',(-28.550513971537,20.5025582045811,4.01448296968854));
#54705=CARTESIAN_POINT('Ctrl Pts',(-28.5582710692767,20.5033459062212,4.01421349340558));
#54706=CARTESIAN_POINT('Ctrl Pts',(-28.566010072344,20.5043149278755,4.01382377207131));
#54707=CARTESIAN_POINT('Ctrl Pts',(-28.5737362162412,20.5054669167645,4.01331514715339));
#54708=CARTESIAN_POINT('Ctrl Pts',(-28.5743575582699,20.5055595605364,4.01327424317302));
#54709=CARTESIAN_POINT('Ctrl Pts',(-28.5749787684162,20.5056533859706,4.01323257019164));
#54710=CARTESIAN_POINT('Ctrl Pts',(-28.5755997697761,20.5057483782164,4.0131901369871));
#54711=CARTESIAN_POINT('Ctrl Pts',(-28.5790836390542,20.5062812926157,4.01295208318048));
#54712=CARTESIAN_POINT('Ctrl Pts',(-28.5825594001091,20.5068506858238,4.01269019751249));
#54713=CARTESIAN_POINT('Ctrl Pts',(-28.5860143380244,20.5074540288925,4.01240599961348));
#54714=CARTESIAN_POINT('Ctrl Pts',(-28.5900946138146,20.5081665760285,4.01207036237905));
#54715=CARTESIAN_POINT('Ctrl Pts',(-28.5941521350908,20.5089273704629,4.01170321587125));
#54716=CARTESIAN_POINT('Ctrl Pts',(-28.598189247445,20.5097359163816,4.01130545373038));
#54717=CARTESIAN_POINT('Ctrl Pts',(-28.5989198489116,20.5098822399867,4.01123347019909));
#54718=CARTESIAN_POINT('Ctrl Pts',(-28.5996497830969,20.5100301241402,4.01116048399731));
#54719=CARTESIAN_POINT('Ctrl Pts',(-28.6003790631507,20.5101795680466,4.01108649976395));
#54720=CARTESIAN_POINT('Ctrl Pts',(-28.6158373800123,20.5133472828995,4.00951827954991));
#54721=CARTESIAN_POINT('Ctrl Pts',(-28.6309836846376,20.51721179935,4.00750372591642));
#54722=CARTESIAN_POINT('Ctrl Pts',(-28.6458381311819,20.5217414512072,4.00509762013458));
#54723=CARTESIAN_POINT('Ctrl Pts',(-28.6466878656163,20.5220005656176,4.00495998115022));
#54724=CARTESIAN_POINT('Ctrl Pts',(-28.6475366445442,20.5222618577133,4.00482105955225));
#54725=CARTESIAN_POINT('Ctrl Pts',(-28.6483844703545,20.522525325589,4.00468086503783));
#54726=CARTESIAN_POINT('Ctrl Pts',(-28.6631564601653,20.5271158260522,4.00223820297968));
#54727=CARTESIAN_POINT('Ctrl Pts',(-28.6776392202979,20.5323666655798,3.99940952546827));
#54728=CARTESIAN_POINT('Ctrl Pts',(-28.6918445815767,20.5382688482248,3.99624486790792));
#54729=CARTESIAN_POINT('Ctrl Pts',(-28.6927070946931,20.5386272136227,3.99605271801456));
#54730=CARTESIAN_POINT('Ctrl Pts',(-28.6935685850001,20.5389879805298,3.99585932819182));
#54731=CARTESIAN_POINT('Ctrl Pts',(-28.69442905358,20.539351151545,3.99566470942585));
#54732=CARTESIAN_POINT('Ctrl Pts',(-28.7019451320231,20.5425234019941,3.99396474042557));
#54733=CARTESIAN_POINT('Ctrl Pts',(-28.7093832773834,20.5458790798609,3.99217104269849));
#54734=CARTESIAN_POINT('Ctrl Pts',(-28.7167440887879,20.5494199410241,3.99029080026248));
#54735=CARTESIAN_POINT('Ctrl Pts',(-28.7232979155013,20.5525726084686,3.98861669364193));
#54736=CARTESIAN_POINT('Ctrl Pts',(-28.7297897873453,20.5558717313291,3.98687415899974));
#54737=CARTESIAN_POINT('Ctrl Pts',(-28.736222233402,20.5593197798329,3.98506764460692));
#54738=CARTESIAN_POINT('Ctrl Pts',(-28.7370142722704,20.5597443443626,3.98484520517987));
#54739=CARTESIAN_POINT('Ctrl Pts',(-28.7378049045635,20.560170909351,3.98462193461541));
#54740=CARTESIAN_POINT('Ctrl Pts',(-28.738594101696,20.560599450483,3.98439785654188));
#54741=CARTESIAN_POINT('Ctrl Pts',(-28.7450528664492,20.564106617761,3.98256400856681));
#54742=CARTESIAN_POINT('Ctrl Pts',(-28.7514055277704,20.5677406151965,3.98067895641415));
#54743=CARTESIAN_POINT('Ctrl Pts',(-28.7576397468618,20.5714889023174,3.97875498379703));
#54744=CARTESIAN_POINT('Ctrl Pts',(-28.7646594833789,20.5757094771148,3.97658858883395));
#54745=CARTESIAN_POINT('Ctrl Pts',(-28.7715387445494,20.5800801099293,3.97437012159623));
#54746=CARTESIAN_POINT('Ctrl Pts',(-28.7782883626914,20.5846018931307,3.9721074341771));
#54747=CARTESIAN_POINT('Ctrl Pts',(-28.7789062759519,20.5850158528159,3.97190028993112));
#54748=CARTESIAN_POINT('Ctrl Pts',(-28.7795231038942,20.5854310777311,3.97169277505919));
#54749=CARTESIAN_POINT('Ctrl Pts',(-28.7801388532259,20.5858475706905,3.97148489500656));
#54750=CARTESIAN_POINT('Ctrl Pts',(-28.7930138998851,20.5945562545815,3.96713821488955));
#54751=CARTESIAN_POINT('Ctrl Pts',(-28.8054045352405,20.6038101537282,3.96263694559618));
#54752=CARTESIAN_POINT('Ctrl Pts',(-28.8173345884296,20.6136080241694,3.95804337703345));
#54753=CARTESIAN_POINT('Ctrl Pts',(-28.8177423111309,20.6139428771781,3.95788638677082));
#54754=CARTESIAN_POINT('Ctrl Pts',(-28.8181494955581,20.6142783658853,3.95772928820928));
#54755=CARTESIAN_POINT('Ctrl Pts',(-28.8185561420664,20.6146144909891,3.95757208373558));
#54756=CARTESIAN_POINT('Ctrl Pts',(-28.8306505221365,20.6246114408557,3.95289654708411));
#54757=CARTESIAN_POINT('Ctrl Pts',(-28.8422694642204,20.6351711425685,3.9481277290909));
#54758=CARTESIAN_POINT('Ctrl Pts',(-28.8534199982048,20.6463132673266,3.94332838466393));
#54759=CARTESIAN_POINT('Ctrl Pts',(-28.8536143750091,20.6465074975408,3.94324472219236));
#54760=CARTESIAN_POINT('Ctrl Pts',(-28.8538086101574,20.6467019063127,3.94316104994417));
#54761=CARTESIAN_POINT('Ctrl Pts',(-28.8540027035162,20.6468964937161,3.94307736830263));
#54762=CARTESIAN_POINT('Ctrl Pts',(-28.8595679483428,20.6524759042999,3.9406779620294));
#54763=CARTESIAN_POINT('Ctrl Pts',(-28.8650165644509,20.6582020618217,3.93827087234596));
#54764=CARTESIAN_POINT('Ctrl Pts',(-28.8703459030302,20.6640775206855,3.93586485412722));
#54765=CARTESIAN_POINT('Ctrl Pts',(-28.8704406479323,20.664181974506,3.93582207997102));
#54766=CARTESIAN_POINT('Ctrl Pts',(-28.8705353426575,20.6642864617524,3.93577931180518));
#54767=CARTESIAN_POINT('Ctrl Pts',(-28.8706299872311,20.6643909824247,3.93573654967076));
#54768=CARTESIAN_POINT('Ctrl Pts',(-28.8760419628682,20.6703676941454,3.93329132094817));
#54769=CARTESIAN_POINT('Ctrl Pts',(-28.8812917390082,20.6764556221647,3.93086501555022));
#54770=CARTESIAN_POINT('Ctrl Pts',(-28.8863833106843,20.6826548610351,3.92846553582844));
#54771=CARTESIAN_POINT('Ctrl Pts',(-28.8863892980072,20.6826621508951,3.92846271421248));
#54772=CARTESIAN_POINT('Ctrl Pts',(-28.8863952851119,20.682669440909,3.92845989263359));
#54773=CARTESIAN_POINT('Ctrl Pts',(-28.8864012719985,20.6826767310768,3.92845707109178));
#54774=CARTESIAN_POINT('Ctrl Pts',(-28.8965956469561,20.695090312607,3.9236525946728));
#54775=CARTESIAN_POINT('Ctrl Pts',(-28.906157067648,20.7079490685553,3.91895575780338));
#54776=CARTESIAN_POINT('Ctrl Pts',(-28.9150984275965,20.7212648273691,3.91442809948265));
#54777=CARTESIAN_POINT('Ctrl Pts',(-28.9152182750854,20.7214433080774,3.91436741201639));
#54778=CARTESIAN_POINT('Ctrl Pts',(-28.9153380111198,20.7216218709325,3.91430675503477));
#54779=CARTESIAN_POINT('Ctrl Pts',(-28.9154576357267,20.7218005159667,3.91424612868925));
#54780=CARTESIAN_POINT('Ctrl Pts',(-28.9242627426992,20.7349498894741,3.90978365669779));
#54781=CARTESIAN_POINT('Ctrl Pts',(-28.9324644748558,20.7485442462784,3.90548665876825));
#54782=CARTESIAN_POINT('Ctrl Pts',(-28.9400523922733,20.7626102463437,3.90141604958038));
#54783=CARTESIAN_POINT('Ctrl Pts',(-28.9402293321847,20.7629382463295,3.90132112851187));
#54784=CARTESIAN_POINT('Ctrl Pts',(-28.9404059381619,20.7632665029513,3.90122633069731));
#54785=CARTESIAN_POINT('Ctrl Pts',(-28.9405822100495,20.7635950165753,3.90113165692879));
#54786=CARTESIAN_POINT('Ctrl Pts',(-28.9442369224986,20.7704062151575,3.89916874948485));
#54787=CARTESIAN_POINT('Ctrl Pts',(-28.9477477566326,20.7773280603452,3.89725914981838));
#54788=CARTESIAN_POINT('Ctrl Pts',(-28.9511114770745,20.7843650393795,3.89541021586002));
#54789=CARTESIAN_POINT('Ctrl Pts',(-28.9512925263593,20.7847437985669,3.89531069862113));
#54790=CARTESIAN_POINT('Ctrl Pts',(-28.9514731291436,20.7851228489911,3.89521136826826));
#54791=CARTESIAN_POINT('Ctrl Pts',(-28.9516532891227,20.7855021994876,3.89511222369121));
#54792=CARTESIAN_POINT('Ctrl Pts',(-28.9532274481634,20.7888167980831,3.89424594177283));
#54793=CARTESIAN_POINT('Ctrl Pts',(-28.954769491257,20.7921584950771,3.89339288708423));
#54794=CARTESIAN_POINT('Ctrl Pts',(-28.9562782863987,20.7955254042893,3.89255427234121));
#54795=CARTESIAN_POINT('Ctrl Pts',(-28.9579597607261,20.7992776508642,3.89161967948501));
#54796=CARTESIAN_POINT('Ctrl Pts',(-28.9596006031374,20.8030630949436,3.89070263223272));
#54797=CARTESIAN_POINT('Ctrl Pts',(-28.9611903084036,20.8068588900011,3.88980980999067));
#54798=CARTESIAN_POINT('Ctrl Pts',(-28.9613600382809,20.8072641599861,3.88971448501893));
#54799=CARTESIAN_POINT('Ctrl Pts',(-28.9615292133495,20.8076696119071,3.88961942017834));
#54800=CARTESIAN_POINT('Ctrl Pts',(-28.9616978272843,20.8080752327577,3.88952461997149));
#54801=CARTESIAN_POINT('Ctrl Pts',(-28.9678462263432,20.8228659370924,3.88606779119053));
#54802=CARTESIAN_POINT('Ctrl Pts',(-28.9732630364474,20.83789669793,3.88295611032183));
#54803=CARTESIAN_POINT('Ctrl Pts',(-28.9779549539186,20.8531699429438,3.88022807675177));
#54804=CARTESIAN_POINT('Ctrl Pts',(-28.9780746227798,20.8535594919608,3.88015849737982));
#54805=CARTESIAN_POINT('Ctrl Pts',(-28.9781938201495,20.8539491990382,3.88008916763081));
#54806=CARTESIAN_POINT('Ctrl Pts',(-28.9783125461397,20.8543390642437,3.88002008814799));
#54807=CARTESIAN_POINT('Ctrl Pts',(-28.9829764275231,20.8696540350547,3.87730645726259));
#54808=CARTESIAN_POINT('Ctrl Pts',(-28.986912984661,20.88521298573,3.87497871048076));
#54809=CARTESIAN_POINT('Ctrl Pts',(-28.9901062452497,20.9010259115082,3.87307658812189));
#54810=CARTESIAN_POINT('Ctrl Pts',(-28.9901641270832,20.901312540523,3.87304210978022));
#54811=CARTESIAN_POINT('Ctrl Pts',(-28.9902217646508,20.9015992530081,3.87300777139739));
#54812=CARTESIAN_POINT('Ctrl Pts',(-28.9902791578525,20.9018860490275,3.87297357321668));
#54813=CARTESIAN_POINT('Ctrl Pts',(-28.9934686710319,20.9178241681235,3.87107307725357));
#54814=CARTESIAN_POINT('Ctrl Pts',(-28.9959038918218,20.9340201547597,3.86960522446342));
#54815=CARTESIAN_POINT('Ctrl Pts',(-28.9975428631309,20.9504914199225,3.86861479762559));
#54816=CARTESIAN_POINT('Ctrl Pts',(-28.9975508466297,20.9505716521533,3.86860997321448));
#54817=CARTESIAN_POINT('Ctrl Pts',(-28.9975588112477,20.9506518910969,3.8686051601259));
#54818=CARTESIAN_POINT('Ctrl Pts',(-28.9975667569751,20.9507321367091,3.86860035836809));
#54819=CARTESIAN_POINT('Ctrl Pts',(-28.9979739536847,20.9548445039341,3.86835428146862));
#54820=CARTESIAN_POINT('Ctrl Pts',(-28.9983312836708,20.9589758111358,3.86813805483529));
#54821=CARTESIAN_POINT('Ctrl Pts',(-28.9986360973411,20.9630941410715,3.86795347229001));
#54822=CARTESIAN_POINT('Ctrl Pts',(-28.9986369825427,20.9631061010088,3.86795293624854));
#54823=CARTESIAN_POINT('Ctrl Pts',(-28.9986378673028,20.9631180608498,3.86795240047308));
#54824=CARTESIAN_POINT('Ctrl Pts',(-28.9986387516214,20.9631300205938,3.86795186496367));
#54825=CARTESIAN_POINT('Ctrl Pts',(-28.9989442640887,20.9672618470215,3.86776685833533));
#54826=CARTESIAN_POINT('Ctrl Pts',(-28.9991977435996,20.9713882018456,3.86761320323202));
#54827=CARTESIAN_POINT('Ctrl Pts',(-28.9993998330421,20.9755090474354,3.86749064815707));
#54828=CARTESIAN_POINT('Ctrl Pts',(-28.9994025151862,20.975563739564,3.86748902159821));
#54829=CARTESIAN_POINT('Ctrl Pts',(-28.9994051882825,20.9756184307224,3.86748740051734));
#54830=CARTESIAN_POINT('Ctrl Pts',(-28.9994078523321,20.9756731209105,3.86748578491389));
#54831=CARTESIAN_POINT('Ctrl Pts',(-28.9998038844389,20.9838032512471,3.86724561264447));
#54832=CARTESIAN_POINT('Ctrl Pts',(-29.0000000019467,20.9919120710539,3.86712648199996));
#54833=CARTESIAN_POINT('Ctrl Pts',(-29.0000000000226,21.0000000000002,3.86712647556469));
#54834=CARTESIAN_POINT('',(-28.5,21.5,4.01452801010865));
#54835=CARTESIAN_POINT('Ctrl Pts',(-29.0000000000226,21.0000000000002,3.86712647556469));
#54836=CARTESIAN_POINT('Ctrl Pts',(-29.0000000000077,21.0000628081229,3.86712647551472));
#54837=CARTESIAN_POINT('Ctrl Pts',(-28.9999999881654,21.0001256149852,3.86712648264873));
#54838=CARTESIAN_POINT('Ctrl Pts',(-28.9999999644977,21.0001884205867,3.86712649696792));
#54839=CARTESIAN_POINT('Ctrl Pts',(-28.9999998965082,21.0003688399577,3.86712653810216));
#54840=CARTESIAN_POINT('Ctrl Pts',(-28.9999997311066,21.0005492489388,3.86712663852461));
#54841=CARTESIAN_POINT('Ctrl Pts',(-28.9999994683105,21.0007296475219,3.86712679826507));
#54842=CARTESIAN_POINT('Ctrl Pts',(-28.9999757916729,21.0169826794255,3.86714119010008));
#54843=CARTESIAN_POINT('Ctrl Pts',(-28.9991615791828,21.0331513380247,3.86763657203004));
#54844=CARTESIAN_POINT('Ctrl Pts',(-28.9975697782028,21.0492373417148,3.86859853229563));
#54845=CARTESIAN_POINT('Ctrl Pts',(-28.9975299458722,21.0496398688054,3.86862260384717));
#54846=CARTESIAN_POINT('Ctrl Pts',(-28.9974896266431,21.0500423441396,3.86864696760125));
#54847=CARTESIAN_POINT('Ctrl Pts',(-28.9974488203613,21.0504447677163,3.86867162334182));
#54848=CARTESIAN_POINT('Ctrl Pts',(-28.9958374348699,21.0663359365465,3.86964524556126));
#54849=CARTESIAN_POINT('Ctrl Pts',(-28.9934664417955,21.0821470065985,3.87107424571494));
#54850=CARTESIAN_POINT('Ctrl Pts',(-28.9903267115591,21.0978760232723,3.87294518199751));
#54851=CARTESIAN_POINT('Ctrl Pts',(-28.9902095243118,21.0984630928699,3.87301501279706));
#54852=CARTESIAN_POINT('Ctrl Pts',(-28.9900912606925,21.0990500622799,3.8730854613775));
#54853=CARTESIAN_POINT('Ctrl Pts',(-28.9899719201338,21.099636928186,3.873156526561));
#54854=CARTESIAN_POINT('Ctrl Pts',(-28.9891427293275,21.1037145344837,3.87365029496153));
#54855=CARTESIAN_POINT('Ctrl Pts',(-28.9882616492729,21.1077866910186,3.8741737758945));
#54856=CARTESIAN_POINT('Ctrl Pts',(-28.9873282487272,21.1118533764022,3.87472671536206));
#54857=CARTESIAN_POINT('Ctrl Pts',(-28.9865480123162,21.115252748754,3.87518892154743));
#54858=CARTESIAN_POINT('Ctrl Pts',(-28.9857308794749,21.1186496307155,3.8756719108919));
#54859=CARTESIAN_POINT('Ctrl Pts',(-28.984877571924,21.1220399125086,3.87617496320682));
#54860=CARTESIAN_POINT('Ctrl Pts',(-28.9847100635754,21.1227054410203,3.87627371477936));
#54861=CARTESIAN_POINT('Ctrl Pts',(-28.9845412792207,21.1233702543533,3.87637316979248));
#54862=CARTESIAN_POINT('Ctrl Pts',(-28.9843712295124,21.1240343283173,3.87647331953722));
#54863=CARTESIAN_POINT('Ctrl Pts',(-28.9824842924156,21.1314031489441,3.87758461970075));
#54864=CARTESIAN_POINT('Ctrl Pts',(-28.9804413090385,21.1386820012024,3.8787816368253));
#54865=CARTESIAN_POINT('Ctrl Pts',(-28.9782473821909,21.1458747456812,3.88005797372067));
#54866=CARTESIAN_POINT('Ctrl Pts',(-28.9780315058454,21.1465824918825,3.88018356174789));
#54867=CARTESIAN_POINT('Ctrl Pts',(-28.977814170689,21.1472894055721,3.88030991766809));
#54868=CARTESIAN_POINT('Ctrl Pts',(-28.9775953797715,21.1479954896081,3.88043703577741));
#54869=CARTESIAN_POINT('Ctrl Pts',(-28.9729390160451,21.1630225489193,3.88314239558005));
#54870=CARTESIAN_POINT('Ctrl Pts',(-28.9676236436874,21.1776738449045,3.88619297247208));
#54871=CARTESIAN_POINT('Ctrl Pts',(-28.9616771780539,21.1919744338817,3.88953620066551));
#54872=CARTESIAN_POINT('Ctrl Pts',(-28.9613856085175,21.1926756262127,3.88970012719846));
#54873=CARTESIAN_POINT('Ctrl Pts',(-28.9610925208102,21.1933759749083,3.88986475847562));
#54874=CARTESIAN_POINT('Ctrl Pts',(-28.960797915745,21.1940754818056,3.89003008861958));
#54875=CARTESIAN_POINT('Ctrl Pts',(-28.9547604581748,21.208410752005,3.89341826433982));
#54876=CARTESIAN_POINT('Ctrl Pts',(-28.9480857142471,21.2223930775751,3.89709988405803));
#54877=CARTESIAN_POINT('Ctrl Pts',(-28.9407802200781,21.2360355854272,3.90102529736883));
#54878=CARTESIAN_POINT('Ctrl Pts',(-28.9404589312627,21.2366355701902,3.90119793338271));
#54879=CARTESIAN_POINT('Ctrl Pts',(-28.9401364145058,21.2372349093322,3.90137104572976));
#54880=CARTESIAN_POINT('Ctrl Pts',(-28.939812669612,21.2378336017067,3.90154462963897));
#54881=CARTESIAN_POINT('Ctrl Pts',(-28.9359701268155,21.2449395085967,3.90360490491386));
#54882=CARTESIAN_POINT('Ctrl Pts',(-28.9319553000605,21.2519530849821,3.90573124712142));
#54883=CARTESIAN_POINT('Ctrl Pts',(-28.9277662154186,21.2588750987062,3.90791660649015));
#54884=CARTESIAN_POINT('Ctrl Pts',(-28.9238452263219,21.2653541132546,3.90996210592255));
#54885=CARTESIAN_POINT('Ctrl Pts',(-28.9197699102247,21.2717553746919,3.91206015529359));
#54886=CARTESIAN_POINT('Ctrl Pts',(-28.915543176381,21.2780716968035,3.91420268904662));
#54887=CARTESIAN_POINT('Ctrl Pts',(-28.9152541757013,21.2785035719702,3.91434918365304));
#54888=CARTESIAN_POINT('Ctrl Pts',(-28.9149646115042,21.2789348366557,3.91449581247848));
#54889=CARTESIAN_POINT('Ctrl Pts',(-28.9146744857417,21.2793654904408,3.91464257259226));
#54890=CARTESIAN_POINT('Ctrl Pts',(-28.9057700776902,21.2925829206963,3.91914686730788));
#54891=CARTESIAN_POINT('Ctrl Pts',(-28.8963265621576,21.30524079736,3.92377989260965));
#54892=CARTESIAN_POINT('Ctrl Pts',(-28.8863569087761,21.3173772818602,3.92847795723015));
#54893=CARTESIAN_POINT('Ctrl Pts',(-28.8861752815226,21.3175983844665,3.92856354662239));
#54894=CARTESIAN_POINT('Ctrl Pts',(-28.8859934794983,21.3178193138715,3.92864915773935));
#54895=CARTESIAN_POINT('Ctrl Pts',(-28.8858115026676,21.3180400701975,3.92873479020661));
#54896=CARTESIAN_POINT('Ctrl Pts',(-28.8756595580032,21.3303554072503,3.9335119701669));
#54897=CARTESIAN_POINT('Ctrl Pts',(-28.8649638851134,21.3421324339506,3.93835551745067));
#54898=CARTESIAN_POINT('Ctrl Pts',(-28.8537165289396,21.3533901769361,3.94320069869318));
#54899=CARTESIAN_POINT('Ctrl Pts',(-28.8536956182929,21.3534111068935,3.94320970666551));
#54900=CARTESIAN_POINT('Ctrl Pts',(-28.8536747057384,21.3534320350552,3.94321871464462));
#54901=CARTESIAN_POINT('Ctrl Pts',(-28.853653791276,21.353452961421,3.94322772263006));
#54902=CARTESIAN_POINT('Ctrl Pts',(-28.8423834682513,21.3647296988866,3.94808191890573));
#54903=CARTESIAN_POINT('Ctrl Pts',(-28.8305594631821,21.3754852655172,3.95293799265001));
#54904=CARTESIAN_POINT('Ctrl Pts',(-28.8181518421502,21.3857193365208,3.95772816499657));
#54905=CARTESIAN_POINT('Ctrl Pts',(-28.8179754092975,21.3858648621084,3.957796279889));
#54906=CARTESIAN_POINT('Ctrl Pts',(-28.817798858339,21.3860102822034,3.95786438143738));
#54907=CARTESIAN_POINT('Ctrl Pts',(-28.817622189181,21.3861555967999,3.95793246944758));
#54908=CARTESIAN_POINT('Ctrl Pts',(-28.8146927985446,21.3885650904719,3.95906145190157));
#54909=CARTESIAN_POINT('Ctrl Pts',(-28.8117308312189,21.3909455061188,3.96018669192006));
#54910=CARTESIAN_POINT('Ctrl Pts',(-28.8087356960771,21.3932966693065,3.96130724892932));
#54911=CARTESIAN_POINT('Ctrl Pts',(-28.8085068196737,21.3934763359154,3.96139287747226));
#54912=CARTESIAN_POINT('Ctrl Pts',(-28.8082777512694,21.3936558303765,3.96147847800928));
#54913=CARTESIAN_POINT('Ctrl Pts',(-28.808048490278,21.3938351528717,3.96156405023994));
#54914=CARTESIAN_POINT('Ctrl Pts',(-28.8050966456304,21.3961440155534,3.96266583353729));
#54915=CARTESIAN_POINT('Ctrl Pts',(-28.802109551168,21.3984267656514,3.96376410259036));
#54916=CARTESIAN_POINT('Ctrl Pts',(-28.7991010675383,21.4006726193195,3.96485276880369));
#54917=CARTESIAN_POINT('Ctrl Pts',(-28.7988201115451,21.4008823548959,3.96495443706415));
#54918=CARTESIAN_POINT('Ctrl Pts',(-28.7985389685179,21.4010917689656,3.96505602171734));
#54919=CARTESIAN_POINT('Ctrl Pts',(-28.7982576504616,21.4013008521561,3.9651575175244));
#54920=CARTESIAN_POINT('Ctrl Pts',(-28.7920463251258,21.4059172771921,3.96739848095954));
#54921=CARTESIAN_POINT('Ctrl Pts',(-28.7857412868542,21.410379634955,3.96959946571781));
#54922=CARTESIAN_POINT('Ctrl Pts',(-28.779342978021,21.4146896451178,3.97175302079555));
#54923=CARTESIAN_POINT('Ctrl Pts',(-28.778966071058,21.4149435360886,3.97187988086517));
#54924=CARTESIAN_POINT('Ctrl Pts',(-28.7785888389221,21.4151968994391,3.97200657683767));
#54925=CARTESIAN_POINT('Ctrl Pts',(-28.7782112814686,21.4154497356643,3.97213310725282));
#54926=CARTESIAN_POINT('Ctrl Pts',(-28.7651895622522,21.4241698981271,3.97649706172807));
#54927=CARTESIAN_POINT('Ctrl Pts',(-28.7517817007072,21.4322645500552,3.98066442474707));
#54928=CARTESIAN_POINT('Ctrl Pts',(-28.7379728369994,21.4397373496941,3.98457399470782));
#54929=CARTESIAN_POINT('Ctrl Pts',(-28.7374403638241,21.440025502683,3.98472474868548));
#54930=CARTESIAN_POINT('Ctrl Pts',(-28.7369072941828,21.4403127306051,3.98487511891608));
#54931=CARTESIAN_POINT('Ctrl Pts',(-28.7363736271155,21.4405990335943,3.9850251018032));
#54932=CARTESIAN_POINT('Ctrl Pts',(-28.7226661907559,21.4479528319546,3.98887746783095));
#54933=CARTESIAN_POINT('Ctrl Pts',(-28.708564846762,21.4546967924008,3.99247483292586));
#54934=CARTESIAN_POINT('Ctrl Pts',(-28.6940418379805,21.4608120817006,3.99575219618881));
#54935=CARTESIAN_POINT('Ctrl Pts',(-28.6934296259969,21.4610698694256,3.99589035220693));
#54936=CARTESIAN_POINT('Ctrl Pts',(-28.6928166640662,21.4613265394595,3.99602793885868));
#54937=CARTESIAN_POINT('Ctrl Pts',(-28.6922029499329,21.4615820902473,3.99616495113051));
#54938=CARTESIAN_POINT('Ctrl Pts',(-28.6852539391292,21.4644756608685,3.9977163244909));
#54939=CARTESIAN_POINT('Ctrl Pts',(-28.6782083508407,21.4672254747693,3.99919404072758));
#54940=CARTESIAN_POINT('Ctrl Pts',(-28.6710619027125,21.4698274446379,4.00059030840056));
#54941=CARTESIAN_POINT('Ctrl Pts',(-28.6704499885629,21.4700502381363,4.00070986372797));
#54942=CARTESIAN_POINT('Ctrl Pts',(-28.6698373005598,21.4702719599817,4.00082882902828));
#54943=CARTESIAN_POINT('Ctrl Pts',(-28.6692238485867,21.4704926025662,4.00094719650824));
#54944=CARTESIAN_POINT('Ctrl Pts',(-28.6620401551094,21.4730763886888,4.00233331266908));
#54945=CARTESIAN_POINT('Ctrl Pts',(-28.6547457476138,21.4755124549176,4.00363754090848));
#54946=CARTESIAN_POINT('Ctrl Pts',(-28.6474356860117,21.4777684558703,4.00483716666479));
#54947=CARTESIAN_POINT('Ctrl Pts',(-28.6468600465228,21.4779461073466,4.00493163262073));
#54948=CARTESIAN_POINT('Ctrl Pts',(-28.6462842497821,21.4781226628457,4.00502546186105));
#54949=CARTESIAN_POINT('Ctrl Pts',(-28.6457083335891,21.4782981094701,4.00511864492646));
#54950=CARTESIAN_POINT('Ctrl Pts',(-28.6304080123218,21.4829591864661,4.00759423226838));
#54951=CARTESIAN_POINT('Ctrl Pts',(-28.6149415475987,21.4868701345595,4.00963042415946));
#54952=CARTESIAN_POINT('Ctrl Pts',(-28.5993223066573,21.4900357985373,4.01119295353938));
#54953=CARTESIAN_POINT('Ctrl Pts',(-28.5988756076155,21.4901263342471,4.0112376407543));
#54954=CARTESIAN_POINT('Ctrl Pts',(-28.5984287796622,21.4902162615444,4.01128194112185));
#54955=CARTESIAN_POINT('Ctrl Pts',(-28.5979818227772,21.4903055806385,4.01132585388403));
#54956=CARTESIAN_POINT('Ctrl Pts',(-28.5822122630561,21.4934569422931,4.01287518660258));
#54957=CARTESIAN_POINT('Ctrl Pts',(-28.566282210323,21.4958512063425,4.01394216943519));
#54958=CARTESIAN_POINT('Ctrl Pts',(-28.5501870504247,21.497474885185,4.01449425451777));
#54959=CARTESIAN_POINT('Ctrl Pts',(-28.5499299179448,21.4975008246954,4.01450307449889));
#54960=CARTESIAN_POINT('Ctrl Pts',(-28.5496727433489,21.497526567513,4.01451176304298));
#54961=CARTESIAN_POINT('Ctrl Pts',(-28.5494155266162,21.4975521135813,4.0145203200153));
#54962=CARTESIAN_POINT('Ctrl Pts',(-28.5331159748128,21.4991709408639,4.0150625662842));
#54963=CARTESIAN_POINT('Ctrl Pts',(-28.5166471370518,21.5,4.01507664076422));
#54964=CARTESIAN_POINT('Ctrl Pts',(-28.5,21.5,4.01452801010865));
#54965=CARTESIAN_POINT('',(-28.5,21.5,4.40714435599954));
#54966=CARTESIAN_POINT('Origin',(-174.463204856321,34.9999999945948,6.54993637452805E-10));
#54967=CARTESIAN_POINT('',(33.,30.9999999945948,6.54994127311525E-10));
#54968=CARTESIAN_POINT('Origin',(33.,34.9999999945948,6.54993637452805E-10));
#54969=CARTESIAN_POINT('',(-174.463204856321,30.9999999945948,6.54994127311525E-10));
#54970=CARTESIAN_POINT('Origin',(-174.463204856321,34.9999999945948,6.54993637452805E-10));
#54971=CARTESIAN_POINT('',(-39.,30.9999999945948,6.54994127311525E-10));
#54972=CARTESIAN_POINT('',(-174.463204856321,30.9999999945948,6.54994127311525E-10));
#54973=CARTESIAN_POINT('Origin',(-39.,34.9999999945948,6.54993637452805E-10));
#54974=CARTESIAN_POINT('Origin',(6.61363325216158E-15,57.,-24.));
#54975=CARTESIAN_POINT('',(-4.19913133791448,57.,-27.5520833333334));
#54976=CARTESIAN_POINT('',(-4.19913133791448,57.,-27.5520833333334));
#54977=CARTESIAN_POINT('',(4.1991313379145,57.,-27.5520833333334));
#54978=CARTESIAN_POINT('Origin',(6.61363325216158E-15,57.,-24.));
#54979=CARTESIAN_POINT('',(4.1991313379145,57.,-27.5520833333334));
#54980=CARTESIAN_POINT('Origin',(6.61363325216158E-15,69.8123087321227,
-24.));
#54981=CARTESIAN_POINT('',(6.91979495194842E-15,52.,-21.5));
#54982=CARTESIAN_POINT('Origin',(6.61363325216158E-15,52.,-24.));
#54983=CARTESIAN_POINT('',(6.91979495194842E-15,57.,-21.5));
#54984=CARTESIAN_POINT('',(6.91979495194842E-15,69.8123087321227,-21.5));
#54985=CARTESIAN_POINT('Origin',(6.61363325216158E-15,57.,-24.));
#54986=CARTESIAN_POINT('Origin',(33.,25.2727793885888,2.53685745363396));
#54987=CARTESIAN_POINT('',(16.5015526417024,25.4697390379769,2.99642996887271));
#54988=CARTESIAN_POINT('Ctrl Pts',(17.3583590725823,24.8843482494656,2.85169179564682));
#54989=CARTESIAN_POINT('Ctrl Pts',(17.3427646761208,24.8904421031615,2.85921017028675));
#54990=CARTESIAN_POINT('Ctrl Pts',(17.3271931898089,24.8967466727953,2.86654362190466));
#54991=CARTESIAN_POINT('Ctrl Pts',(17.1751346754118,24.9602776965675,2.93623867167078));
#54992=CARTESIAN_POINT('Ctrl Pts',(17.0358151286748,25.0347314689897,2.98601836429146));
#54993=CARTESIAN_POINT('Ctrl Pts',(16.8292928010538,25.1726430909796,3.0295764232713));
#54994=CARTESIAN_POINT('Ctrl Pts',(16.7546033612845,25.2287590875601,3.03852282224654));
#54995=CARTESIAN_POINT('Ctrl Pts',(16.6187499796368,25.3457029504125,3.03477909002088));
#54996=CARTESIAN_POINT('Ctrl Pts',(16.5558465481405,25.4073521349368,3.02316721276094));
#54997=CARTESIAN_POINT('Ctrl Pts',(16.5015526417035,25.4697390378793,2.99642996864261));
#54998=CARTESIAN_POINT('',(33.,25.4697390378784,2.99642996864299));
#54999=CARTESIAN_POINT('',(16.1963226914819,25.4697390378784,2.99642996864299));
#55000=CARTESIAN_POINT('Origin',(33.,25.2727793885888,2.53685745363396));
#55001=CARTESIAN_POINT('Origin',(33.,21.,6.));
#55002=CARTESIAN_POINT('',(23.,21.,8.067));
#55003=CARTESIAN_POINT('Origin',(23.,21.,6.));
#55004=CARTESIAN_POINT('',(33.,21.,8.067));
#55005=CARTESIAN_POINT('',(33.,21.,8.067));
#55006=CARTESIAN_POINT('Origin',(33.,21.,6.));
#55007=CARTESIAN_POINT('Origin',(1.25791587597333E-15,20.5440037453175,
-6.93889390390723E-15));
#55008=CARTESIAN_POINT('',(-6.64306116621187E-16,18.7883865373756,14.8183541121548));
#55009=CARTESIAN_POINT('Origin',(-1.13014538236401E-15,20.5440037453175,
19.5));
#55010=CARTESIAN_POINT('Origin',(1.15041887658705E-15,18.7883865373756,
-5.08824700431546E-15));
#55011=CARTESIAN_POINT('Origin',(7.22953690019729E-16,11.8071196962708,
-1.26385727337141E-15));
#55012=CARTESIAN_POINT('',(-1.41238078159923E-15,11.8071196962708,17.4363291775691));
#55013=CARTESIAN_POINT('',(-1.41238078159923E-15,11.8071196962708,17.4363291775691));
#55014=CARTESIAN_POINT('Origin',(7.22953690019729E-16,11.8071196962708,
-1.26385727337141E-15));
#55015=CARTESIAN_POINT('Origin',(7.01454290142472E-16,11.4559962546824,
-3.46944695195362E-15));
#55016=CARTESIAN_POINT('Origin',(-1.31921292845066E-15,11.4559962546824,
16.5));
#55017=CARTESIAN_POINT('Origin',(6.61363325216158E-15,88.645101838174,24.));
#55018=CARTESIAN_POINT('',(6.91979495194842E-15,52.,26.5));
#55019=CARTESIAN_POINT('Origin',(6.61363325216158E-15,52.,24.));
#55020=CARTESIAN_POINT('',(6.91979495194842E-15,57.,26.5));
#55021=CARTESIAN_POINT('',(6.91979495194842E-15,88.645101838174,26.5));
#55022=CARTESIAN_POINT('Origin',(6.61363325216158E-15,57.,24.));
#55023=CARTESIAN_POINT('Origin',(0.5,20.8180194846606,-32.6819805153395));
#55024=CARTESIAN_POINT('',(0.5,17.9895923599144,-32.6819805153395));
#55025=CARTESIAN_POINT('Origin',(0.5,19.4038059222875,-34.0961940777126));
#55026=CARTESIAN_POINT('',(0.5,19.4038059222875,-31.2677669529664));
#55027=CARTESIAN_POINT('',(0.5,19.4038059222875,-31.2677669529664));
#55028=CARTESIAN_POINT('Origin',(0.5,20.8180194846606,-32.6819805153395));
#55029=CARTESIAN_POINT('Origin',(4.5,24.,-35.));
#55030=CARTESIAN_POINT('Origin',(0.5,20.8180194846606,-32.6819805153395));
#55031=CARTESIAN_POINT('Origin',(23.,21.,6.));
#55032=CARTESIAN_POINT('Origin',(33.,26.9685342791486,5.07400811733573));
#55033=CARTESIAN_POINT('',(15.9496310351764,26.7715746300098,4.6144356021428));
#55034=CARTESIAN_POINT('Ctrl Pts',(16.6650252178836,27.3912430012986,4.80695505852849));
#55035=CARTESIAN_POINT('Ctrl Pts',(16.6630100761954,27.3903535292942,4.80554714514958));
#55036=CARTESIAN_POINT('Ctrl Pts',(16.6610051967559,27.3894616239388,4.80415074255901));
#55037=CARTESIAN_POINT('Ctrl Pts',(16.6589687547288,27.388548553701,4.80273701829963));
#55038=CARTESIAN_POINT('Ctrl Pts',(16.6569323127016,27.3876354834631,4.80132329404023));
#55039=CARTESIAN_POINT('Ctrl Pts',(16.6548961566558,27.3867154046794,4.79991437939278));
#55040=CARTESIAN_POINT('Ctrl Pts',(16.6528602685867,27.385788334266,4.79851028887233));
#55041=CARTESIAN_POINT('Ctrl Pts',(16.6487884924487,27.3839341934393,4.79570210783142));
#55042=CARTESIAN_POINT('Ctrl Pts',(16.6447177882178,27.3820520875034,4.79291322229783));
#55043=CARTESIAN_POINT('Ctrl Pts',(16.6406480126451,27.3801421344537,4.79014375984945));
#55044=CARTESIAN_POINT('Ctrl Pts',(16.6325084614997,27.3763222283545,4.78460483495268));
#55045=CARTESIAN_POINT('Ctrl Pts',(16.6243726249869,27.372390956667,4.7791435868405));
#55046=CARTESIAN_POINT('Ctrl Pts',(16.6162393697714,27.368348990199,4.7737612242166));
#55047=CARTESIAN_POINT('Ctrl Pts',(16.6081061145559,27.364307023731,4.7683788615927));
#55048=CARTESIAN_POINT('Ctrl Pts',(16.5999754406376,27.3601543628628,4.76307538424318));
#55049=CARTESIAN_POINT('Ctrl Pts',(16.5918462155288,27.3558913214684,4.75785226689918));
#55050=CARTESIAN_POINT('Ctrl Pts',(16.5837169904199,27.351628280074,4.75262914955517));
#55051=CARTESIAN_POINT('Ctrl Pts',(16.5755828927852,27.3472513208491,4.7474824908028));
#55052=CARTESIAN_POINT('Ctrl Pts',(16.5674672015749,27.34277402452,4.74242914788145));
#55053=CARTESIAN_POINT('Ctrl Pts',(16.5408797860593,27.3281061749427,4.72587414048764));
#55054=CARTESIAN_POINT('Ctrl Pts',(16.5144995283404,27.3123723786464,4.71032264739845));
#55055=CARTESIAN_POINT('Ctrl Pts',(16.4882866689286,27.2955991018421,4.69581689353952));
#55056=CARTESIAN_POINT('Ctrl Pts',(16.4824940898877,27.2918925038652,4.69261137809167));
#55057=CARTESIAN_POINT('Ctrl Pts',(16.4767096854409,27.2881350164069,4.68945708527442));
#55058=CARTESIAN_POINT('Ctrl Pts',(16.4709330265328,27.2843267278126,4.68635475495276));
#55059=CARTESIAN_POINT('Ctrl Pts',(16.4464825909653,27.2682076672312,4.67322375157423));
#55060=CARTESIAN_POINT('Ctrl Pts',(16.4221714637226,27.251181209635,4.6610210419516));
#55061=CARTESIAN_POINT('Ctrl Pts',(16.3979687202308,27.2332322814993,4.64982069702305));
#55062=CARTESIAN_POINT('Ctrl Pts',(16.3905773239509,27.2277507690131,4.64640016794677));
#55063=CARTESIAN_POINT('Ctrl Pts',(16.3831960361998,27.222183128309,4.6430734765975));
#55064=CARTESIAN_POINT('Ctrl Pts',(16.375823976153,27.2165287627257,4.63984370594838));
#55065=CARTESIAN_POINT('Ctrl Pts',(16.3679461041414,27.2104864396722,4.63639233419622));
#55066=CARTESIAN_POINT('Ctrl Pts',(16.3600787695375,27.2043448876271,4.63305150714274));
#55067=CARTESIAN_POINT('Ctrl Pts',(16.352220780091,27.1981025685342,4.62982527152944));
#55068=CARTESIAN_POINT('Ctrl Pts',(16.3443627906444,27.1918602494413,4.62659903591615));
#55069=CARTESIAN_POINT('Ctrl Pts',(16.336507501934,27.1855117252021,4.62348488529172));
#55070=CARTESIAN_POINT('Ctrl Pts',(16.3286750968802,27.179072825651,4.62049569144569));
#55071=CARTESIAN_POINT('Ctrl Pts',(16.3130102867726,27.1661950265487,4.61451730375362));
#55072=CARTESIAN_POINT('Ctrl Pts',(16.2975164416325,27.1530220764324,4.60906778525686));
#55073=CARTESIAN_POINT('Ctrl Pts',(16.2821841177728,27.139559361384,4.60416727061593));
#55074=CARTESIAN_POINT('Ctrl Pts',(16.2605485852015,27.1205620448264,4.59725212552117));
#55075=CARTESIAN_POINT('Ctrl Pts',(16.2392344529781,27.1009901681504,4.59142869627441));
#55076=CARTESIAN_POINT('Ctrl Pts',(16.2182190259903,27.0808433725107,4.58678469061224));
#55077=CARTESIAN_POINT('Ctrl Pts',(16.2094486983112,27.0724355490796,4.5848466166714));
#55078=CARTESIAN_POINT('Ctrl Pts',(16.200730393949,27.0639276706392,4.58311455657391));
#55079=CARTESIAN_POINT('Ctrl Pts',(16.1920624633548,27.0553203598125,4.58159754047634));
#55080=CARTESIAN_POINT('Ctrl Pts',(16.1773434663233,27.0407043010969,4.57902149822564));
#55081=CARTESIAN_POINT('Ctrl Pts',(16.162769897045,27.0257998208095,4.57706420508458));
#55082=CARTESIAN_POINT('Ctrl Pts',(16.1483338722369,27.0106028593833,4.57578102598377));
#55083=CARTESIAN_POINT('Ctrl Pts',(16.1411158598328,27.0030043786702,4.57513943643336));
#55084=CARTESIAN_POINT('Ctrl Pts',(16.1339322335463,26.9953327615401,4.57466662768078));
#55085=CARTESIAN_POINT('Ctrl Pts',(16.1267819344675,26.9875871364787,4.57437126058119));
#55086=CARTESIAN_POINT('Ctrl Pts',(16.1196316353886,26.9798415114174,4.5740758934816));
#55087=CARTESIAN_POINT('Ctrl Pts',(16.112507031152,26.9720133755952,4.57395805152907));
#55088=CARTESIAN_POINT('Ctrl Pts',(16.1054312238926,26.964128732385,4.57402752655474));
#55089=CARTESIAN_POINT('Ctrl Pts',(16.0871593099881,26.9437681549098,4.5742069324714));
#55090=CARTESIAN_POINT('Ctrl Pts',(16.0694041230973,26.9232488322717,4.57562785316267));
#55091=CARTESIAN_POINT('Ctrl Pts',(16.0521364611193,26.9026061632371,4.57837369204593));
#55092=CARTESIAN_POINT('Ctrl Pts',(16.0426564821845,26.8912732990742,4.57988116276228));
#55093=CARTESIAN_POINT('Ctrl Pts',(16.0333234447536,26.8799036284063,4.58178874960394));
#55094=CARTESIAN_POINT('Ctrl Pts',(16.0241325167303,26.8685069912516,4.58411573968941));
#55095=CARTESIAN_POINT('Ctrl Pts',(16.0111664730231,26.8524292573071,4.58739852626739));
#55096=CARTESIAN_POINT('Ctrl Pts',(15.9984836522186,26.8362950343224,4.59151528406382));
#55097=CARTESIAN_POINT('Ctrl Pts',(15.9860712395022,26.8201300060185,4.59653961395909));
#55098=CARTESIAN_POINT('Ctrl Pts',(15.9736588267857,26.8039649777146,4.60156394385436));
#55099=CARTESIAN_POINT('Ctrl Pts',(15.9615168221573,26.7877689169305,4.60749519358178));
#55100=CARTESIAN_POINT('Ctrl Pts',(15.9496310354892,26.771574629859,4.61443560232671));
#55101=CARTESIAN_POINT('',(33.,26.771574629859,4.6144356023267));
#55102=CARTESIAN_POINT('',(15.8907046022141,26.771574629859,4.6144356023267));
#55103=CARTESIAN_POINT('Origin',(33.,26.9685342791486,5.07400811733573));
#55104=CARTESIAN_POINT('Origin',(33.,25.7867763834111,2.31657302728156));
#55105=CARTESIAN_POINT('',(16.4143885868334,25.9837360327007,2.77614554229059));
#55106=CARTESIAN_POINT('',(33.,25.9837360327007,2.77614554229058));
#55107=CARTESIAN_POINT('',(33.,25.9837360327007,2.77614554229058));
#55108=CARTESIAN_POINT('Ctrl Pts',(16.4143885868334,25.9837360327007,2.77614554229059));
#55109=CARTESIAN_POINT('Ctrl Pts',(16.4633974984172,26.0470957947593,2.74899135855118));
#55110=CARTESIAN_POINT('Ctrl Pts',(16.5255478930996,26.1033294237433,2.70947695324141));
#55111=CARTESIAN_POINT('Ctrl Pts',(16.6761004083686,26.1963150747648,2.61126695343904));
#55112=CARTESIAN_POINT('Ctrl Pts',(16.7580192832196,26.2291178133552,2.55689292095467));
#55113=CARTESIAN_POINT('Ctrl Pts',(17.014944149898,26.2965251314195,2.38873820449799));
#55114=CARTESIAN_POINT('Ctrl Pts',(17.1872180079846,26.2925712666988,2.2799008816023));
#55115=CARTESIAN_POINT('Ctrl Pts',(17.3257575088157,26.2722073998847,2.19674998526149));
#55116=CARTESIAN_POINT('Ctrl Pts',(17.3277958722061,26.2719052005207,2.19553219265278));
#55117=CARTESIAN_POINT('Ctrl Pts',(17.3292733299329,26.2716827465251,2.19464747699608));
#55118=CARTESIAN_POINT('Origin',(33.,25.7867763834111,2.31657302728156));
#55119=CARTESIAN_POINT('Origin',(16.0330469265826,57.,-13.5625));
#55120=CARTESIAN_POINT('',(16.0330469265826,57.,-13.5625));
#55121=CARTESIAN_POINT('',(16.0330469265826,53.,-13.5625));
#55122=CARTESIAN_POINT('',(16.0330469265826,57.,-13.5625));
#55123=CARTESIAN_POINT('',(16.0330469265826,53.,-13.5625));
#55124=CARTESIAN_POINT('',(16.0330469265826,57.,-13.5625));
#55125=CARTESIAN_POINT('Origin',(6.61287431064084E-15,57.,0.));
#55126=CARTESIAN_POINT('',(16.0330469265826,57.,13.5625));
#55127=CARTESIAN_POINT('',(16.0330469265826,53.,13.5625));
#55128=CARTESIAN_POINT('',(16.0330469265826,57.,13.5625));
#55129=CARTESIAN_POINT('Origin',(6.61287431064084E-15,53.,0.));
#55130=CARTESIAN_POINT('Origin',(6.61287431064084E-15,57.,0.));
#55131=CARTESIAN_POINT('Origin',(6.61363325216158E-15,57.,24.));
#55132=CARTESIAN_POINT('',(4.1991313379145,57.,27.5520833333334));
#55133=CARTESIAN_POINT('',(-4.19913133791448,57.,27.5520833333334));
#55134=CARTESIAN_POINT('Origin',(6.61363325216158E-15,57.,24.));
#55135=CARTESIAN_POINT('',(4.1991313379145,57.,27.5520833333334));
#55136=CARTESIAN_POINT('',(-16.0330469265826,57.,-13.5625));
#55137=CARTESIAN_POINT('',(-4.19913133791448,57.,-27.5520833333334));
#55138=CARTESIAN_POINT('',(-16.0330469265826,57.,13.5625));
#55139=CARTESIAN_POINT('Origin',(6.61287431064084E-15,57.,0.));
#55140=CARTESIAN_POINT('',(-4.19913133791448,57.,27.5520833333334));
#55141=CARTESIAN_POINT('Origin',(4.1991313379145,57.,27.5520833333334));
#55142=CARTESIAN_POINT('',(4.1991313379145,53.,27.5520833333334));
#55143=CARTESIAN_POINT('',(4.1991313379145,57.,27.5520833333334));
#55144=CARTESIAN_POINT('',(4.1991313379145,53.,27.5520833333334));
#55145=CARTESIAN_POINT('Origin',(6.61363325216158E-15,57.,24.));
#55146=CARTESIAN_POINT('',(-4.19913133791448,53.,27.5520833333334));
#55147=CARTESIAN_POINT('',(-4.19913133791448,57.,27.5520833333334));
#55148=CARTESIAN_POINT('Origin',(6.61363325216158E-15,53.,24.));
#55149=CARTESIAN_POINT('Origin',(-4.19913133791448,57.,27.5520833333334));
#55150=CARTESIAN_POINT('',(-16.0330469265826,53.,13.5625));
#55151=CARTESIAN_POINT('',(-16.0330469265826,57.,13.5625));
#55152=CARTESIAN_POINT('',(-4.19913133791448,53.,27.5520833333334));
#55153=CARTESIAN_POINT('Origin',(6.61287431064084E-15,57.,0.));
#55154=CARTESIAN_POINT('',(-16.0330469265826,53.,-13.5625));
#55155=CARTESIAN_POINT('',(-16.0330469265826,57.,-13.5625));
#55156=CARTESIAN_POINT('Origin',(6.61287431064084E-15,53.,0.));
#55157=CARTESIAN_POINT('Origin',(-38.,21.,7.));
#55158=CARTESIAN_POINT('',(-38.,23.6912516952905,7.08464226247173));
#55159=CARTESIAN_POINT('Ctrl Pts',(-16.5433923268431,19.8911992509365,0.971393813304918));
#55160=CARTESIAN_POINT('Ctrl Pts',(-16.407897387297,20.5,0.963437830432189));
#55161=CARTESIAN_POINT('Ctrl Pts',(-17.0305720504421,20.5,1.));
#55162=CARTESIAN_POINT('Ctrl Pts',(-16.5460230165557,19.891199259935,0.926591628387505));
#55163=CARTESIAN_POINT('Ctrl Pts',(-16.4084072798099,20.5016889125451,0.948330479285953));
#55164=CARTESIAN_POINT('Ctrl Pts',(-17.0332802188509,20.5,0.976939153062529));
#55165=CARTESIAN_POINT('Ctrl Pts',(-16.5475841116722,19.8950096166727,0.882278171409564));
#55166=CARTESIAN_POINT('Ctrl Pts',(-16.4096816508543,20.5038083386403,0.933858336274406));
#55167=CARTESIAN_POINT('Ctrl Pts',(-17.0350550463224,20.5015876519666,0.954134911206445));
#55168=CARTESIAN_POINT('Ctrl Pts',(-16.5487479801528,19.909965914742,0.794606678521227));
#55169=CARTESIAN_POINT('Ctrl Pts',(-16.4137261112856,20.5090429824563,0.904356864073263));
#55170=CARTESIAN_POINT('Ctrl Pts',(-17.0368945748498,20.5078194436758,0.909023217144905));
#55171=CARTESIAN_POINT('Ctrl Pts',(-16.5483503357205,19.9211125982883,0.751247887293482));
#55172=CARTESIAN_POINT('Ctrl Pts',(-16.4164789427531,20.5121455900044,0.889404076489988));
#55173=CARTESIAN_POINT('Ctrl Pts',(-17.0369589041897,20.5124638957006,0.88671544260711));
#55174=CARTESIAN_POINT('Ctrl Pts',(-16.5467905191782,19.9397158472753,0.697663995679634));
#55175=CARTESIAN_POINT('Ctrl Pts',(-16.4206834264394,20.5171906160361,0.869517502731721));
#55176=CARTESIAN_POINT('Ctrl Pts',(-17.0361078121662,20.5202152482318,0.859147613733574));
#55177=CARTESIAN_POINT('Ctrl Pts',(-16.5464256319663,19.9436710140189,0.686978084831627));
#55178=CARTESIAN_POINT('Ctrl Pts',(-16.4215581463202,20.5182547550123,0.865499434449415));
#55179=CARTESIAN_POINT('Ctrl Pts',(-17.0358911926661,20.5218632349471,0.853649964743502));
#55180=CARTESIAN_POINT('Ctrl Pts',(-16.545594966273,19.9520567304156,0.665669029571539));
#55181=CARTESIAN_POINT('Ctrl Pts',(-16.4233747022659,20.5205189452442,0.857341577641165));
#55182=CARTESIAN_POINT('Ctrl Pts',(-17.0353693593641,20.5253572827868,0.842686968399742));
#55183=CARTESIAN_POINT('Ctrl Pts',(-16.5451281146306,19.9564966696759,0.655025666938477));
#55184=CARTESIAN_POINT('Ctrl Pts',(-16.4243180509428,20.5217209530893,0.853195047255348));
#55185=CARTESIAN_POINT('Ctrl Pts',(-17.0350633970533,20.5272072572878,0.837211219553851));
#55186=CARTESIAN_POINT('Ctrl Pts',(-16.5435950680448,19.9704461060348,0.623402194616967));
#55187=CARTESIAN_POINT('Ctrl Pts',(-16.4272156936075,20.5255308654207,0.840655045305963));
#55188=CARTESIAN_POINT('Ctrl Pts',(-17.0340268420252,20.5330195239982,0.820941647960808));
#55189=CARTESIAN_POINT('Ctrl Pts',(-16.5423960960644,19.9805919436888,0.602698030449193));
#55190=CARTESIAN_POINT('Ctrl Pts',(-16.4292443604542,20.5283496476911,0.832125812433268));
#55191=CARTESIAN_POINT('Ctrl Pts',(-17.0331776130024,20.5372469546676,0.810289716104096));
#55192=CARTESIAN_POINT('Ctrl Pts',(-16.5383740427822,20.0135045500505,0.541688220646475));
#55193=CARTESIAN_POINT('Ctrl Pts',(-16.4355081831529,20.5378206889875,0.806060489096857));
#55194=CARTESIAN_POINT('Ctrl Pts',(-17.0302461821317,20.5509605425891,0.778900346429098));
#55195=CARTESIAN_POINT('Ctrl Pts',(-16.5351244462826,20.0387346852731,0.502480294969622));
#55196=CARTESIAN_POINT('Ctrl Pts',(-16.4399382995849,20.5455007368547,0.78792924810244));
#55197=CARTESIAN_POINT('Ctrl Pts',(-17.0277791213822,20.5614730977609,0.758726732122362));
#55198=CARTESIAN_POINT('Ctrl Pts',(-16.5298329930104,20.0814825069704,0.445834797421413));
#55199=CARTESIAN_POINT('Ctrl Pts',(-16.4467056213962,20.5599852183674,0.759646126498156));
#55200=CARTESIAN_POINT('Ctrl Pts',(-17.0236814376451,20.5792846899537,0.729577577968062));
#55201=CARTESIAN_POINT('Ctrl Pts',(-16.5279999224092,20.0965518409253,0.427315285485088));
#55202=CARTESIAN_POINT('Ctrl Pts',(-16.4489689372401,20.5652690924714,0.750102567161397));
#55203=CARTESIAN_POINT('Ctrl Pts',(-17.0222495454306,20.585563579545,0.72004706252039));
#55204=CARTESIAN_POINT('Ctrl Pts',(-16.5252050045946,20.1204096270575,0.400087134515338));
#55205=CARTESIAN_POINT('Ctrl Pts',(-16.4523742507172,20.5740318567946,0.735583389128628));
#55206=CARTESIAN_POINT('Ctrl Pts',(-17.0200525657724,20.5955043231922,0.706033937512207));
#55207=CARTESIAN_POINT('Ctrl Pts',(-16.5242658526117,20.1285713796292,0.391103018058698));
#55208=CARTESIAN_POINT('Ctrl Pts',(-16.4535078916128,20.5770823745325,0.730724230937434));
#55209=CARTESIAN_POINT('Ctrl Pts',(-17.0193120752144,20.5989050538913,0.701410047075698));
#55210=CARTESIAN_POINT('Ctrl Pts',(-16.5223828507085,20.1453196286114,0.373320964386736));
#55211=CARTESIAN_POINT('Ctrl Pts',(-16.4557745374995,20.5834720397517,0.720959701653889));
#55212=CARTESIAN_POINT('Ctrl Pts',(-17.0178235516284,20.6058834904285,0.692257749627275));
#55213=CARTESIAN_POINT('Ctrl Pts',(-16.5214408462345,20.1538906455271,0.364540612191054));
#55214=CARTESIAN_POINT('Ctrl Pts',(-16.4569053132703,20.5868043886051,0.716064040471107));
#55215=CARTESIAN_POINT('Ctrl Pts',(-17.0170769643931,20.6094547473659,0.687738393835301));
#55216=CARTESIAN_POINT('Ctrl Pts',(-16.5167801741158,20.1974911117525,0.321422255422651));
#55217=CARTESIAN_POINT('Ctrl Pts',(-16.4624823349259,20.6039933346536,0.691819606845547));
#55218=CARTESIAN_POINT('Ctrl Pts',(-17.0133752701266,20.6276216101941,0.665544000743011));
#55219=CARTESIAN_POINT('Ctrl Pts',(-16.5131856715377,20.2349569684753,0.289196318408042));
#55220=CARTESIAN_POINT('Ctrl Pts',(-16.4668466775319,20.6198679793505,0.672490019195905));
#55221=CARTESIAN_POINT('Ctrl Pts',(-17.0104951031623,20.6432323821084,0.648953506162977));
#55222=CARTESIAN_POINT('Ctrl Pts',(-16.5069251772217,20.3149416326476,0.229133699455863));
#55223=CARTESIAN_POINT('Ctrl Pts',(-16.475404952459,20.6561212773607,0.63516338539478));
#55224=CARTESIAN_POINT('Ctrl Pts',(-17.0054632578451,20.6765593259124,0.618027613096065));
#55225=CARTESIAN_POINT('Ctrl Pts',(-16.5042566734341,20.3574602973108,0.201297028703423));
#55226=CARTESIAN_POINT('Ctrl Pts',(-16.4796079694452,20.676460019731,0.617125809267408));
#55227=CARTESIAN_POINT('Ctrl Pts',(-17.0033094070265,20.6942754368156,0.603692232152243));
#55228=CARTESIAN_POINT('Ctrl Pts',(-16.5014702539652,20.4251655989665,0.162918760220545));
#55229=CARTESIAN_POINT('Ctrl Pts',(-16.4859952506699,20.7105903622794,0.591789565823027));
#55230=CARTESIAN_POINT('Ctrl Pts',(-17.0010678009979,20.7224859779327,0.583925720088675));
#55231=CARTESIAN_POINT('Ctrl Pts',(-16.5007448950925,20.4484653982754,0.150660370006624));
#55232=CARTESIAN_POINT('Ctrl Pts',(-16.488138164386,20.7225596194786,0.583636449987115));
#55233=CARTESIAN_POINT('Ctrl Pts',(-17.0004860701606,20.732194227621,0.577611671372152));
#55234=CARTESIAN_POINT('Ctrl Pts',(-16.4998065086035,20.4956762612484,0.127659535369717));
#55235=CARTESIAN_POINT('Ctrl Pts',(-16.4924238463118,20.7472907980385,0.568298316995553));
#55236=CARTESIAN_POINT('Ctrl Pts',(-16.9997422762988,20.7518654214002,0.565763816818942));
#55237=CARTESIAN_POINT('Ctrl Pts',(-16.4995891679361,20.5196569119538,0.116872129943027));
#55238=CARTESIAN_POINT('Ctrl Pts',(-16.4945751007252,20.7600913803133,0.561073592164906));
#55239=CARTESIAN_POINT('Ctrl Pts',(-16.9995767220622,20.7618573347902,0.560206868064739));
#55240=CARTESIAN_POINT('Ctrl Pts',(-16.499654466181,20.5440037453176,0.106782473437618));
#55241=CARTESIAN_POINT('Ctrl Pts',(-16.4967580121734,20.7733226724976,0.554332420210066));
#55242=CARTESIAN_POINT('Ctrl Pts',(-16.9996439954592,20.7720018726588,0.555009152983015));
#55243=CARTESIAN_POINT('Origin',(-16.9996439954592,20.5440037453176,0.110018305966033));
#55244=CARTESIAN_POINT('Ctrl Pts',(-16.5433923268431,19.8911992509365,0.971393813304911));
#55245=CARTESIAN_POINT('Ctrl Pts',(-16.5460324658657,19.8911992599673,0.926430701110204));
#55246=CARTESIAN_POINT('Ctrl Pts',(-16.5475861334947,19.895035620538,0.882125735271342));
#55247=CARTESIAN_POINT('Ctrl Pts',(-16.5481658959472,19.9024884294234,0.83844251359447));
#55248=CARTESIAN_POINT('Ctrl Pts',(-16.5482102764594,19.9030589380404,0.835098585852582));
#55249=CARTESIAN_POINT('Ctrl Pts',(-16.5482489443743,19.9036506508715,0.831758298116806));
#55250=CARTESIAN_POINT('Ctrl Pts',(-16.5482819658505,19.9042635663159,0.828421646010209));
#55251=CARTESIAN_POINT('Ctrl Pts',(-16.5485141637358,19.9085734181441,0.804959231555224));
#55252=CARTESIAN_POINT('Ctrl Pts',(-16.5484668356028,19.9139332687769,0.781677203367974));
#55253=CARTESIAN_POINT('Ctrl Pts',(-16.548163843894,19.9203370163541,0.758574853429922));
#55254=CARTESIAN_POINT('Ctrl Pts',(-16.5480123480396,19.9235388901426,0.747023678460895));
#55255=CARTESIAN_POINT('Ctrl Pts',(-16.5477968713962,19.9270019786639,0.735517459337272));
#55256=CARTESIAN_POINT('Ctrl Pts',(-16.5475200008255,19.930727105518,0.724056384611012));
#55257=CARTESIAN_POINT('Ctrl Pts',(-16.5473935804081,19.9324280161282,0.718823203468597));
#55258=CARTESIAN_POINT('Ctrl Pts',(-16.5472542508089,19.934184833772,0.713595822387411));
#55259=CARTESIAN_POINT('Ctrl Pts',(-16.5471024601299,19.9359952994074,0.708380803007421));
#55260=CARTESIAN_POINT('Ctrl Pts',(-16.5469218173869,19.9381498946732,0.702174523336911));
#55261=CARTESIAN_POINT('Ctrl Pts',(-16.5467235931023,19.9403808422703,0.695985801536031));
#55262=CARTESIAN_POINT('Ctrl Pts',(-16.5465088555626,19.9426837122906,0.689825608166473));
#55263=CARTESIAN_POINT('Ctrl Pts',(-16.5463513980074,19.9443723051828,0.685308610400069));
#55264=CARTESIAN_POINT('Ctrl Pts',(-16.5461851308859,19.9460989058903,0.68080855796723));
#55265=CARTESIAN_POINT('Ctrl Pts',(-16.5460102979366,19.9478638776901,0.676323558973994));
#55266=CARTESIAN_POINT('Ctrl Pts',(-16.5457463457432,19.9505285251712,0.669552379246432));
#55267=CARTESIAN_POINT('Ctrl Pts',(-16.5454624471804,19.953284362771,0.662807405302023));
#55268=CARTESIAN_POINT('Ctrl Pts',(-16.5451605304242,19.9561229704575,0.656105186271793));
#55269=CARTESIAN_POINT('Ctrl Pts',(-16.5449852593692,19.9577708609899,0.652214362140303));
#55270=CARTESIAN_POINT('Ctrl Pts',(-16.544803981033,19.9594459793856,0.648339654550236));
#55271=CARTESIAN_POINT('Ctrl Pts',(-16.5446170815428,19.9611465644699,0.644484539592544));
#55272=CARTESIAN_POINT('Ctrl Pts',(-16.5442687863734,19.964315677287,0.637300368487396));
#55273=CARTESIAN_POINT('Ctrl Pts',(-16.5439009460353,19.9675739823819,0.630180634746881));
#55274=CARTESIAN_POINT('Ctrl Pts',(-16.5435149788688,19.9709216245128,0.623118586715854));
#55275=CARTESIAN_POINT('Ctrl Pts',(-16.5427600892517,19.9774690733777,0.609306358121234));
#55276=CARTESIAN_POINT('Ctrl Pts',(-16.5419362971708,19.9843543605266,0.595724100296492));
#55277=CARTESIAN_POINT('Ctrl Pts',(-16.5410553222413,19.9915632524549,0.582361623576685));
#55278=CARTESIAN_POINT('Ctrl Pts',(-16.5405520145231,19.9956817475735,0.574727538381498));
#55279=CARTESIAN_POINT('Ctrl Pts',(-16.5400299818145,19.9999054727865,0.567165025052416));
#55280=CARTESIAN_POINT('Ctrl Pts',(-16.53949136959,20.0042328969111,0.559672683798894));
#55281=CARTESIAN_POINT('Ctrl Pts',(-16.5371210098482,20.0232773067176,0.52669990065196));
#55282=CARTESIAN_POINT('Ctrl Pts',(-16.5344328843906,20.0443209958337,0.495080232313346));
#55283=CARTESIAN_POINT('Ctrl Pts',(-16.5315967308495,20.0672336806369,0.464716909039771));
#55284=CARTESIAN_POINT('Ctrl Pts',(-16.530887911956,20.0729600786099,0.457128428058937));
#55285=CARTESIAN_POINT('Ctrl Pts',(-16.5301697840599,20.078803778894,0.449618679050732));
#55286=CARTESIAN_POINT('Ctrl Pts',(-16.5294449711324,20.0847640692831,0.4421867484608));
#55287=CARTESIAN_POINT('Ctrl Pts',(-16.5283543136099,20.093732777349,0.431003599406807));
#55288=CARTESIAN_POINT('Ctrl Pts',(-16.5272486400087,20.1029648268381,0.419996611718037));
#55289=CARTESIAN_POINT('Ctrl Pts',(-16.5261366293535,20.1124571205592,0.409163249025999));
#55290=CARTESIAN_POINT('Ctrl Pts',(-16.5254006736455,20.1187393515012,0.401993466009371));
#55291=CARTESIAN_POINT('Ctrl Pts',(-16.5246619587109,20.125135694536,0.394899784876159));
#55292=CARTESIAN_POINT('Ctrl Pts',(-16.5239230422738,20.1316458538301,0.38788173218008));
#55293=CARTESIAN_POINT('Ctrl Pts',(-16.5237234984912,20.1334039170503,0.385986512759983));
#55294=CARTESIAN_POINT('Ctrl Pts',(-16.523523911521,20.1351705286926,0.384096538884203));
#55295=CARTESIAN_POINT('Ctrl Pts',(-16.5233243509668,20.1369455085955,0.382211994691331));
#55296=CARTESIAN_POINT('Ctrl Pts',(-16.5225961332083,20.1434225996812,0.375335091819148));
#55297=CARTESIAN_POINT('Ctrl Pts',(-16.5218693863997,20.1500018836066,0.368541134605226));
#55298=CARTESIAN_POINT('Ctrl Pts',(-16.5211497942102,20.1566507251102,0.361858850291119));
#55299=CARTESIAN_POINT('Ctrl Pts',(-16.5209355163636,20.1586305957379,0.359869021170887));
#55300=CARTESIAN_POINT('Ctrl Pts',(-16.5207217743018,20.1606175258447,0.35788820461828));
#55301=CARTESIAN_POINT('Ctrl Pts',(-16.5205086998133,20.1626108208916,0.355917009055417));
#55302=CARTESIAN_POINT('Ctrl Pts',(-16.5198101338809,20.1691458501336,0.349454433098762));
#55303=CARTESIAN_POINT('Ctrl Pts',(-16.5191179110668,20.1757563528476,0.343086927086753));
#55304=CARTESIAN_POINT('Ctrl Pts',(-16.5184344300571,20.1824373565126,0.336815925899807));
#55305=CARTESIAN_POINT('Ctrl Pts',(-16.5154181393187,20.2119214960751,0.309141180687308));
#55306=CARTESIAN_POINT('Ctrl Pts',(-16.5125720762524,20.2427958934596,0.283311277070422));
#55307=CARTESIAN_POINT('Ctrl Pts',(-16.510055328672,20.2749501941091,0.259165979639789));
#55308=CARTESIAN_POINT('Ctrl Pts',(-16.5095951431617,20.2808295851809,0.254751029127042));
#55309=CARTESIAN_POINT('Ctrl Pts',(-16.5091458580602,20.2867518129195,0.2503924601709));
#55310=CARTESIAN_POINT('Ctrl Pts',(-16.5087084339304,20.29271673787,0.246089778989223));
#55311=CARTESIAN_POINT('Ctrl Pts',(-16.5061295101034,20.3278841784264,0.220722438084665));
#55312=CARTESIAN_POINT('Ctrl Pts',(-16.5039651443336,20.3645429559342,0.197285361633269));
#55313=CARTESIAN_POINT('Ctrl Pts',(-16.5023990236787,20.4025977542277,0.17571235928992));
#55314=CARTESIAN_POINT('Ctrl Pts',(-16.5022467391559,20.4062980801142,0.173614670099621));
#55315=CARTESIAN_POINT('Ctrl Pts',(-16.502100105633,20.4100136575059,0.17153383559746));
#55316=CARTESIAN_POINT('Ctrl Pts',(-16.5019593154156,20.4137424636006,0.169470743535446));
#55317=CARTESIAN_POINT('Ctrl Pts',(-16.5015621400589,20.4242615885576,0.163650670662964));
#55318=CARTESIAN_POINT('Ctrl Pts',(-16.501210954272,20.4348995025215,0.157964972318453));
#55319=CARTESIAN_POINT('Ctrl Pts',(-16.5009103026471,20.4456137584343,0.152432928451714));
#55320=CARTESIAN_POINT('Ctrl Pts',(-16.5006642210316,20.454383314908,0.147904982554238));
#55321=CARTESIAN_POINT('Ctrl Pts',(-16.5004519129355,20.463205509022,0.143479117894903));
#55322=CARTESIAN_POINT('Ctrl Pts',(-16.5002757006572,20.4720708611006,0.139160004757658));
#55323=CARTESIAN_POINT('Ctrl Pts',(-16.500236624574,20.4740368037643,0.138202216650574));
#55324=CARTESIAN_POINT('Ctrl Pts',(-16.5001992951787,20.4760053545502,0.137249370747565));
#55325=CARTESIAN_POINT('Ctrl Pts',(-16.5001637279027,20.4779766555572,0.136301387950723));
#55326=CARTESIAN_POINT('Ctrl Pts',(-16.499771814489,20.4996982882644,0.12585562951363));
#55327=CARTESIAN_POINT('Ctrl Pts',(-16.4995946736473,20.5217097527716,0.11602140670495));
#55328=CARTESIAN_POINT('Ctrl Pts',(-16.499654466181,20.5440037453176,0.106782473437692));
#55329=CARTESIAN_POINT('Ctrl Pts',(-28.4921884404488,20.1587841073205,4.48858136870839));
#55330=CARTESIAN_POINT('Ctrl Pts',(-28.4940712295089,20.5,4.37432217737224));
#55331=CARTESIAN_POINT('Ctrl Pts',(-28.5000000000009,20.5,4.01452801010852));
#55332=CARTESIAN_POINT('Ctrl Pts',(-24.4459493854662,20.1555956263289,4.42297449836793));
#55333=CARTESIAN_POINT('Ctrl Pts',(-24.43798817446,20.5,4.31004373441984));
#55334=CARTESIAN_POINT('Ctrl Pts',(-24.4537608788502,20.5,3.94785315837506));
#55335=CARTESIAN_POINT('Ctrl Pts',(-20.3997065615446,20.152598599004,4.35749244459499));
#55336=CARTESIAN_POINT('Ctrl Pts',(-20.392720406832,20.5,4.24601800956522));
#55337=CARTESIAN_POINT('Ctrl Pts',(-20.4075180616586,20.5,3.8814026561495));
#55338=CARTESIAN_POINT('Ctrl Pts',(-16.353460662545,20.1497621460669,4.29211722911022));
#55339=CARTESIAN_POINT('Ctrl Pts',(-16.3552611303492,20.5,4.18217914609945));
#55340=CARTESIAN_POINT('Ctrl Pts',(-16.3612722214407,20.5,3.81513685304315));
#55341=CARTESIAN_POINT('Ctrl Pts',(-16.6268429955203,20.5,3.81948640102502));
#55342=CARTESIAN_POINT('Ctrl Pts',(-20.5845651132323,20.5,3.88431036677466));
#55343=CARTESIAN_POINT('Ctrl Pts',(-24.5422843246593,20.5,3.94931186830211));
#55344=CARTESIAN_POINT('Ctrl Pts',(-28.5,20.5,4.01452801010866));
#55345=CARTESIAN_POINT('Ctrl Pts',(-17.2867685703854,20.1504190344619,4.30719696626493));
#55346=CARTESIAN_POINT('Ctrl Pts',(-17.2686590325533,20.1588563948581,4.30423831313666));
#55347=CARTESIAN_POINT('Ctrl Pts',(-17.2506684453864,20.1671804561454,4.30107402084104));
#55348=CARTESIAN_POINT('Ctrl Pts',(-17.1042449506796,20.2339840890514,4.27363942811962));
#55349=CARTESIAN_POINT('Ctrl Pts',(-16.9731490285154,20.2896863690097,4.23809161586893));
#55350=CARTESIAN_POINT('Ctrl Pts',(-16.6906483986079,20.399246275303,4.13270660898505));
#55351=CARTESIAN_POINT('Ctrl Pts',(-16.5477523533627,20.4474978177044,4.05836797170915));
#55352=CARTESIAN_POINT('Ctrl Pts',(-16.431123175528,20.4751899387349,3.97184757185369));
#55353=CARTESIAN_POINT('Origin',(-28.5,20.,4.01452801010857));
#55354=CARTESIAN_POINT('Ctrl Pts',(-28.4921884534997,21.8412135273285,4.48858057664302));
#55355=CARTESIAN_POINT('Ctrl Pts',(-28.4940712607011,21.5,4.37432028438836));
#55356=CARTESIAN_POINT('Ctrl Pts',(-28.5,21.5,4.01452801010865));
#55357=CARTESIAN_POINT('Ctrl Pts',(-28.5254209870357,21.8411873349216,4.48911941663496));
#55358=CARTESIAN_POINT('Ctrl Pts',(-28.5146908680549,21.5001969822507,4.37470508095403));
#55359=CARTESIAN_POINT('Ctrl Pts',(-28.5166162662214,21.5,4.01507562146144));
#55360=CARTESIAN_POINT('Ctrl Pts',(-28.5583612383751,21.8397714826907,4.48918675379326));
#55361=CARTESIAN_POINT('Ctrl Pts',(-28.535159969218,21.499164542665,4.37488527730213));
#55362=CARTESIAN_POINT('Ctrl Pts',(-28.5330863925031,21.4991738788987,4.01506355035577));
#55363=CARTESIAN_POINT('Ctrl Pts',(-28.6236777750892,21.8342637186865,4.48842670530818));
#55364=CARTESIAN_POINT('Ctrl Pts',(-28.5755649619896,21.4947581941247,4.37486259947081));
#55365=CARTESIAN_POINT('Ctrl Pts',(-28.5657446607293,21.495930348264,4.01397708967205));
#55366=CARTESIAN_POINT('Ctrl Pts',(-28.6560542665336,21.8301715190968,4.48759926621887));
#55367=CARTESIAN_POINT('Ctrl Pts',(-28.5955312938426,21.4913781502374,4.37465937506852));
#55368=CARTESIAN_POINT('Ctrl Pts',(-28.5819329064879,21.4935127684286,4.01290263291554));
#55369=CARTESIAN_POINT('Ctrl Pts',(-28.7202499315746,21.8193320805794,4.48509841768535));
#55370=CARTESIAN_POINT('Ctrl Pts',(-28.6347751662465,21.4823684641649,4.37391749566476));
#55371=CARTESIAN_POINT('Ctrl Pts',(-28.6140307390665,21.4870983928484,4.00974907485253));
#55372=CARTESIAN_POINT('Ctrl Pts',(-28.7520691233355,21.8125849450047,4.48342495569087));
#55373=CARTESIAN_POINT('Ctrl Pts',(-28.6540799499148,21.47672616809,4.37337748925145));
#55374=CARTESIAN_POINT('Ctrl Pts',(-28.6299403346358,21.4831016592162,4.00766990484807));
#55375=CARTESIAN_POINT('Ctrl Pts',(-28.7993731038122,21.8004300668428,4.4803184744276));
#55376=CARTESIAN_POINT('Ctrl Pts',(-28.6823709564734,21.4666385444995,4.37236633380816));
#55377=CARTESIAN_POINT('Ctrl Pts',(-28.6535923252973,21.4758963369637,4.00384291003086));
#55378=CARTESIAN_POINT('Ctrl Pts',(-28.8151137135972,21.7960246635793,4.47917993735541));
#55379=CARTESIAN_POINT('Ctrl Pts',(-28.6917346273236,21.4629852312693,4.37199383821505));
#55380=CARTESIAN_POINT('Ctrl Pts',(-28.6614626302949,21.4732841092092,4.00244472483011));
#55381=CARTESIAN_POINT('Ctrl Pts',(-28.8461585861444,21.7866115397394,4.47673486071072));
#55382=CARTESIAN_POINT('Ctrl Pts',(-28.7100601376562,21.4552142843188,4.37119916143592));
#55383=CARTESIAN_POINT('Ctrl Pts',(-28.6769850660762,21.4677010962118,3.99944965879431));
#55384=CARTESIAN_POINT('Ctrl Pts',(-28.8614762447451,21.7816027460074,4.47542812825129));
#55385=CARTESIAN_POINT('Ctrl Pts',(-28.7190324938991,21.4510933302668,4.37077668089638));
#55386=CARTESIAN_POINT('Ctrl Pts',(-28.6846438958177,21.4647296831086,3.99785250652423));
#55387=CARTESIAN_POINT('Ctrl Pts',(-28.9068305655355,21.7656885765681,4.47127862320908));
#55388=CARTESIAN_POINT('Ctrl Pts',(-28.7454005836816,21.4380588957433,4.36945208065789));
#55389=CARTESIAN_POINT('Ctrl Pts',(-28.7073210556279,21.4552869055806,3.99278981369038));
#55390=CARTESIAN_POINT('Ctrl Pts',(-28.9362700223319,21.7538976633587,4.46820672183587));
#55391=CARTESIAN_POINT('Ctrl Pts',(-28.7621839351622,21.4284950526857,4.36849519695348));
#55392=CARTESIAN_POINT('Ctrl Pts',(-28.7220407844993,21.4482883513904,3.9890532279118));
#55393=CARTESIAN_POINT('Ctrl Pts',(-28.9936013918011,21.7279957199606,4.46156954348255));
#55394=CARTESIAN_POINT('Ctrl Pts',(-28.7941394198094,21.4078545566988,4.36653621615206));
#55395=CARTESIAN_POINT('Ctrl Pts',(-28.7507064690675,21.4329097161546,3.98099696960699));
#55396=CARTESIAN_POINT('Ctrl Pts',(-29.0214932534172,21.7138846523769,4.45800409484777));
#55397=CARTESIAN_POINT('Ctrl Pts',(-28.809316572376,21.3967577837743,4.36553299161296));
#55398=CARTESIAN_POINT('Ctrl Pts',(-28.7646523995967,21.4245296160374,3.9766770804571));
#55399=CARTESIAN_POINT('Ctrl Pts',(-29.062169897947,21.6909554930138,4.45237100283138));
#55400=CARTESIAN_POINT('Ctrl Pts',(-28.8307957370868,21.3791608345931,4.36406993139224));
#55401=CARTESIAN_POINT('Ctrl Pts',(-28.7849907224046,21.4109097954778,3.96986112065059));
#55402=CARTESIAN_POINT('Ctrl Pts',(-29.075534899249,21.6830181207054,4.45044580430147));
#55403=CARTESIAN_POINT('Ctrl Pts',(-28.8377611399515,21.3731163751088,4.36358768640991));
#55404=CARTESIAN_POINT('Ctrl Pts',(-28.7916732225539,21.4061945771178,3.96753309139709));
#55405=CARTESIAN_POINT('Ctrl Pts',(-29.0952881820098,21.6706624712522,4.44749745570096));
#55406=CARTESIAN_POINT('Ctrl Pts',(-28.8478828377938,21.3638285391936,4.36288328557115));
#55407=CARTESIAN_POINT('Ctrl Pts',(-28.8015498644154,21.3988539896752,3.96396973058805));
#55408=CARTESIAN_POINT('Ctrl Pts',(-29.1018282853599,21.6664655673196,4.44650380913622));
#55409=CARTESIAN_POINT('Ctrl Pts',(-28.8512095441988,21.3606882699083,4.36265113339823));
#55410=CARTESIAN_POINT('Ctrl Pts',(-28.8048199161347,21.3963604667832,3.9627691229626));
#55411=CARTESIAN_POINT('Ctrl Pts',(-29.1147425825927,21.6579651097018,4.44450864515904));
#55412=CARTESIAN_POINT('Ctrl Pts',(-28.8577231856397,21.3543668875625,4.3621966351092));
#55413=CARTESIAN_POINT('Ctrl Pts',(-28.8112770643419,21.3913098390223,3.96035897683085));
#55414=CARTESIAN_POINT('Ctrl Pts',(-29.1211247277383,21.6536567486803,4.44350596775694));
#55415=CARTESIAN_POINT('Ctrl Pts',(-28.8609140856392,21.351181922773,4.36197401207208));
#55416=CARTESIAN_POINT('Ctrl Pts',(-28.8144681372952,21.3887498797035,3.95914803253197));
#55417=CARTESIAN_POINT('Ctrl Pts',(-29.1526652448549,21.631827005439,4.43847235110778));
#55418=CARTESIAN_POINT('Ctrl Pts',(-28.8765929641311,21.3350979442923,4.36088339644741));
#55419=CARTESIAN_POINT('Ctrl Pts',(-28.8302383949739,21.3757784666252,3.95307020188013));
#55420=CARTESIAN_POINT('Ctrl Pts',(-29.1767159566876,21.6134440801678,4.43438108172183));
#55421=CARTESIAN_POINT('Ctrl Pts',(-28.8880537416351,21.3219144059112,4.3600980840368));
#55422=CARTESIAN_POINT('Ctrl Pts',(-28.8422637517799,21.3648535306115,3.94813437198529));
#55423=CARTESIAN_POINT('Ctrl Pts',(-29.2225270660648,21.574871526052,4.4261971800743));
#55424=CARTESIAN_POINT('Ctrl Pts',(-28.9090374964588,21.2951002599166,4.358748713827));
#55425=CARTESIAN_POINT('Ctrl Pts',(-28.8651693060966,21.3419268232634,3.9382670253751));
#55426=CARTESIAN_POINT('Ctrl Pts',(-29.2442873168817,21.5546818289773,4.4221043148659));
#55427=CARTESIAN_POINT('Ctrl Pts',(-28.9185449045375,21.2814642482843,4.35818647001453));
#55428=CARTESIAN_POINT('Ctrl Pts',(-28.8760494312548,21.3299250141018,3.93333521783471));
#55429=CARTESIAN_POINT('Ctrl Pts',(-29.2855172252132,21.5124704374293,4.4140388236016));
#55430=CARTESIAN_POINT('Ctrl Pts',(-28.9357479492706,21.2539523862257,4.35731088088201));
#55431=CARTESIAN_POINT('Ctrl Pts',(-28.8966643862929,21.3048295496241,3.92362069657755));
#55432=CARTESIAN_POINT('Ctrl Pts',(-29.3049871100764,21.4904489712157,4.410065963496));
#55433=CARTESIAN_POINT('Ctrl Pts',(-28.9434266252406,21.240076656282,4.35699977222348));
#55434=CARTESIAN_POINT('Ctrl Pts',(-28.9063993271011,21.2917360294249,3.91883768812767));
#55435=CARTESIAN_POINT('Ctrl Pts',(-29.3415625002293,21.4444902677988,4.402363670954));
#55436=CARTESIAN_POINT('Ctrl Pts',(-28.9571107238047,21.2122497699259,4.35662455375813));
#55437=CARTESIAN_POINT('Ctrl Pts',(-28.924687024552,21.2644073658392,3.90956767582023));
#55438=CARTESIAN_POINT('Ctrl Pts',(-29.3583797183681,21.4209125841129,4.39869552597858));
#55439=CARTESIAN_POINT('Ctrl Pts',(-28.9629914489214,21.1985271478654,4.35656529392032));
#55440=CARTESIAN_POINT('Ctrl Pts',(-28.9330956328352,21.250386023388,3.90515441115447));
#55441=CARTESIAN_POINT('Ctrl Pts',(-29.3891180653537,21.3726539763336,4.39183005163618));
#55442=CARTESIAN_POINT('Ctrl Pts',(-28.973161148024,21.1715660793365,4.35664406229473));
#55443=CARTESIAN_POINT('Ctrl Pts',(-28.9484648055261,21.2216851508184,3.89689615360288));
#55444=CARTESIAN_POINT('Ctrl Pts',(-29.4030479090076,21.3479616794509,4.38863064158663));
#55445=CARTESIAN_POINT('Ctrl Pts',(-28.9774363028591,21.1583373942717,4.35678323811578));
#55446=CARTESIAN_POINT('Ctrl Pts',(-28.9554297274226,21.2069988583241,3.89304864813538));
#55447=CARTESIAN_POINT('Ctrl Pts',(-29.4280377101348,21.2974429815817,4.38278815283631));
#55448=CARTESIAN_POINT('Ctrl Pts',(-28.9846847835139,21.132352936126,4.35718155517005));
#55449=CARTESIAN_POINT('Ctrl Pts',(-28.9679246286489,21.1769500095266,3.88602375231856));
#55450=CARTESIAN_POINT('Ctrl Pts',(-29.4390978280929,21.2716166629097,4.38014489699121));
#55451=CARTESIAN_POINT('Ctrl Pts',(-28.9876452414535,21.1196164947342,4.35744097622522));
#55452=CARTESIAN_POINT('Ctrl Pts',(-28.9734546861524,21.1615875015985,3.88284613948955));
#55453=CARTESIAN_POINT('Ctrl Pts',(-29.4534759095429,21.2319956842511,4.37666552971888));
#55454=CARTESIAN_POINT('Ctrl Pts',(-28.9912930054326,21.100819367134,4.35785159131797));
#55455=CARTESIAN_POINT('Ctrl Pts',(-28.9806437285937,21.1380183730222,3.87866382554668));
#55456=CARTESIAN_POINT('Ctrl Pts',(-29.4578992249067,21.2186415082209,4.37558668943266));
#55457=CARTESIAN_POINT('Ctrl Pts',(-28.9923770229233,21.0945950001855,4.35799224521163));
#55458=CARTESIAN_POINT('Ctrl Pts',(-28.9828553849103,21.1300742769095,3.87736710403448));
#55459=CARTESIAN_POINT('Ctrl Pts',(-29.465987969714,21.191630150372,4.37360293094838));
#55460=CARTESIAN_POINT('Ctrl Pts',(-28.9943073102353,21.0822177995094,4.35826908963608));
#55461=CARTESIAN_POINT('Ctrl Pts',(-28.9868997589003,21.1140055482561,3.87498282025292));
#55462=CARTESIAN_POINT('Ctrl Pts',(-29.4696192822395,21.1780858893991,4.37270640575372));
#55463=CARTESIAN_POINT('Ctrl Pts',(-28.9951445909393,21.0761195371597,4.35840399173927));
#55464=CARTESIAN_POINT('Ctrl Pts',(-28.9887154148245,21.1059480903675,3.87390533985094));
#55465=CARTESIAN_POINT('Ctrl Pts',(-29.4792870650363,21.13738000291,4.37030959268363));
#55466=CARTESIAN_POINT('Ctrl Pts',(-28.9973268947821,21.0580347058315,4.35878246091283));
#55467=CARTESIAN_POINT('Ctrl Pts',(-28.993549304859,21.0817318899304,3.87102485145596));
#55468=CARTESIAN_POINT('Ctrl Pts',(-29.4841057550382,21.1101273328488,4.36910072638058));
#55469=CARTESIAN_POINT('Ctrl Pts',(-28.9983395250804,21.0463040140866,4.35899767552963));
#55470=CARTESIAN_POINT('Ctrl Pts',(-28.9959586508823,21.0655186484503,3.86957217090424));
#55471=CARTESIAN_POINT('Ctrl Pts',(-29.490550264767,21.0553939291526,4.3674802440335));
#55472=CARTESIAN_POINT('Ctrl Pts',(-28.9996760790639,21.0230971570783,4.3592939950583));
#55473=CARTESIAN_POINT('Ctrl Pts',(-28.9991809055205,21.0329560350085,3.86762489270201));
#55474=CARTESIAN_POINT('Ctrl Pts',(-29.4921760097455,21.0279131927772,4.36706858867408));
#55475=CARTESIAN_POINT('Ctrl Pts',(-28.9999974971213,21.0116434845654,4.35937439790459));
#55476=CARTESIAN_POINT('Ctrl Pts',(-28.9999937774283,21.0166066609195,3.86713024612489));
#55477=CARTESIAN_POINT('Ctrl Pts',(-29.4921945688699,20.9865184618008,4.36706389944914));
#55478=CARTESIAN_POINT('Ctrl Pts',(-29.0000012300241,20.9943763875203,4.35937529589598));
#55479=CARTESIAN_POINT('Ctrl Pts',(-29.0000030580324,20.9919793004215,3.86712461212284));
#55480=CARTESIAN_POINT('Ctrl Pts',(-29.491796693937,20.9726912328558,4.36716447751106));
#55481=CARTESIAN_POINT('Ctrl Pts',(-28.9999215676363,20.988610264623,4.3593559292573));
#55482=CARTESIAN_POINT('Ctrl Pts',(-28.9998041196641,20.9837529354893,3.86724546797549));
#55483=CARTESIAN_POINT('Ctrl Pts',(-29.4905838324028,20.9519061373972,4.36747053318267));
#55484=CARTESIAN_POINT('Ctrl Pts',(-28.999675702201,20.9799035943349,4.35929796339857));
#55485=CARTESIAN_POINT('Ctrl Pts',(-28.9991976897288,20.9713871033612,3.86761323505766));
#55486=CARTESIAN_POINT('Ctrl Pts',(-29.4900768240666,20.9449703938439,4.36759841750078));
#55487=CARTESIAN_POINT('Ctrl Pts',(-28.9995726548501,20.9769928752733,4.35927385175331));
#55488=CARTESIAN_POINT('Ctrl Pts',(-28.9989441849534,20.9672607767751,3.86776690539778));
#55489=CARTESIAN_POINT('Ctrl Pts',(-29.4888550894157,20.9310839796645,4.36790625998637));
#55490=CARTESIAN_POINT('Ctrl Pts',(-28.9993226236041,20.9711468188149,4.35921639130902));
#55491=CARTESIAN_POINT('Ctrl Pts',(-28.998333318288,20.958999264393,3.86813682365838));
#55492=CARTESIAN_POINT('Ctrl Pts',(-29.4881390288598,20.9241230577317,4.36808655417366));
#55493=CARTESIAN_POINT('Ctrl Pts',(-28.9991753960847,20.9682075011393,4.359182987778));
#55494=CARTESIAN_POINT('Ctrl Pts',(-28.9979752880381,20.954857979854,3.86835347509526));
#55495=CARTESIAN_POINT('Ctrl Pts',(-29.4840537217879,20.8894481005333,4.36911380624685));
#55496=CARTESIAN_POINT('Ctrl Pts',(-28.9983287272948,20.9535160550957,4.35899529685436));
#55497=CARTESIAN_POINT('Ctrl Pts',(-28.9959326327119,20.9342287640144,3.86958788758089));
#55498=CARTESIAN_POINT('Ctrl Pts',(-29.4791760262202,20.8620847319681,4.3703372687358));
#55499=CARTESIAN_POINT('Ctrl Pts',(-28.9973025839744,20.9417309609864,4.35877783659216));
#55500=CARTESIAN_POINT('Ctrl Pts',(-28.99349378694,20.9179496726881,3.87105811205627));
#55501=CARTESIAN_POINT('Ctrl Pts',(-29.4663175094312,20.8080808536016,4.37352482341733));
#55502=CARTESIAN_POINT('Ctrl Pts',(-28.994401313152,20.9177541238724,4.35827550035249));
#55503=CARTESIAN_POINT('Ctrl Pts',(-28.9870645273859,20.8858224184757,3.87488891416135));
#55504=CARTESIAN_POINT('Ctrl Pts',(-29.4583363712703,20.781440422373,4.3754890345634));
#55505=CARTESIAN_POINT('Ctrl Pts',(-28.9925312984857,20.9055848597636,4.35799165813907));
#55506=CARTESIAN_POINT('Ctrl Pts',(-28.9830739586739,20.8699743012662,3.87724964182235));
#55507=CARTESIAN_POINT('Ctrl Pts',(-29.4392907133724,20.7288730680683,4.38009852314833));
#55508=CARTESIAN_POINT('Ctrl Pts',(-28.9876955597396,20.8806200036176,4.35744597641831));
#55509=CARTESIAN_POINT('Ctrl Pts',(-28.9735511301478,20.838703815867,3.88279039442718));
#55510=CARTESIAN_POINT('Ctrl Pts',(-29.4282263471482,20.7029461219291,4.38274392128853));
#55511=CARTESIAN_POINT('Ctrl Pts',(-28.9847392481334,20.8678470649529,4.35718476315632));
#55512=CARTESIAN_POINT('Ctrl Pts',(-28.9680189458604,20.8232814341429,3.88597056971191));
#55513=CARTESIAN_POINT('Ctrl Pts',(-29.4092629849526,20.6645986868852,4.38717765262327));
#55514=CARTESIAN_POINT('Ctrl Pts',(-28.9792302173559,20.8480911023819,4.35688171049857));
#55515=CARTESIAN_POINT('Ctrl Pts',(-28.9585372662084,20.8004721277644,3.89130160193992));
#55516=CARTESIAN_POINT('Ctrl Pts',(-29.4025397457092,20.6518998355629,4.38873461288905));
#55517=CARTESIAN_POINT('Ctrl Pts',(-28.9772187361615,20.841423256124,4.35679578954984));
#55518=CARTESIAN_POINT('Ctrl Pts',(-28.9551756466686,20.792918985876,3.89317381761125));
#55519=CARTESIAN_POINT('Ctrl Pts',(-29.3884503169696,20.6269598359164,4.39195827974487));
#55520=CARTESIAN_POINT('Ctrl Pts',(-28.9728478403863,20.8280481355966,4.3566663867452));
#55521=CARTESIAN_POINT('Ctrl Pts',(-28.9481309311711,20.7780854122449,3.89705062175834));
#55522=CARTESIAN_POINT('Ctrl Pts',(-29.3810676023746,20.6146832373181,4.39362888709889));
#55523=CARTESIAN_POINT('Ctrl Pts',(-28.9704856627442,20.8213250082211,4.35662245897598));
#55524=CARTESIAN_POINT('Ctrl Pts',(-28.9444395747976,20.7707838933009,3.89905990688947));
#55525=CARTESIAN_POINT('Ctrl Pts',(-29.3579234151702,20.5784203361143,4.39879588786272));
#55526=CARTESIAN_POINT('Ctrl Pts',(-28.962834961066,20.8010908203,4.35656590199818));
#55527=CARTESIAN_POINT('Ctrl Pts',(-28.9328674801151,20.7492172623072,3.90527514970604));
#55528=CARTESIAN_POINT('Ctrl Pts',(-29.3411684295824,20.554999545547,4.40244744076628));
#55529=CARTESIAN_POINT('Ctrl Pts',(-28.9569650458199,20.7874431803912,4.35662793190136));
#55530=CARTESIAN_POINT('Ctrl Pts',(-28.9244899880314,20.7352892524624,3.90966848618537));
#55531=CARTESIAN_POINT('Ctrl Pts',(-29.3050389928751,20.509631383246,4.41005424644623));
#55532=CARTESIAN_POINT('Ctrl Pts',(-28.9434428600321,20.7599671800727,4.35699994410375));
#55533=CARTESIAN_POINT('Ctrl Pts',(-28.9064252696976,20.7083117589753,3.91882359624169));
#55534=CARTESIAN_POINT('Ctrl Pts',(-29.2856645850222,20.4876840236708,4.41400971484573));
#55535=CARTESIAN_POINT('Ctrl Pts',(-28.9358090310734,20.7461480282885,4.35730790601429));
#55536=CARTESIAN_POINT('Ctrl Pts',(-28.8967380651115,20.6952622835462,3.92358563950055));
#55537=CARTESIAN_POINT('Ctrl Pts',(-29.2546003141753,20.4558748807086,4.42008700257675));
#55538=CARTESIAN_POINT('Ctrl Pts',(-28.922820708895,20.7253724543198,4.35796877663784));
#55539=CARTESIAN_POINT('Ctrl Pts',(-28.8812059306627,20.6763511463606,3.93090545440959));
#55540=CARTESIAN_POINT('Ctrl Pts',(-29.2439108547355,20.4454572265231,4.42213679870052));
#55541=CARTESIAN_POINT('Ctrl Pts',(-28.9182525509865,20.7184631598855,4.35822084476127));
#55542=CARTESIAN_POINT('Ctrl Pts',(-28.8758612003024,20.6701579942265,3.93337488161505));
#55543=CARTESIAN_POINT('Ctrl Pts',(-29.2218496639032,20.4249998034319,4.42626941644993));
#55544=CARTESIAN_POINT('Ctrl Pts',(-28.9085864424628,20.704673758766,4.35878899591022));
#55545=CARTESIAN_POINT('Ctrl Pts',(-28.8648306055172,20.6579970468792,3.93835482427701));
#55546=CARTESIAN_POINT('Ctrl Pts',(-29.2105624521793,20.4150385371535,4.42833633785348));
#55547=CARTESIAN_POINT('Ctrl Pts',(-28.9035275473896,20.6978463189018,4.35910263212055));
#55548=CARTESIAN_POINT('Ctrl Pts',(-28.8591869996611,20.652075919572,3.9408461871511));
#55549=CARTESIAN_POINT('Ctrl Pts',(-29.17596044531,20.3859527127987,4.43451242027464));
#55550=CARTESIAN_POINT('Ctrl Pts',(-28.8877003840881,20.6776599163682,4.36012163656125));
#55551=CARTESIAN_POINT('Ctrl Pts',(-28.8418859952628,20.6347879628064,3.94829277941604));
#55552=CARTESIAN_POINT('Ctrl Pts',(-29.1518999346225,20.3676173671137,4.43859827357297));
#55553=CARTESIAN_POINT('Ctrl Pts',(-28.8762195965627,20.6644978369657,4.3609092118001));
#55554=CARTESIAN_POINT('Ctrl Pts',(-28.8298557406079,20.623891349496,3.95322218460065));
#55555=CARTESIAN_POINT('Ctrl Pts',(-29.1018152722641,20.3330053854538,4.44658373092187));
#55556=CARTESIAN_POINT('Ctrl Pts',(-28.8513847136705,20.6390640139852,4.36263702917292));
#55557=CARTESIAN_POINT('Ctrl Pts',(-28.8048134093357,20.6033246767378,3.96286433535749));
#55558=CARTESIAN_POINT('Ctrl Pts',(-29.0757911091889,20.3167288114029,4.45048354811133));
#55559=CARTESIAN_POINT('Ctrl Pts',(-28.8380400572134,20.6267792408873,4.36357636390023));
#55560=CARTESIAN_POINT('Ctrl Pts',(-28.7918013274224,20.5936546558004,3.96757734921668));
#55561=CARTESIAN_POINT('Ctrl Pts',(-29.0352521593023,20.2938681210549,4.45609925522955));
#55562=CARTESIAN_POINT('Ctrl Pts',(-28.8165561798406,20.6091707900662,4.3650399217219));
#55563=CARTESIAN_POINT('Ctrl Pts',(-28.7715318531124,20.5800754935647,3.97437224143204));
#55564=CARTESIAN_POINT('Ctrl Pts',(-29.0214882535223,20.2865074155593,4.45793211239332));
#55565=CARTESIAN_POINT('Ctrl Pts',(-28.8091714143158,20.6034513832319,4.36553535860525));
#55566=CARTESIAN_POINT('Ctrl Pts',(-28.7646498997047,20.5757037147109,3.97659139070366));
#55567=CARTESIAN_POINT('Ctrl Pts',(-28.9934475912048,20.2723129927531,4.46150315485745));
#55568=CARTESIAN_POINT('Ctrl Pts',(-28.7939226308694,20.5923278305027,4.36653127887413));
#55569=CARTESIAN_POINT('Ctrl Pts',(-28.7506295691592,20.5672740749771,3.98091835755158));
#55570=CARTESIAN_POINT('Ctrl Pts',(-28.9791516290983,20.2654706309964,4.46324356194687));
#55571=CARTESIAN_POINT('Ctrl Pts',(-28.7860480544218,20.5869145754601,4.36703250165608));
#55572=CARTESIAN_POINT('Ctrl Pts',(-28.7434815880803,20.5632110844206,3.9830288783974));
#55573=CARTESIAN_POINT('Ctrl Pts',(-28.9355954945563,20.2458084368345,4.46828239715749));
#55574=CARTESIAN_POINT('Ctrl Pts',(-28.7618066384647,20.5712704270414,4.36851780691574));
#55575=CARTESIAN_POINT('Ctrl Pts',(-28.7217035199663,20.5515371684708,3.98914513962966));
#55576=CARTESIAN_POINT('Ctrl Pts',(-28.9060067033566,20.2339995629551,4.47135989471833));
#55577=CARTESIAN_POINT('Ctrl Pts',(-28.744926685415,20.561687181048,4.36947765667699));
#55578=CARTESIAN_POINT('Ctrl Pts',(-28.7069091250645,20.5445280122945,3.99288879390593));
#55579=CARTESIAN_POINT('Ctrl Pts',(-28.8457485283665,20.2129019554985,4.47686103269499));
#55580=CARTESIAN_POINT('Ctrl Pts',(-28.7099310450066,20.5444276147742,4.37123208934274));
#55581=CARTESIAN_POINT('Ctrl Pts',(-28.6767800372973,20.5320096838262,3.99960093357708));
#55582=CARTESIAN_POINT('Ctrl Pts',(-28.8150790711961,20.2036134333842,4.47928478552995));
#55583=CARTESIAN_POINT('Ctrl Pts',(-28.6918007935838,20.5367306237201,4.37202848226936));
#55584=CARTESIAN_POINT('Ctrl Pts',(-28.661445308714,20.5265006375016,4.00256956422312));
#55585=CARTESIAN_POINT('Ctrl Pts',(-28.7526503432492,20.1875566536874,4.48338903627318));
#55586=CARTESIAN_POINT('Ctrl Pts',(-28.6544284801008,20.5233913850482,4.3733658398148));
#55587=CARTESIAN_POINT('Ctrl Pts',(-28.630230945009,20.5169822622779,4.00762555943285));
#55588=CARTESIAN_POINT('Ctrl Pts',(-28.7208911539916,20.1807882220752,4.48506965036132));
#55589=CARTESIAN_POINT('Ctrl Pts',(-28.6351661922031,20.5177318547895,4.3739085857297));
#55590=CARTESIAN_POINT('Ctrl Pts',(-28.6143513499902,20.5129728344691,4.00971307048814));
#55591=CARTESIAN_POINT('Ctrl Pts',(-28.6804858960801,20.1739508495855,4.48664840826309));
#55592=CARTESIAN_POINT('Ctrl Pts',(-28.6104428872724,20.5120427346769,4.37437784801154));
#55593=CARTESIAN_POINT('Ctrl Pts',(-28.5941487213541,20.5089266867687,4.01170353994373));
#55594=CARTESIAN_POINT('Ctrl Pts',(-28.6723694509432,20.1726647303069,4.48693804895347));
#55595=CARTESIAN_POINT('Ctrl Pts',(-28.6054711836597,20.5109751096991,4.37446121623121));
#55596=CARTESIAN_POINT('Ctrl Pts',(-28.5900904986563,20.5081658573795,4.01207067678645));
#55597=CARTESIAN_POINT('Ctrl Pts',(-28.6560648033424,20.1702572399895,4.4874636130762));
#55598=CARTESIAN_POINT('Ctrl Pts',(-28.5954663925238,20.5089814406573,4.37460598400524));
#55599=CARTESIAN_POINT('Ctrl Pts',(-28.5819381749868,20.5067421999854,4.01274126216542));
#55600=CARTESIAN_POINT('Ctrl Pts',(-28.64786409799,20.1691343513156,4.48769983367621));
#55601=CARTESIAN_POINT('Ctrl Pts',(-28.5904251656171,20.5080539749396,4.37466747173636));
#55602=CARTESIAN_POINT('Ctrl Pts',(-28.5778378222945,20.5060784772816,4.01304510036563));
#55603=CARTESIAN_POINT('Ctrl Pts',(-28.6232544580252,20.1660288494912,4.48832318516655));
#55604=CARTESIAN_POINT('Ctrl Pts',(-28.5752783730565,20.5054996163594,4.37481674441907));
#55605=CARTESIAN_POINT('Ctrl Pts',(-28.565533002164,20.5042437954364,4.01385517953166));
#55606=CARTESIAN_POINT('Ctrl Pts',(-28.606854980142,20.1643100524113,4.4886249903596));
#55607=CARTESIAN_POINT('Ctrl Pts',(-28.565150180646,20.5040992890267,4.37486951557626));
#55608=CARTESIAN_POINT('Ctrl Pts',(-28.5573332633662,20.5032296994079,4.01425992288297));
#55609=CARTESIAN_POINT('Ctrl Pts',(-28.5576771166509,20.1601865473193,4.48918952635597));
#55610=CARTESIAN_POINT('Ctrl Pts',(-28.5347358984571,20.5008030232128,4.3748833203254));
#55611=CARTESIAN_POINT('Ctrl Pts',(-28.5327443314856,20.5008014950845,4.01506876078307));
#55612=CARTESIAN_POINT('Ctrl Pts',(-28.5249192895454,20.1588122643254,4.48911128378351));
#55613=CARTESIAN_POINT('Ctrl Pts',(-28.5143793401766,20.4998059891208,4.37469926808766));
#55614=CARTESIAN_POINT('Ctrl Pts',(-28.5163654189693,20.5,4.01506735657853));
#55615=CARTESIAN_POINT('Ctrl Pts',(-28.4921884534997,20.1587864726715,4.48858057664303));
#55616=CARTESIAN_POINT('Ctrl Pts',(-28.4940712607011,20.5,4.37432028438837));
#55617=CARTESIAN_POINT('Ctrl Pts',(-28.5,20.5,4.01452801010866));
#55618=CARTESIAN_POINT('Origin',(-28.5,22.,4.01452801010865));
#55619=CARTESIAN_POINT('Ctrl Pts',(-17.1604382594737,21.8496676025271,4.3051562369529));
#55620=CARTESIAN_POINT('Ctrl Pts',(-17.1622439953065,21.5,4.19493778427511));
#55621=CARTESIAN_POINT('Ctrl Pts',(-17.168249805974,21.5,3.82835528266346));
#55622=CARTESIAN_POINT('Ctrl Pts',(-20.9376911771606,21.8469996121483,4.36619869326066));
#55623=CARTESIAN_POINT('Ctrl Pts',(-20.9317890321398,21.5,4.25454850865233));
#55624=CARTESIAN_POINT('Ctrl Pts',(-20.9455027250583,21.5,3.89023893993915));
#55625=CARTESIAN_POINT('Ctrl Pts',(-24.7149414253597,21.8441900241541,4.42733523082889));
#55626=CARTESIAN_POINT('Ctrl Pts',(-24.7082452246339,21.5,4.3143246996786));
#55627=CARTESIAN_POINT('Ctrl Pts',(-24.7227529733574,21.5,3.9522856706513));
#55628=CARTESIAN_POINT('Ctrl Pts',(-28.4921884534997,21.8412135273285,4.48858057664302));
#55629=CARTESIAN_POINT('Ctrl Pts',(-28.4940712607011,21.5,4.37432028438836));
#55630=CARTESIAN_POINT('Ctrl Pts',(-28.5,21.5,4.01452801010865));
#55631=CARTESIAN_POINT('',(-17.1682498059738,21.5,3.82835528266346));
#55632=CARTESIAN_POINT('Origin',(-17.1682498059739,22.,3.82835528266346));
#55633=CARTESIAN_POINT('Ctrl Pts',(-28.5,21.5,4.01452801010865));
#55634=CARTESIAN_POINT('Ctrl Pts',(-24.7227529733574,21.5,3.9522856706513));
#55635=CARTESIAN_POINT('Ctrl Pts',(-20.9455027250583,21.5,3.89023893993915));
#55636=CARTESIAN_POINT('Ctrl Pts',(-17.168249805974,21.5,3.82835528266346));
#55637=CARTESIAN_POINT('Ctrl Pts',(-16.2025936105234,22.0000000000015,3.11864718944382));
#55638=CARTESIAN_POINT('Ctrl Pts',(-16.2025936105219,21.5,3.11864718944354));
#55639=CARTESIAN_POINT('Ctrl Pts',(-16.6935812956895,21.5,3.21315164973649));
#55640=CARTESIAN_POINT('Ctrl Pts',(-16.1958052905938,21.9952325252242,3.15391517021521));
#55641=CARTESIAN_POINT('Ctrl Pts',(-16.2004968595706,21.5,3.15464482315937));
#55642=CARTESIAN_POINT('Ctrl Pts',(-16.6900632709881,21.5,3.23142922671518));
#55643=CARTESIAN_POINT('Ctrl Pts',(-16.1909736753984,21.9904410335953,3.18921042980328));
#55644=CARTESIAN_POINT('Ctrl Pts',(-16.2003114121254,21.5,3.1903398755215));
#55645=CARTESIAN_POINT('Ctrl Pts',(-16.6875219293389,21.5,3.24972861619305));
#55646=CARTESIAN_POINT('Ctrl Pts',(-16.1850775609935,21.9808091032242,3.25984918716021));
#55647=CARTESIAN_POINT('Ctrl Pts',(-16.2035534038268,21.5,3.26082216812292));
#55648=CARTESIAN_POINT('Ctrl Pts',(-16.6843194194186,21.5,3.28636833461055));
#55649=CARTESIAN_POINT('Ctrl Pts',(-16.184013429373,21.9759686124482,3.29519304000078));
#55650=CARTESIAN_POINT('Ctrl Pts',(-16.2069478202362,21.5,3.2956192570052));
#55651=CARTESIAN_POINT('Ctrl Pts',(-16.683658429449,21.5,3.30470884710496));
#55652=CARTESIAN_POINT('Ctrl Pts',(-16.1856383299933,21.9662403165847,3.36592917468473));
#55653=CARTESIAN_POINT('Ctrl Pts',(-16.2171931046112,21.5,3.36436828037402));
#55654=CARTESIAN_POINT('Ctrl Pts',(-16.6842095997079,21.5,3.34143101656532));
#55655=CARTESIAN_POINT('Ctrl Pts',(-16.1883270541929,21.9613524899569,3.40132143910138));
#55656=CARTESIAN_POINT('Ctrl Pts',(-16.2240124021103,21.5,3.39832915993044));
#55657=CARTESIAN_POINT('Ctrl Pts',(-16.6854215969232,21.5,3.35981266995062));
#55658=CARTESIAN_POINT('Ctrl Pts',(-16.1952611487782,21.9539890215863,3.45444862229374));
#55659=CARTESIAN_POINT('Ctrl Pts',(-16.2368456377949,21.5,3.44879630945697));
#55660=CARTESIAN_POINT('Ctrl Pts',(-16.688687584381,21.5,3.38741695572715));
#55661=CARTESIAN_POINT('Ctrl Pts',(-16.1980673520651,21.9515228743596,3.47221008447614));
#55662=CARTESIAN_POINT('Ctrl Pts',(-16.2415532166551,21.5,3.46552752665128));
#55663=CARTESIAN_POINT('Ctrl Pts',(-16.690023065315,21.5,3.39664756592707));
#55664=CARTESIAN_POINT('Ctrl Pts',(-16.2046004673532,21.9466330695926,3.50737333745249));
#55665=CARTESIAN_POINT('Ctrl Pts',(-16.2517211449691,21.5,3.49845354955799));
#55666=CARTESIAN_POINT('Ctrl Pts',(-16.6931549914451,21.5,3.41492555061629));
#55667=CARTESIAN_POINT('Ctrl Pts',(-16.2083287551219,21.9442051915696,3.52480572265553));
#55668=CARTESIAN_POINT('Ctrl Pts',(-16.2571835066352,21.5,3.51468075299862));
#55669=CARTESIAN_POINT('Ctrl Pts',(-16.6949520176578,21.5,3.42398881019779));
#55670=CARTESIAN_POINT('Ctrl Pts',(-16.2208770992767,21.9369742070162,3.57666299693395));
#55671=CARTESIAN_POINT('Ctrl Pts',(-16.2746405337289,21.5,3.56257355900406));
#55672=CARTESIAN_POINT('Ctrl Pts',(-16.7010254780178,21.5,3.45095493296853));
#55673=CARTESIAN_POINT('Ctrl Pts',(-16.2310567694075,21.9322234484231,3.61064917902866));
#55674=CARTESIAN_POINT('Ctrl Pts',(-16.2877614275171,21.5,3.59367857500056));
#55675=CARTESIAN_POINT('Ctrl Pts',(-16.7059823717865,21.5,3.46863477016759));
#55676=CARTESIAN_POINT('Ctrl Pts',(-16.2550248020928,21.9228769565563,3.67746306648168));
#55677=CARTESIAN_POINT('Ctrl Pts',(-16.3168653669915,21.5,3.65418392042109));
#55678=CARTESIAN_POINT('Ctrl Pts',(-16.7177028394155,21.5,3.50340229096279));
#55679=CARTESIAN_POINT('Ctrl Pts',(-16.2688128936766,21.9182811628345,3.71029083551438));
#55680=CARTESIAN_POINT('Ctrl Pts',(-16.332830368222,21.5,3.68360921264127));
#55681=CARTESIAN_POINT('Ctrl Pts',(-16.7244662683933,21.5,3.5204900220454));
#55682=CARTESIAN_POINT('Ctrl Pts',(-16.2922824275864,21.9115226184388,3.75864368771028));
#55683=CARTESIAN_POINT('Ctrl Pts',(-16.3589982628845,21.5,3.72661747700725));
#55684=CARTESIAN_POINT('Ctrl Pts',(-16.736007563454,21.5,3.54566401900879));
#55685=CARTESIAN_POINT('Ctrl Pts',(-16.3005711842475,21.9092923779025,3.77461286058377));
#55686=CARTESIAN_POINT('Ctrl Pts',(-16.3680638057343,21.5,3.74072812126781));
#55687=CARTESIAN_POINT('Ctrl Pts',(-16.7400878524955,21.5,3.55397892124875));
#55688=CARTESIAN_POINT('Ctrl Pts',(-16.3137228907241,21.9059841503794,3.79833842758307));
#55689=CARTESIAN_POINT('Ctrl Pts',(-16.3822304023763,21.5,3.76161740284943));
#55690=CARTESIAN_POINT('Ctrl Pts',(-16.7465683117126,21.5,3.56633327337009));
#55691=CARTESIAN_POINT('Ctrl Pts',(-16.3182212166037,21.9048890818084,3.80619831559438));
#55692=CARTESIAN_POINT('Ctrl Pts',(-16.3870345783552,21.5,3.76851593328029));
#55693=CARTESIAN_POINT('Ctrl Pts',(-16.7487858382735,21.5,3.57042620530286));
#55694=CARTESIAN_POINT('Ctrl Pts',(-16.3274032276077,21.9027249657743,3.82174713590922));
#55695=CARTESIAN_POINT('Ctrl Pts',(-16.3967694053034,21.5,3.78213337204833));
#55696=CARTESIAN_POINT('Ctrl Pts',(-16.7533142130753,21.5,3.57852323401373));
#55697=CARTESIAN_POINT('Ctrl Pts',(-16.3320928677396,21.9016544021241,3.82944691852646));
#55698=CARTESIAN_POINT('Ctrl Pts',(-16.4017064266611,21.5,3.78886237761036));
#55699=CARTESIAN_POINT('Ctrl Pts',(-16.7556279975421,21.5,3.58253297968588));
#55700=CARTESIAN_POINT('Ctrl Pts',(-16.3560302683597,21.8963596025904,3.86757608216625));
#55701=CARTESIAN_POINT('Ctrl Pts',(-16.4266703272049,21.5,3.82202712471223));
#55702=CARTESIAN_POINT('Ctrl Pts',(-16.7674429297045,21.5,3.60238940882647));
#55703=CARTESIAN_POINT('Ctrl Pts',(-16.3767412732872,21.8923088287891,3.89689945605709));
#55704=CARTESIAN_POINT('Ctrl Pts',(-16.4477938851887,21.5,3.8473985141041));
#55705=CARTESIAN_POINT('Ctrl Pts',(-16.7776799493915,21.5,3.61766088108806));
#55706=CARTESIAN_POINT('Ctrl Pts',(-16.4212547011672,21.8846000679653,3.95321952314127));
#55707=CARTESIAN_POINT('Ctrl Pts',(-16.4922230549556,21.5,3.89577853632942));
#55708=CARTESIAN_POINT('Ctrl Pts',(-16.7997098422747,21.5,3.64698765705913));
#55709=CARTESIAN_POINT('Ctrl Pts',(-16.4450569830293,21.8809420124786,3.98021630120148));
#55710=CARTESIAN_POINT('Ctrl Pts',(-16.5155303766581,21.5,3.91881887619101));
#55711=CARTESIAN_POINT('Ctrl Pts',(-16.8115026386653,21.5,3.66104302080526));
#55712=CARTESIAN_POINT('Ctrl Pts',(-16.4831394704891,21.8757778117398,4.01892896400379));
#55713=CARTESIAN_POINT('Ctrl Pts',(-16.5522429195535,21.5,3.9517142788955));
#55714=CARTESIAN_POINT('Ctrl Pts',(-16.8303901405096,21.5,3.6811893820933));
#55715=CARTESIAN_POINT('Ctrl Pts',(-16.4962310185836,21.87411034819,4.03153544455166));
#55716=CARTESIAN_POINT('Ctrl Pts',(-16.5647486534221,21.5,3.96238401751056));
#55717=CARTESIAN_POINT('Ctrl Pts',(-16.8368861257833,21.5,3.68774838298534));
#55718=CARTESIAN_POINT('Ctrl Pts',(-16.5232304690003,21.8708896855758,4.05613814359352));
#55719=CARTESIAN_POINT('Ctrl Pts',(-16.590350960388,21.5,3.98315775527099));
#55720=CARTESIAN_POINT('Ctrl Pts',(-16.8502894580342,21.5,3.70054483446619));
#55721=CARTESIAN_POINT('Ctrl Pts',(-16.5371840523959,21.8693320923327,4.06816930064024));
#55722=CARTESIAN_POINT('Ctrl Pts',(-16.6034911562703,21.5,3.99329469932326));
#55723=CARTESIAN_POINT('Ctrl Pts',(-16.857219503229,21.5,3.7068004456941));
#55724=CARTESIAN_POINT('Ctrl Pts',(-16.5798092654162,21.8648926734758,4.10291746959841));
#55725=CARTESIAN_POINT('Ctrl Pts',(-16.6433246202798,21.5,4.02248194760078));
#55726=CARTESIAN_POINT('Ctrl Pts',(-16.8783985705853,21.5,3.72486007985719));
#55727=CARTESIAN_POINT('Ctrl Pts',(-16.6093180269739,21.8622318314065,4.12437979135235));
#55728=CARTESIAN_POINT('Ctrl Pts',(-16.6706091197525,21.5,4.04047712969076));
#55729=CARTESIAN_POINT('Ctrl Pts',(-16.8930725009553,21.5,3.73600407557229));
#55730=CARTESIAN_POINT('Ctrl Pts',(-16.6704766461075,21.8575203303899,4.16397285607147));
#55731=CARTESIAN_POINT('Ctrl Pts',(-16.7265858290891,21.5,4.07360970878173));
#55732=CARTESIAN_POINT('Ctrl Pts',(-16.9235088870901,21.5,3.75653378697986));
#55733=CARTESIAN_POINT('Ctrl Pts',(-16.7021265340692,21.8554696437867,4.18210353848355));
#55734=CARTESIAN_POINT('Ctrl Pts',(-16.7553000207359,21.5,4.08877356617264));
#55735=CARTESIAN_POINT('Ctrl Pts',(-16.939271358146,21.5,3.76591947797279));
#55736=CARTESIAN_POINT('Ctrl Pts',(-16.7512338740401,21.8528738488001,4.20676429215578));
#55737=CARTESIAN_POINT('Ctrl Pts',(-16.7995480615473,21.5,4.10943149659409));
#55738=CARTESIAN_POINT('Ctrl Pts',(-16.9637457752419,21.5,3.77865617925544));
#55739=CARTESIAN_POINT('Ctrl Pts',(-16.7678756736467,21.8520887609395,4.21456104764755));
#55740=CARTESIAN_POINT('Ctrl Pts',(-16.8144838835962,21.5,4.11596590227308));
#55741=CARTESIAN_POINT('Ctrl Pts',(-16.9720426664911,21.5,3.78267762181121));
#55742=CARTESIAN_POINT('Ctrl Pts',(-16.7932565263885,21.851035571477,4.22560727704492));
#55743=CARTESIAN_POINT('Ctrl Pts',(-16.8372007595605,21.5,4.12524195165351));
#55744=CARTESIAN_POINT('Ctrl Pts',(-16.9847008585882,21.5,3.78836596354519));
#55745=CARTESIAN_POINT('Ctrl Pts',(-16.801786542946,21.8507052596251,4.22918113595141));
#55746=CARTESIAN_POINT('Ctrl Pts',(-16.844822832901,21.5,4.12824551873968));
#55747=CARTESIAN_POINT('Ctrl Pts',(-16.988955749425,21.5,3.79020474534342));
#55748=CARTESIAN_POINT('Ctrl Pts',(-16.8189881015471,21.8500869595188,4.23610930375404));
#55749=CARTESIAN_POINT('Ctrl Pts',(-16.8601732377462,21.5,4.13407543455927));
#55750=CARTESIAN_POINT('Ctrl Pts',(-16.9975375853533,21.5,3.79376592069795));
#55751=CARTESIAN_POINT('Ctrl Pts',(-16.8276738712233,21.8497985841018,4.23946862537602));
#55752=CARTESIAN_POINT('Ctrl Pts',(-16.867914670736,21.5,4.1369063079806));
#55753=CARTESIAN_POINT('Ctrl Pts',(-17.0018716295893,21.5,3.79549088840137));
#55754=CARTESIAN_POINT('Ctrl Pts',(-16.8711939657873,21.8484725442454,4.25561007104468));
#55755=CARTESIAN_POINT('Ctrl Pts',(-16.9066342732154,21.5,4.15052253339453));
#55756=CARTESIAN_POINT('Ctrl Pts',(-17.0235910074471,21.5,3.80377002509308));
#55757=CARTESIAN_POINT('Ctrl Pts',(-16.9064159264563,21.8477761420408,4.26648696465632));
#55758=CARTESIAN_POINT('Ctrl Pts',(-16.9378678496199,21.5,4.15978704982608));
#55759=CARTESIAN_POINT('Ctrl Pts',(-17.0411805852199,21.5,3.80931813715357));
#55760=CARTESIAN_POINT('Ctrl Pts',(-16.9776436707534,21.8470943053695,4.2843084329609));
#55761=CARTESIAN_POINT('Ctrl Pts',(-17.000858079899,21.5,4.17518084553056));
#55762=CARTESIAN_POINT('Ctrl Pts',(-17.0767734998278,21.5,3.81833625027318));
#55763=CARTESIAN_POINT('Ctrl Pts',(-17.01364953131,21.8471089197294,4.29125260718064));
#55764=CARTESIAN_POINT('Ctrl Pts',(-17.0326487818633,21.5,4.1813198113202));
#55765=CARTESIAN_POINT('Ctrl Pts',(-17.0947768799094,21.5,3.82180603412564));
#55766=CARTESIAN_POINT('Ctrl Pts',(-17.0864469048579,21.8478497977723,4.30119943960749));
#55767=CARTESIAN_POINT('Ctrl Pts',(-17.0968888854338,21.5,4.1904875213887));
#55768=CARTESIAN_POINT('Ctrl Pts',(-17.1311983375874,21.5,3.82666277743901));
#55769=CARTESIAN_POINT('Ctrl Pts',(-17.1232387598336,21.848576004873,4.30420261445776));
#55770=CARTESIAN_POINT('Ctrl Pts',(-17.1293741316385,21.5,4.19351989656681));
#55771=CARTESIAN_POINT('Ctrl Pts',(-17.1496165974329,21.5,3.8280499971787));
#55772=CARTESIAN_POINT('Ctrl Pts',(-17.1604382594748,21.8496676025273,4.3051562369486));
#55773=CARTESIAN_POINT('Ctrl Pts',(-17.1622439953075,21.5,4.19493778427092));
#55774=CARTESIAN_POINT('Ctrl Pts',(-17.1682498059746,21.5,3.82835528265908));
#55775=CARTESIAN_POINT('',(-16.6935812956895,21.5,3.21315164973691));
#55776=CARTESIAN_POINT('Origin',(-16.6935812956894,22.,3.21315164973691));
#55777=CARTESIAN_POINT('Ctrl Pts',(-17.1682498059738,21.5,3.82835528266346));
#55778=CARTESIAN_POINT('Ctrl Pts',(-17.1496163615266,21.5,3.82805000639156));
#55779=CARTESIAN_POINT('Ctrl Pts',(-17.1311983124107,21.5,3.82666291100431));
#55780=CARTESIAN_POINT('Ctrl Pts',(-17.1129875977713,21.5,3.82423447272218));
#55781=CARTESIAN_POINT('Ctrl Pts',(-17.0947768831318,21.5,3.82180603444003));
#55782=CARTESIAN_POINT('Ctrl Pts',(-17.0767734953455,21.5,3.81833624928029));
#55783=CARTESIAN_POINT('Ctrl Pts',(-17.0589770387714,21.5,3.81382719380588));
#55784=CARTESIAN_POINT('Ctrl Pts',(-17.0411805821973,21.5,3.8093181383315));
#55785=CARTESIAN_POINT('Ctrl Pts',(-17.0235910065198,21.5,3.80377002473762));
#55786=CARTESIAN_POINT('Ctrl Pts',(-17.0062155047223,21.5,3.79714671688814));
#55787=CARTESIAN_POINT('Ctrl Pts',(-17.001871629273,21.5,3.79549088992577));
#55788=CARTESIAN_POINT('Ctrl Pts',(-16.9975375843724,21.5,3.79376592229798));
#55789=CARTESIAN_POINT('Ctrl Pts',(-16.9932466670332,21.5,3.79198533387674));
#55790=CARTESIAN_POINT('Ctrl Pts',(-16.9889557496941,21.5,3.79020474545551));
#55791=CARTESIAN_POINT('Ctrl Pts',(-16.9847008623217,21.5,3.7883659651211));
#55792=CARTESIAN_POINT('Ctrl Pts',(-16.9804814700195,21.5,3.78646985358707));
#55793=CARTESIAN_POINT('Ctrl Pts',(-16.9720426854152,21.5,3.78267763051893));
#55794=CARTESIAN_POINT('Ctrl Pts',(-16.9637458137767,21.5,3.7786561987763));
#55795=CARTESIAN_POINT('Ctrl Pts',(-16.9555876582206,21.5,3.77441062361576));
#55796=CARTESIAN_POINT('Ctrl Pts',(-16.9392713471094,21.5,3.76591947329292));
#55797=CARTESIAN_POINT('Ctrl Pts',(-16.9235088867934,21.5,3.75653378679473));
#55798=CARTESIAN_POINT('Ctrl Pts',(-16.9082906937124,21.5,3.74626893113479));
#55799=CARTESIAN_POINT('Ctrl Pts',(-16.8930725006315,21.5,3.73600407547485));
#55800=CARTESIAN_POINT('Ctrl Pts',(-16.8783985701434,21.5,3.72486007947304));
#55801=CARTESIAN_POINT('Ctrl Pts',(-16.8642791914462,21.5,3.71282032480514));
#55802=CARTESIAN_POINT('Ctrl Pts',(-16.8572195020976,21.5,3.70680044747119));
#55803=CARTESIAN_POINT('Ctrl Pts',(-16.8502894552196,21.5,3.70054483670679));
#55804=CARTESIAN_POINT('Ctrl Pts',(-16.8435877906765,21.5,3.69414661001588));
#55805=CARTESIAN_POINT('Ctrl Pts',(-16.8368861261335,21.5,3.68774838332496));
#55806=CARTESIAN_POINT('Ctrl Pts',(-16.8303901666861,21.5,3.68118940941518));
#55807=CARTESIAN_POINT('Ctrl Pts',(-16.8240943181697,21.5,3.67447394733714));
#55808=CARTESIAN_POINT('Ctrl Pts',(-16.8115026211382,21.5,3.66104302317998));
#55809=CARTESIAN_POINT('Ctrl Pts',(-16.7997097982202,21.5,3.6469876915202));
#55810=CARTESIAN_POINT('Ctrl Pts',(-16.7886948737312,21.5,3.63232428633634));
#55811=CARTESIAN_POINT('Ctrl Pts',(-16.7776799492422,21.5,3.61766088115248));
#55812=CARTESIAN_POINT('Ctrl Pts',(-16.767442929528,21.5,3.60238940852384));
#55813=CARTESIAN_POINT('Ctrl Pts',(-16.7579909834741,21.5,3.58650426581163));
#55814=CARTESIAN_POINT('Ctrl Pts',(-16.7556279969606,21.5,3.58253298013358));
#55815=CARTESIAN_POINT('Ctrl Pts',(-16.7533142130046,21.5,3.57852323388594));
#55816=CARTESIAN_POINT('Ctrl Pts',(-16.7510500252507,21.5,3.57447471989511));
#55817=CARTESIAN_POINT('Ctrl Pts',(-16.7487858374968,21.5,3.57042620590428));
#55818=CARTESIAN_POINT('Ctrl Pts',(-16.7465683099919,21.5,3.56633327394474));
#55819=CARTESIAN_POINT('Ctrl Pts',(-16.744408157582,21.5,3.56221515655127));
#55820=CARTESIAN_POINT('Ctrl Pts',(-16.7400878527623,21.5,3.55397892176433));
#55821=CARTESIAN_POINT('Ctrl Pts',(-16.7360075823247,21.5,3.54566405902614));
#55822=CARTESIAN_POINT('Ctrl Pts',(-16.7321604686133,21.5,3.53727271349726));
#55823=CARTESIAN_POINT('Ctrl Pts',(-16.7244662411923,21.5,3.52049002243889));
#55824=CARTESIAN_POINT('Ctrl Pts',(-16.71770275581,21.5,3.50340231839282));
#55825=CARTESIAN_POINT('Ctrl Pts',(-16.7118425636876,21.5,3.4860185443094));
#55826=CARTESIAN_POINT('Ctrl Pts',(-16.7059823715651,21.5,3.46863477022598));
#55827=CARTESIAN_POINT('Ctrl Pts',(-16.7010254779788,21.5,3.45095493277599));
#55828=CARTESIAN_POINT('Ctrl Pts',(-16.6969765036837,21.5,3.43297751795946));
#55829=CARTESIAN_POINT('Ctrl Pts',(-16.6949520165362,21.5,3.4239888105512));
#55830=CARTESIAN_POINT('Ctrl Pts',(-16.6931549913987,21.5,3.41492555032882));
#55831=CARTESIAN_POINT('Ctrl Pts',(-16.6915890273506,21.5,3.40578655844823));
#55832=CARTESIAN_POINT('Ctrl Pts',(-16.6900230633025,21.5,3.39664756656763));
#55833=CARTESIAN_POINT('Ctrl Pts',(-16.6886875818764,21.5,3.38741695570003));
#55834=CARTESIAN_POINT('Ctrl Pts',(-16.6875989202476,21.5,3.37821552733009));
#55835=CARTESIAN_POINT('Ctrl Pts',(-16.6854215969899,21.5,3.3598126705902));
#55836=CARTESIAN_POINT('Ctrl Pts',(-16.6842095211892,21.5,3.341431016089));
#55837=CARTESIAN_POINT('Ctrl Pts',(-16.6839339752301,21.5,3.3230699323332));
#55838=CARTESIAN_POINT('Ctrl Pts',(-16.6836584292711,21.5,3.3047088485774));
#55839=CARTESIAN_POINT('Ctrl Pts',(-16.6843194198805,21.5,3.28636832755855));
#55840=CARTESIAN_POINT('Ctrl Pts',(-16.6859206734574,21.5,3.26804847058621));
#55841=CARTESIAN_POINT('Ctrl Pts',(-16.6875219270342,21.5,3.24972861361384));
#55842=CARTESIAN_POINT('Ctrl Pts',(-16.690063224909,21.5,3.23142940534175));
#55843=CARTESIAN_POINT('Ctrl Pts',(-16.6935812956894,21.5,3.2131516497369));
#55844=CARTESIAN_POINT('Ctrl Pts',(-16.202593610521,22.0000000000008,3.11864718945664));
#55845=CARTESIAN_POINT('Ctrl Pts',(-16.1957184589487,21.9951715430978,3.15436629462203));
#55846=CARTESIAN_POINT('Ctrl Pts',(-16.1859815099194,21.9854654363101,3.2258598790665));
#55847=CARTESIAN_POINT('Ctrl Pts',(-16.1829665819188,21.9707542512648,3.33325881028339));
#55848=CARTESIAN_POINT('Ctrl Pts',(-16.1886594487158,21.9608489185629,3.40496390278775));
#55849=CARTESIAN_POINT('Ctrl Pts',(-16.1947028831469,21.9546309218519,3.44981433014988));
#55850=CARTESIAN_POINT('Ctrl Pts',(-16.1960370051889,21.953385286737,3.45879111255802));
#55851=CARTESIAN_POINT('Ctrl Pts',(-16.198954525102,21.9508943481814,3.47672737206541));
#55852=CARTESIAN_POINT('Ctrl Pts',(-16.2036886600536,21.9471719103735,3.50350885086792));
#55853=CARTESIAN_POINT('Ctrl Pts',(-16.2094820387957,21.943491629387,3.52992662971199));
#55854=CARTESIAN_POINT('Ctrl Pts',(-16.2224555305134,21.9361888154331,3.58228639799885));
#55855=CARTESIAN_POINT('Ctrl Pts',(-16.243443740362,21.926605150889,3.65083327008112));
#55856=CARTESIAN_POINT('Ctrl Pts',(-16.2717387445229,21.9173594545968,3.71687788011058));
#55857=CARTESIAN_POINT('Ctrl Pts',(-16.2917644766302,21.9117030148381,3.7573558784022));
#55858=CARTESIAN_POINT('Ctrl Pts',(-16.2958870189328,21.9105778618014,3.76541137344736));
#55859=CARTESIAN_POINT('Ctrl Pts',(-16.3043697052139,21.9083403604339,3.78144124856931));
#55860=CARTESIAN_POINT('Ctrl Pts',(-16.3087328107494,21.9072272829545,3.78942086022403));
#55861=CARTESIAN_POINT('Ctrl Pts',(-16.322164701551,21.9039128024683,3.81320292616586));
#55862=CARTESIAN_POINT('Ctrl Pts',(-16.3502131607211,21.897428434432,3.85981308323516));
#55863=CARTESIAN_POINT('Ctrl Pts',(-16.4027322179389,21.8873501734346,3.93285235362841));
#55864=CARTESIAN_POINT('Ctrl Pts',(-16.4507908256363,21.8801055090351,3.98642820570205));
#55865=CARTESIAN_POINT('Ctrl Pts',(-16.489139535366,21.8750052615153,4.02476122756083));
#55866=CARTESIAN_POINT('Ctrl Pts',(-16.5023073928949,21.8733608411019,4.03723009232507));
#55867=CARTESIAN_POINT('Ctrl Pts',(-16.5226493863467,21.8709822151684,4.05546028919251));
#55868=CARTESIAN_POINT('Ctrl Pts',(-16.5295361102566,21.8702031867554,4.06146456476965));
#55869=CARTESIAN_POINT('Ctrl Pts',(-16.543474562978,21.8686791236909,4.07328378046564));
#55870=CARTESIAN_POINT('Ctrl Pts',(-16.5786505469972,21.8649629318275,4.10228849368512));
#55871=CARTESIAN_POINT('Ctrl Pts',(-16.6448850977027,21.8591153975305,4.14969206171699));
#55872=CARTESIAN_POINT('Ctrl Pts',(-16.7078023052139,21.8551318036597,4.18517776427292));
#55873=CARTESIAN_POINT('Ctrl Pts',(-16.7565201517863,21.8526184966066,4.20927636685549));
#55874=CARTESIAN_POINT('Ctrl Pts',(-16.7812623913296,21.8514806347264,4.2206953758905));
#55875=CARTESIAN_POINT('Ctrl Pts',(-16.8065901477069,21.8505264209456,4.23115186259816));
#55876=CARTESIAN_POINT('Ctrl Pts',(-16.823607193619,21.849931839782,4.23790608915463));
#55877=CARTESIAN_POINT('Ctrl Pts',(-16.832186504007,21.8496552608978,4.24117617269013));
#55878=CARTESIAN_POINT('Ctrl Pts',(-16.8751402484291,21.8483856367268,4.25688013740921));
#55879=CARTESIAN_POINT('Ctrl Pts',(-16.9446525228319,21.8470617787459,4.27805545503759));
#55880=CARTESIAN_POINT('Ctrl Pts',(-17.051203088172,21.847149288382,4.29835081221195));
#55881=CARTESIAN_POINT('Ctrl Pts',(-17.1237622003836,21.8485913694647,4.30421603447309));
#55882=CARTESIAN_POINT('Ctrl Pts',(-17.1604382594737,21.8496676025262,4.30515623695262));
#55883=CARTESIAN_POINT('Origin',(6.61363325216158E-15,22.,8.67361737988404E-16));
#55884=CARTESIAN_POINT('Origin',(-16.9705627484772,22.,1.));
#55885=CARTESIAN_POINT('Origin',(6.61363325216158E-15,21.5,8.67361737988404E-16));
#55886=CARTESIAN_POINT('Ctrl Pts',(-16.9705627484772,21.5,1.));
#55887=CARTESIAN_POINT('Ctrl Pts',(-16.4714285499925,21.5,0.970588235294119));
#55888=CARTESIAN_POINT('Ctrl Pts',(-16.4714285499925,22.,0.970588235294118));
#55889=CARTESIAN_POINT('Ctrl Pts',(-16.9730924147114,21.5,0.978535066559706));
#55890=CARTESIAN_POINT('Ctrl Pts',(-16.4726248688848,21.4987357550958,0.950286027904117));
#55891=CARTESIAN_POINT('Ctrl Pts',(-16.4738838149159,21.9999999929056,0.928921007848723));
#55892=CARTESIAN_POINT('Ctrl Pts',(-16.9754317317103,21.4986236405249,0.957298789971464));
#55893=CARTESIAN_POINT('Ctrl Pts',(-16.473800294324,21.4962631113247,0.930413747061852));
#55894=CARTESIAN_POINT('Ctrl Pts',(-16.4761543280373,21.9972472802644,0.887697651229367));
#55895=CARTESIAN_POINT('Ctrl Pts',(-16.9797520531917,21.4932235672925,0.915268418547053));
#55896=CARTESIAN_POINT('Ctrl Pts',(-16.4761285834595,21.4890472146769,0.89129077147285));
#55897=CARTESIAN_POINT('Ctrl Pts',(-16.4803475808381,21.9864471353705,0.806109282953636));
#55898=CARTESIAN_POINT('Ctrl Pts',(-16.9817330388163,21.4891995296268,0.894474005556199));
#55899=CARTESIAN_POINT('Ctrl Pts',(-16.477280626014,21.4843014926403,0.872053955068109));
#55900=CARTESIAN_POINT('Ctrl Pts',(-16.4822703025775,21.9783990610965,0.765743657386917));
#55901=CARTESIAN_POINT('Ctrl Pts',(-16.9844503569915,21.4811576965197,0.863617266846394));
#55902=CARTESIAN_POINT('Ctrl Pts',(-16.478997614542,21.4754624026359,0.843578987364932));
#55903=CARTESIAN_POINT('Ctrl Pts',(-16.4849076993345,21.962315392118,0.705845282930559));
#55904=CARTESIAN_POINT('Ctrl Pts',(-16.9853137502372,21.4781418015439,0.853387668521146));
#55905=CARTESIAN_POINT('Ctrl Pts',(-16.4795681715045,21.4722267570588,0.834149063173336));
#55906=CARTESIAN_POINT('Ctrl Pts',(-16.4857456988577,21.9562836046578,0.685987826630035));
#55907=CARTESIAN_POINT('Ctrl Pts',(-16.9865469689091,21.4731031270861,0.83812930879024));
#55908=CARTESIAN_POINT('Ctrl Pts',(-16.4804215368506,21.4669273082589,0.820090807417157));
#55909=CARTESIAN_POINT('Ctrl Pts',(-16.4869426462451,21.9462062533871,0.656368658489502));
#55910=CARTESIAN_POINT('Ctrl Pts',(-16.9869483441066,21.4713344879556,0.833049325850491));
#55911=CARTESIAN_POINT('Ctrl Pts',(-16.4807060704638,21.4650828708149,0.81541110466952));
#55912=CARTESIAN_POINT('Ctrl Pts',(-16.4873322164795,21.9426689751386,0.646507515166357));
#55913=CARTESIAN_POINT('Ctrl Pts',(-16.9877257789808,21.4676473220122,0.822983872627081));
#55914=CARTESIAN_POINT('Ctrl Pts',(-16.4812706985101,21.4612671112103,0.806139057202684));
#55915=CARTESIAN_POINT('Ctrl Pts',(-16.4880867853405,21.935294644797,0.626968693643048));
#55916=CARTESIAN_POINT('Ctrl Pts',(-16.9881022884415,21.4657273940252,0.817993215794496));
#55917=CARTESIAN_POINT('Ctrl Pts',(-16.4815510701315,21.4592943080115,0.801542122223246));
#55918=CARTESIAN_POINT('Ctrl Pts',(-16.4884522212722,21.9314547874519,0.617280948546226));
#55919=CARTESIAN_POINT('Ctrl Pts',(-16.9899262296916,21.4557510501466,0.793247536974804));
#55920=CARTESIAN_POINT('Ctrl Pts',(-16.4829437859584,21.4491049656455,0.778740039448324));
#55921=CARTESIAN_POINT('Ctrl Pts',(-16.4902225165023,21.9115021026871,0.569245217876393));
#55922=CARTESIAN_POINT('Ctrl Pts',(-16.9911982217854,21.4465691378748,0.774112785120951));
#55923=CARTESIAN_POINT('Ctrl Pts',(-16.4840273309326,21.4399290909792,0.761105698710872));
#55924=CARTESIAN_POINT('Ctrl Pts',(-16.4914570981261,21.8931382758739,0.532101288712044));
#55925=CARTESIAN_POINT('Ctrl Pts',(-16.9934231069503,21.4258556925665,0.737138900069214));
#55926=CARTESIAN_POINT('Ctrl Pts',(-16.4861354093574,21.4194806578111,0.726913881060247));
#55927=CARTESIAN_POINT('Ctrl Pts',(-16.4936165444703,21.8517113850087,0.46032845312769));
#55928=CARTESIAN_POINT('Ctrl Pts',(-16.9943758591795,21.414324206792,0.71929973894501));
#55929=CARTESIAN_POINT('Ctrl Pts',(-16.4871593711862,21.408212854135,0.710365087012568));
#55930=CARTESIAN_POINT('Ctrl Pts',(-16.4945412755648,21.8286484158979,0.42569949159161));
#55931=CARTESIAN_POINT('Ctrl Pts',(-16.9953970848308,21.3984014616618,0.697833076923672));
#55932=CARTESIAN_POINT('Ctrl Pts',(-16.4883990487207,21.3927164742621,0.690342539314858));
#55933=CARTESIAN_POINT('Ctrl Pts',(-16.495532464569,21.796802922745,0.384028914441952));
#55934=CARTESIAN_POINT('Ctrl Pts',(-16.9955928310526,21.3951412010012,0.693581520762139));
#55935=CARTESIAN_POINT('Ctrl Pts',(-16.4886448954113,21.389547103093,0.686372439009793));
#55936=CARTESIAN_POINT('Ctrl Pts',(-16.4957224537866,21.7902824027076,0.375775892704089));
#55937=CARTESIAN_POINT('Ctrl Pts',(-16.9959680297371,21.3884670399167,0.685163197758813));
#55938=CARTESIAN_POINT('Ctrl Pts',(-16.4891323578279,21.3830633781607,0.678500451067321));
#55939=CARTESIAN_POINT('Ctrl Pts',(-16.4960866169799,21.7769340791281,0.359434443248347));
#55940=CARTESIAN_POINT('Ctrl Pts',(-16.9961468750295,21.3850634632371,0.681009770694884));
#55941=CARTESIAN_POINT('Ctrl Pts',(-16.4893731970484,21.3797591439209,0.674611100232451));
#55942=CARTESIAN_POINT('Ctrl Pts',(-16.4962602024104,21.7701269259005,0.351371908294615));
#55943=CARTESIAN_POINT('Ctrl Pts',(-16.9966570591121,21.3746901264464,0.668757101822919));
#55944=CARTESIAN_POINT('Ctrl Pts',(-16.4900845285808,21.3696931424689,0.663121500578075));
#55945=CARTESIAN_POINT('Ctrl Pts',(-16.4967553805512,21.7493802540404,0.327587314353041));
#55946=CARTESIAN_POINT('Ctrl Pts',(-16.9969628806611,21.367543746169,0.660847276778648));
#55947=CARTESIAN_POINT('Ctrl Pts',(-16.4905449680627,21.3627634611966,0.655681319541789));
#55948=CARTESIAN_POINT('Ctrl Pts',(-16.4970522080279,21.7350874917574,0.312232949589363));
#55949=CARTESIAN_POINT('Ctrl Pts',(-16.9977909492914,21.3454263958916,0.637877776038412));
#55950=CARTESIAN_POINT('Ctrl Pts',(-16.4918845932564,21.3413163750418,0.634012177598984));
#55951=CARTESIAN_POINT('Ctrl Pts',(-16.4978559207164,21.6908527929444,0.267645093565885));
#55952=CARTESIAN_POINT('Ctrl Pts',(-16.9982241467675,21.3297798973633,0.623575071775558));
#55953=CARTESIAN_POINT('Ctrl Pts',(-16.4927226159692,21.3261385831506,0.620424702005762));
#55954=CARTESIAN_POINT('Ctrl Pts',(-16.4982763783124,21.6595597954117,0.239881020862232));
#55955=CARTESIAN_POINT('Ctrl Pts',(-16.9987417316421,21.3049641718212,0.603629616735995));
#55956=CARTESIAN_POINT('Ctrl Pts',(-16.4938942111891,21.3019902595213,0.601351128009065));
#55957=CARTESIAN_POINT('Ctrl Pts',(-16.4987787392512,21.6099283432998,0.201163374073859));
#55958=CARTESIAN_POINT('Ctrl Pts',(-16.9988921266689,21.2964672601923,0.597233320088741));
#55959=CARTESIAN_POINT('Ctrl Pts',(-16.4942703351611,21.2937134410915,0.59521430533367));
#55960=CARTESIAN_POINT('Ctrl Pts',(-16.4989247114421,21.5929345210954,0.188747032136024));
#55961=CARTESIAN_POINT('Ctrl Pts',(-16.9990895438383,21.2833789662798,0.588023277146211));
#55962=CARTESIAN_POINT('Ctrl Pts',(-16.4948124151445,21.2809410864574,0.58634835836836));
#55963=CARTESIAN_POINT('Ctrl Pts',(-16.499116321829,21.5667579322043,0.170868714949001));
#55964=CARTESIAN_POINT('Ctrl Pts',(-16.9991506486861,21.278959003145,0.585017379496349));
#55965=CARTESIAN_POINT('Ctrl Pts',(-16.4949893919106,21.2766248913159,0.583450140483979));
#55966=CARTESIAN_POINT('Ctrl Pts',(-16.4991756297338,21.5579180067263,0.165033736025826));
#55967=CARTESIAN_POINT('Ctrl Pts',(-16.9992642464521,21.2700032207303,0.579135459380374));
#55968=CARTESIAN_POINT('Ctrl Pts',(-16.4953358105115,21.2678716432874,0.577769744216801));
#55969=CARTESIAN_POINT('Ctrl Pts',(-16.4992858861356,21.5400064410244,0.153615892381932));
#55970=CARTESIAN_POINT('Ctrl Pts',(-16.9993168223211,21.2654589507784,0.576254390691533));
#55971=CARTESIAN_POINT('Ctrl Pts',(-16.495505551458,21.2634263453468,0.574982645018446));
#55972=CARTESIAN_POINT('Ctrl Pts',(-16.4993369159319,21.5309179011113,0.148023229697779));
#55973=CARTESIAN_POINT('Ctrl Pts',(-16.9995587890305,21.2425697250579,0.562255024254108));
#55974=CARTESIAN_POINT('Ctrl Pts',(-16.4963302414363,21.2410229373867,0.561423225150239));
#55975=CARTESIAN_POINT('Ctrl Pts',(-16.4995717652251,21.4851394518979,0.120847985424646));
#55976=CARTESIAN_POINT('Ctrl Pts',(-16.9996864974581,21.2237270718151,0.552343930390703));
#55977=CARTESIAN_POINT('Ctrl Pts',(-16.4969149739077,21.2225074098179,0.551748630561899));
#55978=CARTESIAN_POINT('Ctrl Pts',(-16.4996957185789,21.4474541433703,0.101608806618414));
#55979=CARTESIAN_POINT('Ctrl Pts',(-16.9998646648994,21.1850170081964,0.535007025860517));
#55980=CARTESIAN_POINT('Ctrl Pts',(-16.497937467953,21.1843269944478,0.534747006217183));
#55981=CARTESIAN_POINT('Ctrl Pts',(-16.4998686448857,21.3700340166527,0.0679548143398367));
#55982=CARTESIAN_POINT('Ctrl Pts',(-16.9999149747695,21.1651494999123,0.527581453344155));
#55983=CARTESIAN_POINT('Ctrl Pts',(-16.4983754282979,21.1646605210359,0.527417269072898));
#55984=CARTESIAN_POINT('Ctrl Pts',(-16.4999174758386,21.3302990004269,0.0535404663248945));
#55985=CARTESIAN_POINT('Ctrl Pts',(-16.9999615835097,21.1345695782299,0.518331609142281));
#55986=CARTESIAN_POINT('Ctrl Pts',(-16.4989206599236,21.1342942076196,0.518256449450954));
#55987=CARTESIAN_POINT('Ctrl Pts',(-16.499962713243,21.2691391561586,0.03558488930072));
#55988=CARTESIAN_POINT('Ctrl Pts',(-16.9999722038594,21.1242461095535,0.515564014231725));
#55989=CARTESIAN_POINT('Ctrl Pts',(-16.4990837274006,21.1240294091075,0.515509487574471));
#55990=CARTESIAN_POINT('Ctrl Pts',(-16.4999730215237,21.2484922195051,0.0302124965614095));
#55991=CARTESIAN_POINT('Ctrl Pts',(-16.9999835208626,21.1085607133984,0.511898164807746));
#55992=CARTESIAN_POINT('Ctrl Pts',(-16.4992996622756,21.1084131980924,0.511865629153836));
#55993=CARTESIAN_POINT('Ctrl Pts',(-16.4999840054778,21.2171214265978,0.0230964383945357));
#55994=CARTESIAN_POINT('Ctrl Pts',(-16.9999865105534,21.103306350935,0.510759293490706));
#55995=CARTESIAN_POINT('Ctrl Pts',(-16.4993667326936,21.1031791513432,0.510732629817123));
#55996=CARTESIAN_POINT('Ctrl Pts',(-16.4999869073623,21.2066127017183,0.0208856881011679));
#55997=CARTESIAN_POINT('Ctrl Pts',(-16.9999913085683,21.0928052333294,0.508659120654602));
#55998=CARTESIAN_POINT('Ctrl Pts',(-16.4994903974202,21.0927131482552,0.508641928307854));
#55999=CARTESIAN_POINT('Ctrl Pts',(-16.4999915641382,21.1856104668105,0.0168088805338418));
#56000=CARTESIAN_POINT('Ctrl Pts',(-16.9999931228912,21.0875500018386,0.507695791798136));
#56001=CARTESIAN_POINT('Ctrl Pts',(-16.4995471133876,21.0874726632328,0.507682173326117));
#56002=CARTESIAN_POINT('Ctrl Pts',(-16.4999933252095,21.1751000035788,0.0149388905328434));
#56003=CARTESIAN_POINT('Ctrl Pts',(-17.0000001629822,21.0612507660885,0.503307616912964));
#56004=CARTESIAN_POINT('Ctrl Pts',(-16.4998053929721,21.0612395973646,0.503308608999867));
#56005=CARTESIAN_POINT('Ctrl Pts',(-16.5000001579872,21.1225015325702,0.00642066583814521));
#56006=CARTESIAN_POINT('Ctrl Pts',(-16.9999999168185,21.0401378114417,0.501162938454188));
#56007=CARTESIAN_POINT('Ctrl Pts',(-16.4999315871971,21.0401353257552,0.501162809927001));
#56008=CARTESIAN_POINT('Ctrl Pts',(-16.4999999193109,21.080275622896,0.00225746843716186));
#56009=CARTESIAN_POINT('Ctrl Pts',(-17.0000000528006,20.9977674399885,0.499555723826538));
#56010=CARTESIAN_POINT('Ctrl Pts',(-16.500026133197,20.9977703241831,0.499555867466912));
#56011=CARTESIAN_POINT('Ctrl Pts',(-16.5000000512018,20.9955348799642,-0.000862418127516337));
#56012=CARTESIAN_POINT('Ctrl Pts',(-17.0000004327897,20.9765100308675,0.500093051759841));
#56013=CARTESIAN_POINT('Ctrl Pts',(-16.4999945261161,20.9765031360088,0.500094127563245));
#56014=CARTESIAN_POINT('Ctrl Pts',(-16.5000004199499,20.9530200614576,0.000180626893516891));
#56015=CARTESIAN_POINT('Ctrl Pts',(-16.9999992958654,20.949845179443,0.502493050353376));
#56016=CARTESIAN_POINT('Ctrl Pts',(-16.4998533288364,20.9498593753611,0.50249165881252));
#56017=CARTESIAN_POINT('Ctrl Pts',(-16.4999993166029,20.8996903589554,0.00483945143427439));
#56018=CARTESIAN_POINT('Ctrl Pts',(-16.9999989479835,20.9444988945152,0.503060911828994));
#56019=CARTESIAN_POINT('Ctrl Pts',(-16.4998199145986,20.9445181653914,0.50305883795362));
#56020=CARTESIAN_POINT('Ctrl Pts',(-16.4999989788889,20.888997789137,0.00594177086414229));
#56021=CARTESIAN_POINT('Ctrl Pts',(-16.9999978061467,20.9338399384988,0.504367397839467));
#56022=CARTESIAN_POINT('Ctrl Pts',(-16.4997430304164,20.9338730534644,0.50436305067304));
#56023=CARTESIAN_POINT('Ctrl Pts',(-16.4999978707081,20.8676798768911,0.00847788908051538));
#56024=CARTESIAN_POINT('Ctrl Pts',(-16.9999970135041,20.9285349696757,0.505104749276568));
#56025=CARTESIAN_POINT('Ctrl Pts',(-16.4996996337999,20.9285767396921,0.505098840478412));
#56026=CARTESIAN_POINT('Ctrl Pts',(-16.4999971012969,20.8570699394581,0.00990921985109947));
#56027=CARTESIAN_POINT('Ctrl Pts',(-16.9999935826483,20.9126925582127,0.507565588529774));
#56028=CARTESIAN_POINT('Ctrl Pts',(-16.4995547778939,20.9127662249117,0.507552986668588));
#56029=CARTESIAN_POINT('Ctrl Pts',(-16.4999937714846,20.8253851162119,0.0146861411058046));
#56030=CARTESIAN_POINT('Ctrl Pts',(-16.9999899191601,20.9022275356819,0.509537601288132));
#56031=CARTESIAN_POINT('Ctrl Pts',(-16.4994386694513,20.9023313755917,0.509517878518783));
#56032=CARTESIAN_POINT('Ctrl Pts',(-16.4999902155292,20.8044550715146,0.018514167866819));
#56033=CARTESIAN_POINT('Ctrl Pts',(-16.9999707269349,20.8711168396759,0.516429520854516));
#56034=CARTESIAN_POINT('Ctrl Pts',(-16.4990327235418,20.8713427933764,0.516372901480069));
#56035=CARTESIAN_POINT('Ctrl Pts',(-16.4999715881597,20.7422336790502,0.0318925979849346));
#56036=CARTESIAN_POINT('Ctrl Pts',(-16.9999474621371,20.8507544093414,0.52232143473415));
#56037=CARTESIAN_POINT('Ctrl Pts',(-16.498685458987,20.8511091143981,0.522220449062311));
#56038=CARTESIAN_POINT('Ctrl Pts',(-16.4999490069737,20.7015088182385,0.0433298426955125));
#56039=CARTESIAN_POINT('Ctrl Pts',(-16.999872593906,20.8207774110138,0.533103835838787));
#56040=CARTESIAN_POINT('Ctrl Pts',(-16.49804985819,20.8214264933554,0.532857061552179));
#56041=CARTESIAN_POINT('Ctrl Pts',(-16.4998763413414,20.6415548222497,0.0642603878165643));
#56042=CARTESIAN_POINT('Ctrl Pts',(-16.9998408653516,20.8108798020863,0.537023027180669));
#56043=CARTESIAN_POINT('Ctrl Pts',(-16.4978187255782,20.811640257904,0.536715854407526));
#56044=CARTESIAN_POINT('Ctrl Pts',(-16.4998455455476,20.6217596036359,0.0718682280307113));
#56045=CARTESIAN_POINT('Ctrl Pts',(-16.9997583144814,20.7912774765208,0.545523339639611));
#56046=CARTESIAN_POINT('Ctrl Pts',(-16.4973174053915,20.7922932250178,0.545060273323437));
#56047=CARTESIAN_POINT('Ctrl Pts',(-16.4997654231138,20.5825549535782,0.088368836973362));
#56048=CARTESIAN_POINT('Ctrl Pts',(-16.9997073352247,20.7815527714696,0.550115598300045));
#56049=CARTESIAN_POINT('Ctrl Pts',(-16.4970465330306,20.7827124914974,0.549557176956291));
#56050=CARTESIAN_POINT('Ctrl Pts',(-16.4997159433886,20.5631055157649,0.0972832302481202));
#56051=CARTESIAN_POINT('Ctrl Pts',(-16.9996439954592,20.7720018726588,0.555009152983024));
#56052=CARTESIAN_POINT('Ctrl Pts',(-16.4967580121734,20.7733226724976,0.554332420210074));
#56053=CARTESIAN_POINT('Ctrl Pts',(-16.499654466181,20.5440037453175,0.106782473437634));
#56054=CARTESIAN_POINT('Origin',(-28.5,21.,1.));
#56055=CARTESIAN_POINT('Origin',(-17.5,24.,-29.5));
#56056=CARTESIAN_POINT('Origin',(6.61287431064084E-15,53.,0.));
#56057=CARTESIAN_POINT('',(-15.2695685015073,52.,12.9166666666667));
#56058=CARTESIAN_POINT('Origin',(-15.2695685015073,53.,12.9166666666667));
#56059=CARTESIAN_POINT('',(-15.2695685015073,52.,-12.9166666666666));
#56060=CARTESIAN_POINT('Origin',(-15.2695685015073,53.,-12.9166666666667));
#56061=CARTESIAN_POINT('Origin',(6.61287431064084E-15,52.,0.));
#56062=CARTESIAN_POINT('Origin',(-45.2928932188135,48.4656487624794,-19.0077234952746));
#56063=CARTESIAN_POINT('',(-45.2928932188135,48.0436073736659,-18.7396170497563));
#56064=CARTESIAN_POINT('',(-45.2928932188135,48.7337552079976,-18.5856821064611));
#56065=CARTESIAN_POINT('Origin',(-45.2928932188135,48.4656487624794,-19.0077234952746));
#56066=CARTESIAN_POINT('',(-45.6464466094067,48.6552286481851,-18.7092951673032));
#56067=CARTESIAN_POINT('Origin',(-45.2928932188135,48.4656487624794,-19.0077234952746));
#56068=CARTESIAN_POINT('Origin',(-45.2928932188135,48.4656487624794,-19.0077234952746));
#56069=CARTESIAN_POINT('Origin',(-50.,48.4656487624794,-19.0077234952746));
#56070=CARTESIAN_POINT('',(-50.,48.7337552079976,-18.5856821064611));
#56071=CARTESIAN_POINT('',(-50.,48.0436073736659,-18.7396170497563));
#56072=CARTESIAN_POINT('Origin',(-45.2928932188135,51.4199384841736,-20.884468613902));
#56073=CARTESIAN_POINT('',(-45.2928932188135,51.2660035408783,-20.1943207795704));
#56074=CARTESIAN_POINT('',(-45.6464466094067,51.1874769810659,-20.3179338404124));
#56075=CARTESIAN_POINT('Origin',(-45.2928932188135,50.9978970953601,-20.6163621683838));
#56076=CARTESIAN_POINT('',(-45.6464466094067,51.6095183698793,-20.5860402859306));
#56077=CARTESIAN_POINT('',(-45.2928932188135,48.3117138191841,-18.3175756609429));
#56078=CARTESIAN_POINT('Origin',(-36.5,53.9282032302755,-24.));
#56079=CARTESIAN_POINT('',(-37.,53.9282032302755,-24.));
#56080=CARTESIAN_POINT('',(-36.5,54.4282032302755,-24.));
#56081=CARTESIAN_POINT('Origin',(-36.5,53.9282032302755,-24.));
#56082=CARTESIAN_POINT('',(-36.5,53.9282032302755,-24.5));
#56083=CARTESIAN_POINT('Origin',(-36.5,53.9282032302755,-24.));
#56084=CARTESIAN_POINT('Origin',(-36.5,53.9282032302755,-24.));
#56085=CARTESIAN_POINT('Origin',(-36.5,53.9282032302755,0.));
#56086=CARTESIAN_POINT('',(-37.,53.9282032302755,-17.5));
#56087=CARTESIAN_POINT('',(-36.5,54.4282032302755,-17.5));
#56088=CARTESIAN_POINT('Origin',(-36.5,53.9282032302755,-17.5));
#56089=CARTESIAN_POINT('',(-36.5,54.4282032302755,-17.));
#56090=CARTESIAN_POINT('',(-37.,53.9282032302755,-24.5));
#56091=CARTESIAN_POINT('Origin',(-37.,53.9282032302755,-24.));
#56092=CARTESIAN_POINT('',(-6.78091634720693,53.9282032302755,-24.5));
#56093=CARTESIAN_POINT('',(-7.20387088797839,54.4282032302755,-24.));
#56094=CARTESIAN_POINT('Origin',(-7.20387088797737,53.9282032302767,-24.0000000000012));
#56095=CARTESIAN_POINT('',(-37.,53.9282032302755,-24.5));
#56096=CARTESIAN_POINT('',(-37.,54.4282032302755,-24.));
#56097=CARTESIAN_POINT('Origin',(-36.5,53.9282032302755,-17.5));
#56098=CARTESIAN_POINT('',(-36.5,53.9282032302755,-17.));
#56099=CARTESIAN_POINT('Origin',(-36.5,53.9282032302755,-17.5));
#56100=CARTESIAN_POINT('Origin',(-36.5,53.9282032302755,-17.5));
#56101=CARTESIAN_POINT('Origin',(-36.5,3.36766747301154E-16,-17.5));
#56102=CARTESIAN_POINT('',(-37.,45.4641016151378,-17.5));
#56103=CARTESIAN_POINT('',(-36.5,45.4641016151378,-17.));
#56104=CARTESIAN_POINT('Origin',(-36.5,45.4641016151378,-17.5));
#56105=CARTESIAN_POINT('',(-36.5,44.9641016151378,-17.));
#56106=CARTESIAN_POINT('',(-37.,54.4282032302755,-17.5));
#56107=CARTESIAN_POINT('Origin',(-37.,53.9282032302755,-17.5));
#56108=CARTESIAN_POINT('',(-12.7022799180074,54.4282032302755,-17.5));
#56109=CARTESIAN_POINT('',(-13.1252344587788,53.9282032302755,-17.));
#56110=CARTESIAN_POINT('Origin',(-12.702279918008,53.9282032302763,-17.4999999999992));
#56111=CARTESIAN_POINT('',(-37.,54.4282032302755,-17.5));
#56112=CARTESIAN_POINT('',(-37.,53.9282032302755,-17.));
#56113=CARTESIAN_POINT('Origin',(-36.5,45.4641016151378,-17.5));
#56114=CARTESIAN_POINT('',(-36.5,44.9641016151378,-17.5));
#56115=CARTESIAN_POINT('Origin',(-36.5,45.4641016151378,-17.5));
#56116=CARTESIAN_POINT('Origin',(-36.5,45.4641016151378,-17.5));
#56117=CARTESIAN_POINT('Origin',(-36.5,45.4641016151375,6.30941155087793E-13));
#56118=CARTESIAN_POINT('',(-36.5,44.9641016151378,-23.5872397343813));
#56119=CARTESIAN_POINT('',(-37.,45.4641016151378,-22.800161699018));
#56120=CARTESIAN_POINT('Origin',(-36.5000000000005,45.4641016151372,-22.8001616990189));
#56121=CARTESIAN_POINT('',(-36.5,44.9641016151378,-23.5872397343815));
#56122=CARTESIAN_POINT('',(-37.,45.4641016151378,-17.));
#56123=CARTESIAN_POINT('Origin',(-6.5,41.0779586111866,-36.2318935544818));
#56124=CARTESIAN_POINT('',(-6.5,49.1231323076242,-24.5));
#56125=CARTESIAN_POINT('',(-6.5,41.5,-36.5));
#56126=CARTESIAN_POINT('',(-6.,48.8484038560691,-24.));
#56127=CARTESIAN_POINT('Origin',(-6.49999999999975,48.8484038560692,-24.0000000000003));
#56128=CARTESIAN_POINT('',(-6.,45.6658960598572,-29.0097639675421));
#56129=CARTESIAN_POINT('Origin',(-6.5,38.813816723824,-34.2012134925591));
#56130=CARTESIAN_POINT('',(-6.,38.813816723824,-34.2012134925591));
#56131=CARTESIAN_POINT('',(-6.5,38.5457102783057,-34.6232548813726));
#56132=CARTESIAN_POINT('Origin',(-6.5,38.813816723824,-34.2012134925591));
#56133=CARTESIAN_POINT('',(-6.5,38.3917753350105,-33.9331070470409));
#56134=CARTESIAN_POINT('Origin',(-6.5,38.813816723824,-34.2012134925591));
#56135=CARTESIAN_POINT('Origin',(-6.5,38.813816723824,-34.2012134925591));
#56136=CARTESIAN_POINT('Origin',(-6.5,41.7681064455182,-36.0779586111866));
#56137=CARTESIAN_POINT('',(-6.5,41.5,-36.5));
#56138=CARTESIAN_POINT('',(-6.,-4.31983100315249,-6.80008819812621));
#56139=CARTESIAN_POINT('Origin',(-45.2928932188134,41.7681064455182,-36.0779586111866));
#56140=CARTESIAN_POINT('',(-45.2928932188134,38.5457102783057,-34.6232548813726));
#56141=CARTESIAN_POINT('',(-45.6464466094067,38.6242368381183,-34.4996418205305));
#56142=CARTESIAN_POINT('Origin',(-45.2928932188135,38.813816723824,-34.2012134925591));
#56143=CARTESIAN_POINT('',(-45.6464466094067,38.2021954493047,-34.2315353750123));
#56144=CARTESIAN_POINT('Origin',(-45.2928932188134,41.3460650567048,-35.8098521656684));
#56145=CARTESIAN_POINT('',(-45.2928932188134,41.5,-36.5));
#56146=CARTESIAN_POINT('Origin',(-45.2928932188135,38.813816723824,-34.2012134925591));
#56147=CARTESIAN_POINT('',(-45.2928932188135,38.3917753350105,-33.9331070470409));
#56148=CARTESIAN_POINT('Origin',(-45.2928932188134,38.813816723824,-34.2012134925591));
#56149=CARTESIAN_POINT('Origin',(-45.2928932188135,38.813816723824,-34.2012134925591));
#56150=CARTESIAN_POINT('Origin',(-50.,38.813816723824,-34.2012134925591));
#56151=CARTESIAN_POINT('',(-50.,38.3917753350105,-33.9331070470409));
#56152=CARTESIAN_POINT('',(-50.,38.5457102783057,-34.6232548813726));
#56153=CARTESIAN_POINT('Origin',(-47.3964466094067,39.9417691688435,-32.4256403037406));
#56154=CARTESIAN_POINT('',(-49.5,40.6476802250494,-30.3819606694039));
#56155=CARTESIAN_POINT('',(-45.1464466094067,38.313248775198,-34.056720107883));
#56156=CARTESIAN_POINT('',(-49.8535533905933,40.8801417281571,-30.9484954428935));
#56157=CARTESIAN_POINT('Origin',(-49.5,41.0697216138629,-30.6500671149221));
#56158=CARTESIAN_POINT('',(-50.,40.9586682879697,-30.8248823820514));
#56159=CARTESIAN_POINT('Origin',(-49.5,-2.06392611311356,-3.24894182048922));
#56160=CARTESIAN_POINT('',(-50.,41.0697216138629,-30.6500671149221));
#56161=CARTESIAN_POINT('Origin',(-49.5,41.0697216138629,-30.6500671149221));
#56162=CARTESIAN_POINT('',(-50.,-2.06392611311356,-3.24894182048923));
#56163=CARTESIAN_POINT('',(-49.8535533905933,-2.2535059988193,-3.54737014846061));
#56164=CARTESIAN_POINT('Origin',(-49.5,41.0697216138629,-30.6500671149221));
#56165=CARTESIAN_POINT('Origin',(-49.5,41.0697216138629,-30.6500671149221));
#56166=CARTESIAN_POINT('Origin',(-49.5,43.1336477269765,-27.4011252944329));
#56167=CARTESIAN_POINT('',(-50.,43.1035198521152,-27.4485512715437));
#56168=CARTESIAN_POINT('',(-49.5,40.5366268991562,-30.5567759365332));
#56169=CARTESIAN_POINT('Origin',(-6.5,38.5457102783057,-34.6232548813726));
#56170=CARTESIAN_POINT('',(-6.,40.2323075626015,-31.9682875274271));
#56171=CARTESIAN_POINT('',(-6.,43.1336477269765,-27.4011252944329));
#56172=CARTESIAN_POINT('',(-6.5,39.7323075626015,-31.8229001029736));
#56173=CARTESIAN_POINT('Origin',(-6.5000000000006,40.2323075626021,-31.9682875274273));
#56174=CARTESIAN_POINT('',(-6.5,38.1236688894923,-34.3551484358543));
#56175=CARTESIAN_POINT('Origin',(-45.2928932188135,41.3460650567048,-35.8098521656684));
#56176=CARTESIAN_POINT('Origin',(-49.5,45.6658960598572,-29.0097639675421));
#56177=CARTESIAN_POINT('',(-50.,48.7419922053212,-24.1675085460208));
#56178=CARTESIAN_POINT('',(-50.,46.7081939670689,-27.3690243893992));
#56179=CARTESIAN_POINT('',(-49.5,49.1640335941347,-24.435614991539));
#56180=CARTESIAN_POINT('Origin',(-49.5,48.7419922053212,-24.1675085460208));
#56181=CARTESIAN_POINT('',(-49.5,49.275086920028,-24.2607997244097));
#56182=CARTESIAN_POINT('Origin',(-49.5,48.7419922053212,-24.1675085460208));
#56183=CARTESIAN_POINT('',(-49.8535533905933,48.931572091027,-23.8690802180494));
#56184=CARTESIAN_POINT('Origin',(-49.5,48.7419922053212,-24.1675085460208));
#56185=CARTESIAN_POINT('Origin',(-49.5,48.7419922053212,-24.1675085460208));
#56186=CARTESIAN_POINT('Origin',(-56.8964466094067,44.7759221854948,-30.4107217446581));
#56187=CARTESIAN_POINT('',(-45.2928932188135,51.4199384841736,-20.884468613902));
#56188=CARTESIAN_POINT('Origin',(-45.2928932188135,50.9978970953601,-20.6163621683838));
#56189=CARTESIAN_POINT('',(-45.1464466094067,51.4984650439861,-20.7608555530599));
#56190=CARTESIAN_POINT('',(-50.,48.8530455312145,-23.9926932788915));
#56191=CARTESIAN_POINT('Origin',(-56.8964466094067,42.243673852614,-28.8020830715488));
#56192=CARTESIAN_POINT('',(-45.5,48.7337552079976,-18.5856821064611));
#56193=CARTESIAN_POINT('',(-49.6464466094067,45.7091759238145,-22.4143764882355));
#56194=CARTESIAN_POINT('Origin',(-49.5,3.07609614546394,4.8422554215213));
#56195=CARTESIAN_POINT('',(-50.,3.07609614546394,4.84225542152131));
#56196=CARTESIAN_POINT('',(-49.8535533905933,3.26567603116969,5.14068374949269));
#56197=CARTESIAN_POINT('Origin',(-49.5,43.1336477269765,-27.4011252944329));
#56198=CARTESIAN_POINT('',(-50.,44.1759456341881,-25.7603857162899));
#56199=CARTESIAN_POINT('',(-50.,46.3207971983337,-22.3840546057823));
#56200=CARTESIAN_POINT('',(-49.5,44.0220106908928,-25.0702378819582));
#56201=CARTESIAN_POINT('Origin',(-49.5000000000009,44.444052079705,-25.3383443274766));
#56202=CARTESIAN_POINT('',(-49.5,43.7539042453746,-25.4922792707717));
#56203=CARTESIAN_POINT('Origin',(-37.,54.4282032302755,-17.));
#56204=CARTESIAN_POINT('',(-4.19913133791448,54.4282032302755,-27.5520833333334));
#56205=CARTESIAN_POINT('Origin',(-37.,3.67381906146713E-16,0.));
#56206=CARTESIAN_POINT('',(-37.,51.5341099863965,-19.7722793907569));
#56207=CARTESIAN_POINT('',(-37.,5.86821392653928,9.23748457678522));
#56208=CARTESIAN_POINT('',(-37.,38.1236688894923,-34.3551484358543));
#56209=CARTESIAN_POINT('',(-37.,50.0331217848147,-24.));
#56210=CARTESIAN_POINT('',(-37.,49.1231323076242,-24.));
#56211=CARTESIAN_POINT('',(-37.,51.8419798729871,-21.1525750594202));
#56212=CARTESIAN_POINT('',(-37.,46.5099788374842,-29.5459768585786));
#56213=CARTESIAN_POINT('Origin',(-37.,50.9978970953601,-20.6163621683838));
#56214=CARTESIAN_POINT('Origin',(-37.,44.9641016151378,-24.5));
#56215=CARTESIAN_POINT('',(-10.,44.9641016151378,-23.5872397343813));
#56216=CARTESIAN_POINT('',(-10.,44.9641016151378,-17.5));
#56217=CARTESIAN_POINT('',(-10.,44.9641016151375,6.24002261183886E-13));
#56218=CARTESIAN_POINT('',(-37.,44.9641016151378,-17.5));
#56219=CARTESIAN_POINT('',(-50.,44.9641016151378,-23.5872397343813));
#56220=CARTESIAN_POINT('Origin',(-37.,44.9641016151378,-17.));
#56221=CARTESIAN_POINT('',(-10.,45.4641016151378,-17.));
#56222=CARTESIAN_POINT('',(-10.,51.,-17.));
#56223=CARTESIAN_POINT('',(-10.,3.67381906146713E-16,-17.));
#56224=CARTESIAN_POINT('',(-11.,52.,-17.));
#56225=CARTESIAN_POINT('Origin',(-11.,51.,-17.));
#56226=CARTESIAN_POINT('',(-11.8154397518737,52.,-17.));
#56227=CARTESIAN_POINT('',(6.61363325216158E-15,52.,-17.));
#56228=CARTESIAN_POINT('',(-13.1252344587788,53.,-17.));
#56229=CARTESIAN_POINT('Origin',(-11.8154397518729,53.0000000000004,-17.));
#56230=CARTESIAN_POINT('',(-13.1252344587788,57.,-17.));
#56231=CARTESIAN_POINT('',(-37.,45.4641016151378,-17.));
#56232=CARTESIAN_POINT('Origin',(33.,25.8967919448979,4.98934246731003));
#56233=CARTESIAN_POINT('',(15.863798335516,26.6272203612273,4.67630172554642));
#56234=CARTESIAN_POINT('Origin',(16.7453756123118,26.2781107809041,4.82592044071226));
#56235=CARTESIAN_POINT('',(16.0339930597927,26.2575776988747,4.83472006237606));
#56236=CARTESIAN_POINT('Origin',(16.8887635278285,26.8426106081843,4.58399492666055));
#56237=CARTESIAN_POINT('',(33.,26.2575776350368,4.83472002867911));
#56238=CARTESIAN_POINT('',(33.,26.2575776350368,4.83472002867911));
#56239=CARTESIAN_POINT('',(33.,25.8967919448979,4.98934246731003));
#56240=CARTESIAN_POINT('Origin',(0.5,48.5249973351313,-4.97500266486866));
#56241=CARTESIAN_POINT('',(5.4811647369232,19.0972134699726,-33.7896016253977));
#56242=CARTESIAN_POINT('Ctrl Pts',(5.47974928497604,19.0969304167095,-33.767306956549));
#56243=CARTESIAN_POINT('Ctrl Pts',(5.48022993085033,19.0970264611248,-33.7747404391871));
#56244=CARTESIAN_POINT('Ctrl Pts',(5.48070183516169,19.097120832269,-33.7821735628567));
#56245=CARTESIAN_POINT('Ctrl Pts',(5.4811647369232,19.0972134699726,-33.7896016253977));
#56246=CARTESIAN_POINT('Origin',(0.5,19.4038059222875,-34.0961940777126));
#56247=CARTESIAN_POINT('Origin',(-27.5,24.,-29.5));
#56248=CARTESIAN_POINT('',(-27.5,23.5,-23.));
#56249=CARTESIAN_POINT('',(-27.5,23.5,-29.5));
#56250=CARTESIAN_POINT('',(-27.5,24.5,-23.));
#56251=CARTESIAN_POINT('',(-27.5,23.5,-23.));
#56252=CARTESIAN_POINT('',(-27.5,24.5,-29.5));
#56253=CARTESIAN_POINT('Origin',(4.5,24.,-37.));
#56254=CARTESIAN_POINT('',(0.5,22.3076118445749,-37.));
#56255=CARTESIAN_POINT('',(-2.35233629352793,22.3076118445749,-37.));
#56256=CARTESIAN_POINT('',(0.5,22.3076118445749,-37.));
#56257=CARTESIAN_POINT('Origin',(0.499999999976273,16.5000000000764,-36.9999999999998));
#56258=CARTESIAN_POINT('Origin',(4.5,24.,6.93889390390723E-15));
#56259=CARTESIAN_POINT('Origin',(4.49999999937185,24.0000000020693,-38.6923881574814));
#56260=CARTESIAN_POINT('Origin',(0.5,19.4038059222875,-34.0961940777126));
#56261=CARTESIAN_POINT('Origin',(0.5,19.4038059222875,-34.0961940777126));
#56262=CARTESIAN_POINT('Origin',(9.,24.,-29.5));
#56263=CARTESIAN_POINT('',(9.5,21.9882004875966,-35.152668637192));
#56264=CARTESIAN_POINT('Origin',(9.,21.9882004875966,-35.152668637192));
#56265=CARTESIAN_POINT('',(9.5,21.9882004875966,-23.847331362808));
#56266=CARTESIAN_POINT('Origin',(9.5,24.,-29.5));
#56267=CARTESIAN_POINT('Origin',(9.,21.9882004875966,-23.847331362808));
#56268=CARTESIAN_POINT('Ctrl Pts',(9.5,26.0117995124037,-35.1526686371919));
#56269=CARTESIAN_POINT('Ctrl Pts',(9.50000000000001,26.1794494717706,-35.623724356958));
#56270=CARTESIAN_POINT('Ctrl Pts',(8.99999999999989,26.1794494717706,-35.6237243569579));
#56271=CARTESIAN_POINT('Ctrl Pts',(9.5,25.969126524566,-35.1678560713817));
#56272=CARTESIAN_POINT('Ctrl Pts',(9.50000000000001,26.1363858923875,-35.6200054618018));
#56273=CARTESIAN_POINT('Ctrl Pts',(9.01826917526509,26.1417283486801,-35.6371494030576));
#56274=CARTESIAN_POINT('Ctrl Pts',(9.5,25.9266618092262,-35.1837246773205));
#56275=CARTESIAN_POINT('Ctrl Pts',(9.49999999999997,26.0919477789377,-35.6183024929583));
#56276=CARTESIAN_POINT('Ctrl Pts',(9.03631589192574,26.1032568243223,-35.6504486521462));
#56277=CARTESIAN_POINT('Ctrl Pts',(9.5,25.8420590117766,-35.21653092188));
#56278=CARTESIAN_POINT('Ctrl Pts',(9.50000000000005,26.0025448380055,-35.6183771479464));
#56279=CARTESIAN_POINT('Ctrl Pts',(9.07183836849202,26.0248814931803,-35.6766951383499));
#56280=CARTESIAN_POINT('Ctrl Pts',(9.5,25.7999211590539,-35.2334691645038));
#56281=CARTESIAN_POINT('Ctrl Pts',(9.50000000000001,25.9574863153535,-35.6200467193352));
#56282=CARTESIAN_POINT('Ctrl Pts',(9.08931415962551,25.9849775488743,-35.6896423865758));
#56283=CARTESIAN_POINT('Ctrl Pts',(9.5,25.7158975753409,-35.2681705887087));
#56284=CARTESIAN_POINT('Ctrl Pts',(9.49999999999999,25.8671165675929,-35.6260854809282));
#56285=CARTESIAN_POINT('Ctrl Pts',(9.1235736889288,25.9038137144825,-35.7150866515789));
#56286=CARTESIAN_POINT('Ctrl Pts',(9.5,25.6740028719298,-35.2859382131717));
#56287=CARTESIAN_POINT('Ctrl Pts',(9.5,25.8216976115558,-35.6303888638396));
#56288=CARTESIAN_POINT('Ctrl Pts',(9.14036084384017,25.8625443955667,-35.7275862152158));
#56289=CARTESIAN_POINT('Ctrl Pts',(9.5,25.5904820429837,-35.322051972562));
#56290=CARTESIAN_POINT('Ctrl Pts',(9.5,25.7308556139648,-35.6410699898064));
#56291=CARTESIAN_POINT('Ctrl Pts',(9.17309573545697,25.7788188856162,-35.7520160803084));
#56292=CARTESIAN_POINT('Ctrl Pts',(9.5,25.54884683225,-35.3404019499814));
#56293=CARTESIAN_POINT('Ctrl Pts',(9.50000000000001,25.6853264252681,-35.6474086022825));
#56294=CARTESIAN_POINT('Ctrl Pts',(9.18904735031175,25.7363542059438,-35.7639492338914));
#56295=CARTESIAN_POINT('Ctrl Pts',(9.5,25.4242015033402,-35.3960612434519));
#56296=CARTESIAN_POINT('Ctrl Pts',(9.50000000000001,25.5502828319477,-35.6685604400058));
#56297=CARTESIAN_POINT('Ctrl Pts',(9.23550610480808,25.607279019684,-35.7987774920106));
#56298=CARTESIAN_POINT('Ctrl Pts',(9.5,25.3414487728041,-35.433973095274));
#56299=CARTESIAN_POINT('Ctrl Pts',(9.50000000000009,25.4588206457325,-35.685861865764));
#56300=CARTESIAN_POINT('Ctrl Pts',(9.2646135723705,25.5189820341969,-35.8206987330504));
#56301=CARTESIAN_POINT('Ctrl Pts',(9.5,25.176109276692,-35.5101853172836));
#56302=CARTESIAN_POINT('Ctrl Pts',(9.49999999999992,25.2766858194012,-35.7237734257663));
#56303=CARTESIAN_POINT('Ctrl Pts',(9.31837705316277,25.3386902127447,-35.8613243440875));
#56304=CARTESIAN_POINT('Ctrl Pts',(9.5,25.0935237034198,-35.5484884786143));
#56305=CARTESIAN_POINT('Ctrl Pts',(9.49999999999992,25.1853323050273,-35.7444076007431));
#56306=CARTESIAN_POINT('Ctrl Pts',(9.34303153817123,25.2466967857052,-35.8800272698057));
#56307=CARTESIAN_POINT('Ctrl Pts',(9.5,24.9280807136363,-35.6244584254345));
#56308=CARTESIAN_POINT('Ctrl Pts',(9.50000000000008,25.0033399898978,-35.7867586891882));
#56309=CARTESIAN_POINT('Ctrl Pts',(9.38729861344404,25.0599620838701,-35.9136948179777));
#56310=CARTESIAN_POINT('Ctrl Pts',(9.5,24.8452239160408,-35.6621266597857));
#56311=CARTESIAN_POINT('Ctrl Pts',(9.5,24.9120763623833,-35.8085867314734));
#56312=CARTESIAN_POINT('Ctrl Pts',(9.40691008519286,24.9652233257944,-35.9286583428068));
#56313=CARTESIAN_POINT('Ctrl Pts',(9.5,24.6788556331735,-35.7359305267538));
#56314=CARTESIAN_POINT('Ctrl Pts',(9.5,24.7301341256831,-35.8516195729549));
#56315=CARTESIAN_POINT('Ctrl Pts',(9.44067629739234,24.7740415871847,-35.9544685122108));
#56316=CARTESIAN_POINT('Ctrl Pts',(9.5,24.5953445434688,-35.7720670853785));
#56317=CARTESIAN_POINT('Ctrl Pts',(9.5,24.6388718622012,-35.8729686489815));
#56318=CARTESIAN_POINT('Ctrl Pts',(9.45483075696681,24.6776017522002,-35.9653147728946));
#56319=CARTESIAN_POINT('Ctrl Pts',(9.5,24.4273258947367,-35.8420075016043));
#56320=CARTESIAN_POINT('Ctrl Pts',(9.5,24.4567995163812,-35.913676588705));
#56321=CARTESIAN_POINT('Ctrl Pts',(9.47746628181506,24.4840675352485,-35.9826782942412));
#56322=CARTESIAN_POINT('Ctrl Pts',(9.5,24.3428186889365,-35.875812186098));
#56323=CARTESIAN_POINT('Ctrl Pts',(9.50000000000009,24.365437407906,-35.9331791082525));
#56324=CARTESIAN_POINT('Ctrl Pts',(9.48594808355023,24.3869762064944,-35.9891960450384));
#56325=CARTESIAN_POINT('Ctrl Pts',(9.5,24.2150771332136,-35.9242233171871));
#56326=CARTESIAN_POINT('Ctrl Pts',(9.49999999999996,24.2284532489845,-35.9601253781755));
#56327=CARTESIAN_POINT('Ctrl Pts',(9.49439707925568,24.2415678655432,-35.9956907978406));
#56328=CARTESIAN_POINT('Ctrl Pts',(9.5,24.1723333665474,-35.939978202615));
#56329=CARTESIAN_POINT('Ctrl Pts',(9.50000000000017,24.1827991755656,-35.9687288907579));
#56330=CARTESIAN_POINT('Ctrl Pts',(9.49650254697548,24.1931355198232,-35.9973099740758));
#56331=CARTESIAN_POINT('Ctrl Pts',(9.5,24.1079451005327,-35.9629723458731));
#56332=CARTESIAN_POINT('Ctrl Pts',(9.49999999999993,24.11429879057,-35.9809702182257));
#56333=CARTESIAN_POINT('Ctrl Pts',(9.49860334653214,24.1206206521294,-35.998925697095));
#56334=CARTESIAN_POINT('Ctrl Pts',(9.5,24.0864369182992,-35.9705307174653));
#56335=CARTESIAN_POINT('Ctrl Pts',(9.49999999999993,24.0914619868762,-35.9849404193503));
#56336=CARTESIAN_POINT('Ctrl Pts',(9.49912745052014,24.0964712112024,-35.9993288281094));
#56337=CARTESIAN_POINT('Ctrl Pts',(9.5,24.0541030972586,-35.9817007841272));
#56338=CARTESIAN_POINT('Ctrl Pts',(9.50000000000002,24.0571981105742,-35.9907188498919));
#56339=CARTESIAN_POINT('Ctrl Pts',(9.49965105814884,24.0602891948851,-35.9997315860922));
#56340=CARTESIAN_POINT('Ctrl Pts',(9.5,24.0433132330065,-35.9853962262216));
#56341=CARTESIAN_POINT('Ctrl Pts',(9.49999999999965,24.0457753673003,-35.9926155427435));
#56342=CARTESIAN_POINT('Ctrl Pts',(9.49978183973438,24.0482355396307,-35.9998321856301));
#56343=CARTESIAN_POINT('Ctrl Pts',(9.5,24.021709091742,-35.9927299609635));
#56344=CARTESIAN_POINT('Ctrl Pts',(9.50000000000013,24.0229268751936,-35.9963480615538));
#56345=CARTESIAN_POINT('Ctrl Pts',(9.49995621937517,24.0241436645304,-35.9999663224548));
#56346=CARTESIAN_POINT('Ctrl Pts',(9.5,24.0109082581165,-35.9963507604577));
#56347=CARTESIAN_POINT('Ctrl Pts',(9.5,24.0115165090366,-35.998175025983));
#56348=CARTESIAN_POINT('Ctrl Pts',(9.5,24.0121234081387,-36.0000000002211));
#56349=CARTESIAN_POINT('Ctrl Pts',(9.5,24.,-36.));
#56350=CARTESIAN_POINT('Ctrl Pts',(9.5,24.,-36.));
#56351=CARTESIAN_POINT('Ctrl Pts',(9.5,24.,-36.));
#56352=CARTESIAN_POINT('Ctrl Pts',(9.5,24.,-36.));
#56353=CARTESIAN_POINT('Ctrl Pts',(9.5,24.0054150064504,-35.9981884682733));
#56354=CARTESIAN_POINT('Ctrl Pts',(9.49999999999458,24.0108043085154,-35.9963861629621));
#56355=CARTESIAN_POINT('Ctrl Pts',(9.49999999999452,24.0161950807351,-35.994574350307));
#56356=CARTESIAN_POINT('Ctrl Pts',(9.49999999999445,24.0215858529548,-35.9927625376518));
#56357=CARTESIAN_POINT('Ctrl Pts',(9.5,24.0269887853828,-35.9909375873191));
#56358=CARTESIAN_POINT('Ctrl Pts',(9.5,24.0323884057965,-35.9891047955571));
#56359=CARTESIAN_POINT('Ctrl Pts',(9.5,24.0431876466238,-35.9854392120329));
#56360=CARTESIAN_POINT('Ctrl Pts',(9.5,24.0539746311336,-35.9817449034163));
#56361=CARTESIAN_POINT('Ctrl Pts',(9.5,24.0647497302229,-35.9780227911426));
#56362=CARTESIAN_POINT('Ctrl Pts',(9.5,24.0862999284017,-35.9705785665953));
#56363=CARTESIAN_POINT('Ctrl Pts',(9.5,24.1078024533637,-35.9630227406302));
#56364=CARTESIAN_POINT('Ctrl Pts',(9.5,24.1292595640221,-35.9553606016205));
#56365=CARTESIAN_POINT('Ctrl Pts',(9.5,24.1721737853388,-35.9400363236011));
#56366=CARTESIAN_POINT('Ctrl Pts',(9.5,24.214906343328,-35.9242867765023));
#56367=CARTESIAN_POINT('Ctrl Pts',(9.5,24.2574757167881,-35.9081552208262));
#56368=CARTESIAN_POINT('Ctrl Pts',(9.5,24.3426144637084,-35.8758921094742));
#56369=CARTESIAN_POINT('Ctrl Pts',(9.5,24.4270996255911,-35.8420989822636));
#56370=CARTESIAN_POINT('Ctrl Pts',(9.5,24.511087024606,-35.8071406043763));
#56371=CARTESIAN_POINT('Ctrl Pts',(9.5,24.5950744236209,-35.7721822264891));
#56372=CARTESIAN_POINT('Ctrl Pts',(9.5,24.6785636988575,-35.7360577521598));
#56373=CARTESIAN_POINT('Ctrl Pts',(9.5,24.7617259798232,-35.6991678002813));
#56374=CARTESIAN_POINT('Ctrl Pts',(9.5,24.8448882607888,-35.6622778484028));
#56375=CARTESIAN_POINT('Ctrl Pts',(9.5,24.927723145438,-35.6246214737663));
#56376=CARTESIAN_POINT('Ctrl Pts',(9.5,25.0104224970507,-35.586647819507));
#56377=CARTESIAN_POINT('Ctrl Pts',(9.5,25.0931218486634,-35.5486741652478));
#56378=CARTESIAN_POINT('Ctrl Pts',(9.5,25.1756850333398,-35.510381750864));
#56379=CARTESIAN_POINT('Ctrl Pts',(9.5,25.2583319332265,-35.4722853085716));
#56380=CARTESIAN_POINT('Ctrl Pts',(9.5,25.3409788331131,-35.4341888662792));
#56381=CARTESIAN_POINT('Ctrl Pts',(9.5,25.4237082318775,-35.396285553944));
#56382=CARTESIAN_POINT('Ctrl Pts',(9.5,25.5067810211281,-35.359186104854));
#56383=CARTESIAN_POINT('Ctrl Pts',(9.5,25.5483174157534,-35.3406363803091));
#56384=CARTESIAN_POINT('Ctrl Pts',(9.5,25.5899403696571,-35.322289289189));
#56385=CARTESIAN_POINT('Ctrl Pts',(9.5,25.631688289108,-35.3042347373429));
#56386=CARTESIAN_POINT('Ctrl Pts',(9.5,25.673436208559,-35.2861801854968));
#56387=CARTESIAN_POINT('Ctrl Pts',(9.5,25.7153114927794,-35.2684168699898));
#56388=CARTESIAN_POINT('Ctrl Pts',(9.5,25.7573416172799,-35.2510543894317));
#56389=CARTESIAN_POINT('Ctrl Pts',(9.5,25.7993717417804,-35.2336919088736));
#56390=CARTESIAN_POINT('Ctrl Pts',(9.5,25.8415589341829,-35.2167287338712));
#56391=CARTESIAN_POINT('Ctrl Pts',(9.5,25.8839510568005,-35.2002865579818));
#56392=CARTESIAN_POINT('Ctrl Pts',(9.5,25.9263431794182,-35.1838443820923));
#56393=CARTESIAN_POINT('Ctrl Pts',(9.5,25.9689399542761,-35.167922472263));
#56394=CARTESIAN_POINT('Ctrl Pts',(9.5,26.0117995124036,-35.1526686371919));
#56395=CARTESIAN_POINT('Origin',(33.,25.1089533477396,3.15105240727392));
#56396=CARTESIAN_POINT('',(16.3099522017294,25.8138525767018,2.84895274151619));
#56397=CARTESIAN_POINT('Origin',(17.2842114798612,26.0363332260021,2.7536033866521));
#56398=CARTESIAN_POINT('Ctrl Pts',(16.3099522026769,25.8138525749482,2.84895273847024));
#56399=CARTESIAN_POINT('Ctrl Pts',(16.3240895307231,25.8437370215131,2.83614511851386));
#56400=CARTESIAN_POINT('Ctrl Pts',(16.3399187528226,25.8729217068007,2.82363739624781));
#56401=CARTESIAN_POINT('Ctrl Pts',(16.3748080290301,25.9296601647623,2.79932091426426));
#56402=CARTESIAN_POINT('Ctrl Pts',(16.3938455706131,25.9571775849078,2.78752773420181));
#56403=CARTESIAN_POINT('Ctrl Pts',(16.4143885868334,25.9837360327007,2.77614554229059));
#56404=CARTESIAN_POINT('',(33.,25.1089533477396,3.15105240727392));
#56405=CARTESIAN_POINT('Origin',(6.61325378140121E-15,20.5440037453176,
8.67361737988404E-16));
#56406=CARTESIAN_POINT('Ctrl Pts',(-16.385691310591,19.4906335657927,3.17789716423393));
#56407=CARTESIAN_POINT('Ctrl Pts',(-16.3838865721657,19.4947404992376,3.17911372502469));
#56408=CARTESIAN_POINT('Ctrl Pts',(-16.3820956441718,19.4988402929659,3.1803255757144));
#56409=CARTESIAN_POINT('Ctrl Pts',(-16.3802955079033,19.5029802288914,3.18155987450784));
#56410=CARTESIAN_POINT('Ctrl Pts',(-16.3784953716348,19.5071201648169,3.18279417330128));
#56411=CARTESIAN_POINT('Ctrl Pts',(-16.3767037318314,19.5112616232316,3.18403510677131));
#56412=CARTESIAN_POINT('Ctrl Pts',(-16.3749204594914,19.5154048469311,3.18528271336203));
#56413=CARTESIAN_POINT('Ctrl Pts',(-16.3713539148114,19.5236912943301,3.18777792654347));
#56414=CARTESIAN_POINT('Ctrl Pts',(-16.3678208473976,19.5319848056864,3.19029983360368));
#56415=CARTESIAN_POINT('Ctrl Pts',(-16.3643220920495,19.540282957292,3.19284739442709));
#56416=CARTESIAN_POINT('Ctrl Pts',(-16.3573245813534,19.5568792605033,3.19794251607391));
#56417=CARTESIAN_POINT('Ctrl Pts',(-16.3504642791346,19.573494110083,3.20314024696002));
#56418=CARTESIAN_POINT('Ctrl Pts',(-16.3437394425506,19.5901276480582,3.20843815327197));
#56419=CARTESIAN_POINT('Ctrl Pts',(-16.3333325527163,19.6158685556778,3.216636824965));
#56420=CARTESIAN_POINT('Ctrl Pts',(-16.3232499873013,19.6416542601259,3.22507559721058));
#56421=CARTESIAN_POINT('Ctrl Pts',(-16.3134863331361,19.6674851436201,3.23374592772394));
#56422=CARTESIAN_POINT('Ctrl Pts',(-16.3106316200911,19.6750376192432,3.23628097302589));
#56423=CARTESIAN_POINT('Ctrl Pts',(-16.3078041721284,19.6825939649084,3.23883583254844));
#56424=CARTESIAN_POINT('Ctrl Pts',(-16.3050038513243,19.6901542140904,3.24141036122125));
#56425=CARTESIAN_POINT('Ctrl Pts',(-16.2988148796738,19.7068630739431,3.2471003110821));
#56426=CARTESIAN_POINT('Ctrl Pts',(-16.2927584396821,19.7235909289062,3.2528861111911));
#56427=CARTESIAN_POINT('Ctrl Pts',(-16.2868332639472,19.7403379264866,3.25876585540606));
#56428=CARTESIAN_POINT('Ctrl Pts',(-16.2809080882122,19.7570849240671,3.26464559962101));
#56429=CARTESIAN_POINT('Ctrl Pts',(-16.2751116707373,19.7738586442461,3.27062203393933));
#56430=CARTESIAN_POINT('Ctrl Pts',(-16.2694535638472,19.7906272310772,3.27668164700856));
#56431=CARTESIAN_POINT('Ctrl Pts',(-16.2581373500668,19.8241644047395,3.28880087314701));
#56432=CARTESIAN_POINT('Ctrl Pts',(-16.2473713706875,19.8576872094414,3.30125446802705));
#56433=CARTESIAN_POINT('Ctrl Pts',(-16.2371394993118,19.891199479047,3.31402457021168));
#56434=CARTESIAN_POINT('Ctrl Pts',(0.214931209580442,20.543989890264,-16.4986005940977));
#56435=CARTESIAN_POINT('Ctrl Pts',(0.248500277094282,20.5181273342308,-16.4981634012918));
#56436=CARTESIAN_POINT('Ctrl Pts',(0.281612583091536,20.493053464206,-16.4979577166671));
#56437=CARTESIAN_POINT('Ctrl Pts',(0.5671966423497,20.2806701732619,-16.4978943536735));
#56438=CARTESIAN_POINT('Ctrl Pts',(0.831304673132399,20.1086229690508,-16.5088512065424));
#56439=CARTESIAN_POINT('Ctrl Pts',(1.41340912589609,19.7774389533295,-16.5366009814182));
#56440=CARTESIAN_POINT('Ctrl Pts',(1.73506034135079,19.6224000490625,-16.5541218518306));
#56441=CARTESIAN_POINT('Ctrl Pts',(2.06506260776274,19.4906334205533,-16.5627719180497));
#56442=CARTESIAN_POINT('Origin',(-39.,35.,5.80048162279745E-15));
#56443=CARTESIAN_POINT('Origin',(33.,35.,5.81688018065629E-15));
#56444=CARTESIAN_POINT('Origin',(33.,26.4545372843263,5.29429254368814));
#56445=CARTESIAN_POINT('Origin',(-37.5,50.9978970953601,-20.6163621683838));
#56446=CARTESIAN_POINT('',(-37.5,51.4199384841736,-20.884468613902));
#56447=CARTESIAN_POINT('Origin',(-37.5,51.8419798729871,-21.1525750594202));
#56448=CARTESIAN_POINT('',(-37.5,51.2660035408783,-20.1943207795704));
#56449=CARTESIAN_POINT('Origin',(-37.5,50.9978970953601,-20.6163621683838));
#56450=CARTESIAN_POINT('Origin',(-37.5,51.5341099863965,-19.7722793907569));
#56451=CARTESIAN_POINT('Origin',(-50.,50.9978970953601,-20.6163621683838));
#56452=CARTESIAN_POINT('',(-50.,51.4199384841736,-20.884468613902));
#56453=CARTESIAN_POINT('Origin',(-45.2928932188135,50.9978970953601,-20.6163621683838));
#56454=CARTESIAN_POINT('',(-50.,51.2660035408783,-20.1943207795704));
#56455=CARTESIAN_POINT('Origin',(-37.5,51.95615137521,-20.0403858362751));
#56456=CARTESIAN_POINT('',(-37.5,51.6880449296918,-20.4624272250886));
#56457=CARTESIAN_POINT('Origin',(-45.2928932188135,50.9978970953601,-20.6163621683838));
#56458=CARTESIAN_POINT('Origin',(-45.2221315177632,41.5560116976042,-24.0960437966388));
#56459=CARTESIAN_POINT('',(-50.,44.1759456341881,-25.7603857162899));
#56460=CARTESIAN_POINT('',(-50.,41.5560116976042,-24.0960437966388));
#56461=CARTESIAN_POINT('Origin',(-50.,3.18714947135723,5.01707068865061));
#56462=CARTESIAN_POINT('Origin',(-49.5,45.6658960598572,-29.0097639675421));
#56463=CARTESIAN_POINT('',(-50.,45.635768184996,-29.057189944653));
#56464=CARTESIAN_POINT('',(-50.,43.4909166208504,-32.4335210551606));
#56465=CARTESIAN_POINT('',(-49.5,45.7897031282913,-29.7473377789847));
#56466=CARTESIAN_POINT('Origin',(-49.5,45.3676617394779,-29.4792313334666));
#56467=CARTESIAN_POINT('',(-49.5,46.0578095738095,-29.3252963901712));
#56468=CARTESIAN_POINT('Origin',(-50.,45.3676617394778,-29.4792313334664));
#56469=CARTESIAN_POINT('',(-50.,45.635768184996,-29.057189944653));
#56470=CARTESIAN_POINT('',(-45.2221315177632,45.7897031282913,-29.7473377789847));
#56471=CARTESIAN_POINT('Origin',(9.5,24.,-29.5));
#56472=CARTESIAN_POINT('',(9.5,24.0000000040242,-23.000000001077));
#56473=CARTESIAN_POINT('Ctrl Pts',(9.5,26.0117995124034,-23.847331362808));
#56474=CARTESIAN_POINT('Ctrl Pts',(9.5,25.9689096319939,-23.8320667357437));
#56475=CARTESIAN_POINT('Ctrl Pts',(9.5,25.9262879467264,-23.8161349281401));
#56476=CARTESIAN_POINT('Ctrl Pts',(9.5,25.883874978838,-23.7996839392245));
#56477=CARTESIAN_POINT('Ctrl Pts',(9.5,25.8414587998583,-23.7832317048023));
#56478=CARTESIAN_POINT('Ctrl Pts',(9.5,25.7992516394778,-23.7662594986502));
#56479=CARTESIAN_POINT('Ctrl Pts',(9.5,25.7572045884039,-23.7488890070158));
#56480=CARTESIAN_POINT('Ctrl Pts',(9.5,25.7151550358237,-23.7315174819583));
#56481=CARTESIAN_POINT('Ctrl Pts',(9.5,25.6732659998802,-23.7137472811973));
#56482=CARTESIAN_POINT('Ctrl Pts',(9.5,25.6314953697901,-23.6956818329298));
#56483=CARTESIAN_POINT('Ctrl Pts',(9.5,25.5897299794738,-23.6776186508207));
#56484=CARTESIAN_POINT('Ctrl Pts',(9.5,25.5480846709542,-23.6592606571989));
#56485=CARTESIAN_POINT('Ctrl Pts',(9.5,25.5065351970736,-23.640704126495));
#56486=CARTESIAN_POINT('Ctrl Pts',(9.50000000000001,25.4234324751939,-23.6035893795174));
#56487=CARTESIAN_POINT('Ctrl Pts',(9.5,25.340692297494,-23.5656796578226));
#56488=CARTESIAN_POINT('Ctrl Pts',(9.5,25.2580389063772,-23.5275796334702));
#56489=CARTESIAN_POINT('Ctrl Pts',(9.5,25.1753855152603,-23.4894796091178));
#56490=CARTESIAN_POINT('Ctrl Pts',(9.5,25.0928202181361,-23.4511864152134));
#56491=CARTESIAN_POINT('Ctrl Pts',(9.5,25.0101108671149,-23.4132090978422));
#56492=CARTESIAN_POINT('Ctrl Pts',(9.5,24.9274015160936,-23.3752317804711));
#56493=CARTESIAN_POINT('Ctrl Pts',(9.5,24.8445483055857,-23.337568859186));
#56494=CARTESIAN_POINT('Ctrl Pts',(9.5,24.7613805795409,-23.3006789941698));
#56495=CARTESIAN_POINT('Ctrl Pts',(9.5,24.6781802428869,-23.2637746643964));
#56496=CARTESIAN_POINT('Ctrl Pts',(9.5,24.5946613246052,-23.2276411758559));
#56497=CARTESIAN_POINT('Ctrl Pts',(9.5,24.5106576117287,-23.1926806714327));
#56498=CARTESIAN_POINT('Ctrl Pts',(9.5,24.4267197498417,-23.1577475727482));
#56499=CARTESIAN_POINT('Ctrl Pts',(9.5,24.3422981983971,-23.1239848109111));
#56500=CARTESIAN_POINT('Ctrl Pts',(9.5,24.2572425017914,-23.0917564080366));
#56501=CARTESIAN_POINT('Ctrl Pts',(9.5,24.2146979715,-23.0756358856371));
#56502=CARTESIAN_POINT('Ctrl Pts',(9.5,24.1719949918743,-23.0598987437645));
#56503=CARTESIAN_POINT('Ctrl Pts',(9.5,24.1291157581348,-23.0445880627847));
#56504=CARTESIAN_POINT('Ctrl Pts',(9.5,24.1076774470549,-23.0369331885468));
#56505=CARTESIAN_POINT('Ctrl Pts',(9.5,24.0861944286833,-23.0293846978839));
#56506=CARTESIAN_POINT('Ctrl Pts',(9.5,24.0646742539635,-23.0219511396643));
#56507=CARTESIAN_POINT('Ctrl Pts',(9.5,24.0539125104744,-23.0182337884897));
#56508=CARTESIAN_POINT('Ctrl Pts',(9.5,24.0431409392655,-23.0145449829623));
#56509=CARTESIAN_POINT('Ctrl Pts',(9.5,24.032359320533,-23.0108853638909));
#56510=CARTESIAN_POINT('Ctrl Pts',(9.5,24.0269687018538,-23.0090556190804));
#56511=CARTESIAN_POINT('Ctrl Pts',(9.49999999999461,24.0215753227308,-23.0072339008906));
#56512=CARTESIAN_POINT('Ctrl Pts',(9.49999999999462,24.0161787253986,-23.0054201450326));
#56513=CARTESIAN_POINT('Ctrl Pts',(9.49999999999464,24.0107824390184,-23.0036064936833));
#56514=CARTESIAN_POINT('Ctrl Pts',(9.5,24.0053865342605,-23.0018020066657));
#56515=CARTESIAN_POINT('Ctrl Pts',(9.5,24.0000000128774,-23.000000004308));
#56516=CARTESIAN_POINT('Ctrl Pts',(9.5,24.,-23.));
#56517=CARTESIAN_POINT('Ctrl Pts',(9.5,23.9945849935496,-23.0018115317267));
#56518=CARTESIAN_POINT('Ctrl Pts',(9.49999999999458,23.9891956914846,-23.0036138370378));
#56519=CARTESIAN_POINT('Ctrl Pts',(9.49999999999452,23.9838049192649,-23.005425649693));
#56520=CARTESIAN_POINT('Ctrl Pts',(9.49999999999445,23.9784141470452,-23.0072374623481));
#56521=CARTESIAN_POINT('Ctrl Pts',(9.5,23.9730112146172,-23.0090624126808));
#56522=CARTESIAN_POINT('Ctrl Pts',(9.5,23.9676115942036,-23.0108952044431));
#56523=CARTESIAN_POINT('Ctrl Pts',(9.5,23.9568123533764,-23.0145607879675));
#56524=CARTESIAN_POINT('Ctrl Pts',(9.5,23.9460253688664,-23.0182550965837));
#56525=CARTESIAN_POINT('Ctrl Pts',(9.5,23.9352502697771,-23.0219772088574));
#56526=CARTESIAN_POINT('Ctrl Pts',(9.5,23.9137000715983,-23.0294214334047));
#56527=CARTESIAN_POINT('Ctrl Pts',(9.5,23.8921975466363,-23.0369772593698));
#56528=CARTESIAN_POINT('Ctrl Pts',(9.5,23.8707404359779,-23.0446393983796));
#56529=CARTESIAN_POINT('Ctrl Pts',(9.5,23.8278262146613,-23.059963676399));
#56530=CARTESIAN_POINT('Ctrl Pts',(9.5,23.7850936566721,-23.0757132234977));
#56531=CARTESIAN_POINT('Ctrl Pts',(9.5,23.742524283212,-23.0918447791738));
#56532=CARTESIAN_POINT('Ctrl Pts',(9.5,23.6573855362917,-23.1241078905259));
#56533=CARTESIAN_POINT('Ctrl Pts',(9.5,23.572900374409,-23.1579010177367));
#56534=CARTESIAN_POINT('Ctrl Pts',(9.5,23.488912975394,-23.1928593956236));
#56535=CARTESIAN_POINT('Ctrl Pts',(9.5,23.404925576379,-23.2278177735106));
#56536=CARTESIAN_POINT('Ctrl Pts',(9.5,23.3214363011426,-23.2639422478401));
#56537=CARTESIAN_POINT('Ctrl Pts',(9.5,23.2382740201769,-23.3008321997186));
#56538=CARTESIAN_POINT('Ctrl Pts',(9.5,23.1551117392113,-23.3377221515971));
#56539=CARTESIAN_POINT('Ctrl Pts',(9.5,23.0722768545621,-23.3753785262336));
#56540=CARTESIAN_POINT('Ctrl Pts',(9.5,22.9895775029495,-23.4133521804931));
#56541=CARTESIAN_POINT('Ctrl Pts',(9.5,22.9068781513369,-23.4513258347525));
#56542=CARTESIAN_POINT('Ctrl Pts',(9.5,22.8243149666603,-23.4896182491358));
#56543=CARTESIAN_POINT('Ctrl Pts',(9.5,22.7416680667737,-23.5277146914284));
#56544=CARTESIAN_POINT('Ctrl Pts',(9.5,22.6590211668871,-23.5658111337209));
#56545=CARTESIAN_POINT('Ctrl Pts',(9.5,22.5762917681227,-23.603714446056));
#56546=CARTESIAN_POINT('Ctrl Pts',(9.5,22.493218978872,-23.6408138951459));
#56547=CARTESIAN_POINT('Ctrl Pts',(9.5,22.4516825842467,-23.6593636196908));
#56548=CARTESIAN_POINT('Ctrl Pts',(9.5,22.4100596303431,-23.677710710811));
#56549=CARTESIAN_POINT('Ctrl Pts',(9.5,22.3683117108922,-23.695765262657));
#56550=CARTESIAN_POINT('Ctrl Pts',(9.5,22.3265637914412,-23.713819814503));
#56551=CARTESIAN_POINT('Ctrl Pts',(9.5,22.2846885072208,-23.7315831300102));
#56552=CARTESIAN_POINT('Ctrl Pts',(9.5,22.2426583827203,-23.7489456105683));
#56553=CARTESIAN_POINT('Ctrl Pts',(9.5,22.2006282582199,-23.7663080911264));
#56554=CARTESIAN_POINT('Ctrl Pts',(9.5,22.1584410658174,-23.7832712661287));
#56555=CARTESIAN_POINT('Ctrl Pts',(9.5,22.1160489431998,-23.7997134420182));
#56556=CARTESIAN_POINT('Ctrl Pts',(9.50000000000001,22.0736568205821,-23.8161556179077));
#56557=CARTESIAN_POINT('Ctrl Pts',(9.5,22.031060045724,-23.8320775277365));
#56558=CARTESIAN_POINT('Ctrl Pts',(9.5,21.9882004875966,-23.847331362808));
#56559=CARTESIAN_POINT('Ctrl Pts',(9.5,21.9882004875966,-35.152668637192));
#56560=CARTESIAN_POINT('Ctrl Pts',(9.5,22.0310903680061,-35.1679332642564));
#56561=CARTESIAN_POINT('Ctrl Pts',(9.5,22.0737120532736,-35.1838650718599));
#56562=CARTESIAN_POINT('Ctrl Pts',(9.5,22.116125021162,-35.2003160607755));
#56563=CARTESIAN_POINT('Ctrl Pts',(9.5,22.1585412001417,-35.2167682951977));
#56564=CARTESIAN_POINT('Ctrl Pts',(9.5,22.2007483605221,-35.23374050135));
#56565=CARTESIAN_POINT('Ctrl Pts',(9.5,22.242795411596,-35.2511109929843));
#56566=CARTESIAN_POINT('Ctrl Pts',(9.5,22.2848449641762,-35.2684825180418));
#56567=CARTESIAN_POINT('Ctrl Pts',(9.5,22.3267340001198,-35.2862527188033));
#56568=CARTESIAN_POINT('Ctrl Pts',(9.5,22.3685046302098,-35.3043181670704));
#56569=CARTESIAN_POINT('Ctrl Pts',(9.5,22.410270020526,-35.3223813491792));
#56570=CARTESIAN_POINT('Ctrl Pts',(9.5,22.4519153290457,-35.3407393428013));
#56571=CARTESIAN_POINT('Ctrl Pts',(9.5,22.4934648029264,-35.3592958735051));
#56572=CARTESIAN_POINT('Ctrl Pts',(9.5,22.5765675248061,-35.3964106204826));
#56573=CARTESIAN_POINT('Ctrl Pts',(9.5,22.659307702506,-35.4343203421775));
#56574=CARTESIAN_POINT('Ctrl Pts',(9.5,22.7419610936227,-35.4724203665301));
#56575=CARTESIAN_POINT('Ctrl Pts',(9.5,22.8246144847395,-35.5105203908827));
#56576=CARTESIAN_POINT('Ctrl Pts',(9.5,22.9071797818639,-35.5488135847866));
#56577=CARTESIAN_POINT('Ctrl Pts',(9.5,22.9898891328852,-35.5867909021576));
#56578=CARTESIAN_POINT('Ctrl Pts',(9.5,23.0725984839066,-35.6247682195286));
#56579=CARTESIAN_POINT('Ctrl Pts',(9.5,23.1554516944143,-35.662431140814));
#56580=CARTESIAN_POINT('Ctrl Pts',(9.5,23.2386194204592,-35.6993210058301));
#56581=CARTESIAN_POINT('Ctrl Pts',(9.5,23.3217871465041,-35.7362108708462));
#56582=CARTESIAN_POINT('Ctrl Pts',(9.50000000000004,23.4052731920914,-35.7723305361407));
#56583=CARTESIAN_POINT('Ctrl Pts',(9.49999999999995,23.4892435227574,-35.8072784366652));
#56584=CARTESIAN_POINT('Ctrl Pts',(9.49999999999985,23.5732138534233,-35.8422263371897));
#56585=CARTESIAN_POINT('Ctrl Pts',(9.5,23.6576684376259,-35.8760025471646));
#56586=CARTESIAN_POINT('Ctrl Pts',(9.5,23.7427574982086,-35.9082435919634));
#56587=CARTESIAN_POINT('Ctrl Pts',(9.5,23.7853020285,-35.9243641143629));
#56588=CARTESIAN_POINT('Ctrl Pts',(9.5,23.8280050081257,-35.9401012562356));
#56589=CARTESIAN_POINT('Ctrl Pts',(9.5,23.8708842418652,-35.9554119372154));
#56590=CARTESIAN_POINT('Ctrl Pts',(9.5,23.8923225529451,-35.9630668114532));
#56591=CARTESIAN_POINT('Ctrl Pts',(9.5,23.9138055713167,-35.9706153021161));
#56592=CARTESIAN_POINT('Ctrl Pts',(9.5,23.9353257460365,-35.9780488603358));
#56593=CARTESIAN_POINT('Ctrl Pts',(9.5,23.9460874895256,-35.9817662115104));
#56594=CARTESIAN_POINT('Ctrl Pts',(9.5,23.9568590607345,-35.9854550170376));
#56595=CARTESIAN_POINT('Ctrl Pts',(9.5,23.9676406794671,-35.989114636109));
#56596=CARTESIAN_POINT('Ctrl Pts',(9.5,23.9730312981462,-35.9909443809195));
#56597=CARTESIAN_POINT('Ctrl Pts',(9.49999999999524,23.9784247177933,-35.9927659777918));
#56598=CARTESIAN_POINT('Ctrl Pts',(9.49999999999624,23.983819858151,-35.9945789780646));
#56599=CARTESIAN_POINT('Ctrl Pts',(9.49999999999724,23.9892146876407,-35.9963918738723));
#56600=CARTESIAN_POINT('Ctrl Pts',(9.5,23.9946073268916,-35.9981959396455));
#56601=CARTESIAN_POINT('Ctrl Pts',(9.5,23.9999999209526,-35.9999999735555));
#56602=CARTESIAN_POINT('Ctrl Pts',(9.5,21.9882004875966,-23.847331362808));
#56603=CARTESIAN_POINT('Ctrl Pts',(9.5,21.8205505282296,-23.376275643042));
#56604=CARTESIAN_POINT('Ctrl Pts',(9.,21.8205505282296,-23.376275643042));
#56605=CARTESIAN_POINT('Ctrl Pts',(9.5,22.0308734754341,-23.8321439286178));
#56606=CARTESIAN_POINT('Ctrl Pts',(9.49999999999997,21.8636141076127,-23.3799945381981));
#56607=CARTESIAN_POINT('Ctrl Pts',(9.01826917526517,21.8582716513203,-23.3628505969422));
#56608=CARTESIAN_POINT('Ctrl Pts',(9.5,22.0733381907741,-23.8162753226795));
#56609=CARTESIAN_POINT('Ctrl Pts',(9.50000000000008,21.9080522210625,-23.3816975070418));
#56610=CARTESIAN_POINT('Ctrl Pts',(9.03631589192582,21.8967431756777,-23.3495513478538));
#56611=CARTESIAN_POINT('Ctrl Pts',(9.5,22.1579409882236,-23.7834690781199));
#56612=CARTESIAN_POINT('Ctrl Pts',(9.49999999999993,21.9974551619948,-23.3816228520534));
#56613=CARTESIAN_POINT('Ctrl Pts',(9.07183836849214,21.9751185068201,-23.32330486165));
#56614=CARTESIAN_POINT('Ctrl Pts',(9.5,22.2000788409464,-23.7665308354962));
#56615=CARTESIAN_POINT('Ctrl Pts',(9.49999999999999,22.0425136846468,-23.3799532806648));
#56616=CARTESIAN_POINT('Ctrl Pts',(9.08931415962565,22.015022451126,-23.3103576134241));
#56617=CARTESIAN_POINT('Ctrl Pts',(9.5,22.2841024246593,-23.7318294112912));
#56618=CARTESIAN_POINT('Ctrl Pts',(9.5,22.1328834324073,-23.3739145190718));
#56619=CARTESIAN_POINT('Ctrl Pts',(9.12357368892884,22.0961862855176,-23.284913348421));
#56620=CARTESIAN_POINT('Ctrl Pts',(9.5,22.3259971280704,-23.7140617868281));
#56621=CARTESIAN_POINT('Ctrl Pts',(9.49999999999999,22.1783023884446,-23.3696111361603));
#56622=CARTESIAN_POINT('Ctrl Pts',(9.14036084384036,22.1374556044338,-23.2724137847841));
#56623=CARTESIAN_POINT('Ctrl Pts',(9.5,22.4095179570165,-23.677948027438));
#56624=CARTESIAN_POINT('Ctrl Pts',(9.5,22.2691443860353,-23.3589300101936));
#56625=CARTESIAN_POINT('Ctrl Pts',(9.17309573545695,22.2211811143838,-23.2479839196916));
#56626=CARTESIAN_POINT('Ctrl Pts',(9.5,22.4511531677501,-23.6595980500185));
#56627=CARTESIAN_POINT('Ctrl Pts',(9.50000000000004,22.3146735747321,-23.3525913977176));
#56628=CARTESIAN_POINT('Ctrl Pts',(9.18904735031177,22.2636457940565,-23.2360507661085));
#56629=CARTESIAN_POINT('Ctrl Pts',(9.5,22.5757984966601,-23.603938756548));
#56630=CARTESIAN_POINT('Ctrl Pts',(9.49999999999992,22.4497171680525,-23.3314395599938));
#56631=CARTESIAN_POINT('Ctrl Pts',(9.23550610480825,22.3927209803161,-23.2012225079895));
#56632=CARTESIAN_POINT('Ctrl Pts',(9.5,22.6585512271961,-23.5660269047261));
#56633=CARTESIAN_POINT('Ctrl Pts',(9.50000000000001,22.5411793542677,-23.3141381342362));
#56634=CARTESIAN_POINT('Ctrl Pts',(9.26461357237069,22.4810179658032,-23.1793012669497));
#56635=CARTESIAN_POINT('Ctrl Pts',(9.5,22.8238907233082,-23.4898146827162));
#56636=CARTESIAN_POINT('Ctrl Pts',(9.5,22.723314180599,-23.2762265742333));
#56637=CARTESIAN_POINT('Ctrl Pts',(9.31837705316271,22.6613097872554,-23.1386756559123));
#56638=CARTESIAN_POINT('Ctrl Pts',(9.5,22.9064762965803,-23.4515115213861));
#56639=CARTESIAN_POINT('Ctrl Pts',(9.50000000000008,22.8146676949729,-23.2555923992572));
#56640=CARTESIAN_POINT('Ctrl Pts',(9.34303153817126,22.7533032142948,-23.1199727301944));
#56641=CARTESIAN_POINT('Ctrl Pts',(9.5,23.0719192863638,-23.375541574565));
#56642=CARTESIAN_POINT('Ctrl Pts',(9.49999999999992,22.9966600101024,-23.2132413108115));
#56643=CARTESIAN_POINT('Ctrl Pts',(9.38729861344406,22.9400379161302,-23.0863051820222));
#56644=CARTESIAN_POINT('Ctrl Pts',(9.5,23.1547760839593,-23.3378733402142));
#56645=CARTESIAN_POINT('Ctrl Pts',(9.5,23.0879236376168,-23.1914132685269));
#56646=CARTESIAN_POINT('Ctrl Pts',(9.40691008519306,23.0347766742058,-23.0713416571934));
#56647=CARTESIAN_POINT('Ctrl Pts',(9.5,23.3211443668266,-23.2640694732462));
#56648=CARTESIAN_POINT('Ctrl Pts',(9.5,23.269865874317,-23.1483804270448));
#56649=CARTESIAN_POINT('Ctrl Pts',(9.44067629739217,23.2259584128153,-23.0455314877889));
#56650=CARTESIAN_POINT('Ctrl Pts',(9.5,23.4046554565311,-23.2279329146211));
#56651=CARTESIAN_POINT('Ctrl Pts',(9.49999999999991,23.3611281377987,-23.1270313510183));
#56652=CARTESIAN_POINT('Ctrl Pts',(9.45483075696682,23.3223982477998,-23.0346852271054));
#56653=CARTESIAN_POINT('Ctrl Pts',(9.5,23.5726741052635,-23.1579924983959));
#56654=CARTESIAN_POINT('Ctrl Pts',(9.50000000000008,23.543200483619,-23.0863234112952));
#56655=CARTESIAN_POINT('Ctrl Pts',(9.47746628181507,23.5159324647517,-23.0173217057587));
#56656=CARTESIAN_POINT('Ctrl Pts',(9.5,23.6571813110635,-23.1241878139021));
#56657=CARTESIAN_POINT('Ctrl Pts',(9.50000000000015,23.6345625920942,-23.0668208917478));
#56658=CARTESIAN_POINT('Ctrl Pts',(9.48594808355026,23.613023793506,-23.0108039549616));
#56659=CARTESIAN_POINT('Ctrl Pts',(9.5,23.7849228667865,-23.0757766828128));
#56660=CARTESIAN_POINT('Ctrl Pts',(9.49999999999992,23.7715467510155,-23.0398746218244));
#56661=CARTESIAN_POINT('Ctrl Pts',(9.49439707925567,23.7584321344567,-23.0043092021594));
#56662=CARTESIAN_POINT('Ctrl Pts',(9.5,23.8276666334525,-23.0600217973851));
#56663=CARTESIAN_POINT('Ctrl Pts',(9.49999999999982,23.8172008244345,-23.0312711092426));
#56664=CARTESIAN_POINT('Ctrl Pts',(9.49650254697548,23.8068644801768,-23.0026900259242));
#56665=CARTESIAN_POINT('Ctrl Pts',(9.5,23.8920548994674,-23.0370276541268));
#56666=CARTESIAN_POINT('Ctrl Pts',(9.50000000000011,23.8857012094299,-23.019029781774));
#56667=CARTESIAN_POINT('Ctrl Pts',(9.49860334653214,23.8793793478707,-23.001074302905));
#56668=CARTESIAN_POINT('Ctrl Pts',(9.5,23.9135630817008,-23.0294692825348));
#56669=CARTESIAN_POINT('Ctrl Pts',(9.50000000000052,23.9085380131238,-23.0150595806498));
#56670=CARTESIAN_POINT('Ctrl Pts',(9.49912745052014,23.9035287887977,-23.0006711718907));
#56671=CARTESIAN_POINT('Ctrl Pts',(9.5,23.9458969027414,-23.0182992158728));
#56672=CARTESIAN_POINT('Ctrl Pts',(9.49999999999972,23.9428018894257,-23.0092811501081));
#56673=CARTESIAN_POINT('Ctrl Pts',(9.49965105814884,23.9397108051149,-23.0002684139077));
#56674=CARTESIAN_POINT('Ctrl Pts',(9.5,23.9566867669937,-23.0146037737788));
#56675=CARTESIAN_POINT('Ctrl Pts',(9.5000000000002,23.9542246326999,-23.0073844572567));
#56676=CARTESIAN_POINT('Ctrl Pts',(9.49978183973438,23.9517644603695,-23.0001678143699));
#56677=CARTESIAN_POINT('Ctrl Pts',(9.5,23.9782909082579,-23.0072700390361));
#56678=CARTESIAN_POINT('Ctrl Pts',(9.49999999999955,23.9770731248063,-23.003651938446));
#56679=CARTESIAN_POINT('Ctrl Pts',(9.49995621937517,23.9758563354694,-23.0000336775452));
#56680=CARTESIAN_POINT('Ctrl Pts',(9.5,23.9890917418835,-23.0036492395423));
#56681=CARTESIAN_POINT('Ctrl Pts',(9.5,23.9884834909635,-23.0018249740171));
#56682=CARTESIAN_POINT('Ctrl Pts',(9.5,23.9878765918614,-22.999999999779));
#56683=CARTESIAN_POINT('Ctrl Pts',(9.5,24.,-23.));
#56684=CARTESIAN_POINT('Ctrl Pts',(9.5,24.,-23.));
#56685=CARTESIAN_POINT('Ctrl Pts',(9.5,24.,-23.));
#56686=CARTESIAN_POINT('Ctrl Pts',(9.00000000000003,21.8205505282297,-23.376275643042));
#56687=CARTESIAN_POINT('Ctrl Pts',(9.00499129300375,21.8308562576916,-23.372607807045));
#56688=CARTESIAN_POINT('Ctrl Pts',(9.00995373459346,21.841192773063,-23.3689583730607));
#56689=CARTESIAN_POINT('Ctrl Pts',(9.0148783576887,21.8515416277292,-23.3653340482104));
#56690=CARTESIAN_POINT('Ctrl Pts',(9.01980298078395,21.8618904823954,-23.3617097233601));
#56691=CARTESIAN_POINT('Ctrl Pts',(9.02469199992643,21.8722562234444,-23.3581088799382));
#56692=CARTESIAN_POINT('Ctrl Pts',(9.02954542600218,21.8826388751752,-23.3545316367355));
#56693=CARTESIAN_POINT('Ctrl Pts',(9.03782625969413,21.9003535804005,-23.348428204732));
#56694=CARTESIAN_POINT('Ctrl Pts',(9.04600352023976,21.9181175364614,-23.3423934607784));
#56695=CARTESIAN_POINT('Ctrl Pts',(9.05407713254697,21.9359308413409,-23.3364281049891));
#56696=CARTESIAN_POINT('Ctrl Pts',(9.05546746601018,21.938998419139,-23.3354008282933));
#56697=CARTESIAN_POINT('Ctrl Pts',(9.05685472633738,21.9420674633145,-23.3343756088419));
#56698=CARTESIAN_POINT('Ctrl Pts',(9.0582389147631,21.9451379750064,-23.3333524492007));
#56699=CARTESIAN_POINT('Ctrl Pts',(9.07474419566322,21.9817512402532,-23.3211521324161));
#56700=CARTESIAN_POINT('Ctrl Pts',(9.09081329757236,22.0185740363922,-23.3092442159581));
#56701=CARTESIAN_POINT('Ctrl Pts',(9.10644398031617,22.0556043729826,-23.2976354922079));
#56702=CARTESIAN_POINT('Ctrl Pts',(9.10865899416138,22.060851917801,-23.2959904275454));
#56703=CARTESIAN_POINT('Ctrl Pts',(9.11086526354459,22.0661038086614,-23.2943513253027));
#56704=CARTESIAN_POINT('Ctrl Pts',(9.11306274833677,22.0713599394839,-23.2927182300073));
#56705=CARTESIAN_POINT('Ctrl Pts',(9.12802360671032,22.1071445916041,-23.2815998334148));
#56706=CARTESIAN_POINT('Ctrl Pts',(9.14258366284695,22.1431405314812,-23.2707550505375));
#56707=CARTESIAN_POINT('Ctrl Pts',(9.15672841971646,22.1793183764486,-23.2601988916461));
#56708=CARTESIAN_POINT('Ctrl Pts',(9.173222617404,22.2215053530299,-23.247889357224));
#56709=CARTESIAN_POINT('Ctrl Pts',(9.18915639775547,22.2639484742488,-23.2359691362469));
#56710=CARTESIAN_POINT('Ctrl Pts',(9.20453378247886,22.3066708891664,-23.2244414206892));
#56711=CARTESIAN_POINT('Ctrl Pts',(9.20718005181625,22.3140229206496,-23.2224576347101));
#56712=CARTESIAN_POINT('Ctrl Pts',(9.20980980902293,22.3213832951449,-23.2204854962787));
#56713=CARTESIAN_POINT('Ctrl Pts',(9.21242308500115,22.3287521298052,-23.2185250123999));
#56714=CARTESIAN_POINT('Ctrl Pts',(9.23546015599538,22.393711349049,-23.2012425643632));
#56715=CARTESIAN_POINT('Ctrl Pts',(9.25720832413433,22.4592986133338,-23.1848714345782));
#56716=CARTESIAN_POINT('Ctrl Pts',(9.27764739317659,22.5255230192183,-23.1694460829554));
#56717=CARTESIAN_POINT('Ctrl Pts',(9.2823323904216,22.5407028279698,-23.165910318694));
#56718=CARTESIAN_POINT('Ctrl Pts',(9.28694852686031,22.5559163090766,-23.1624242938876));
#56719=CARTESIAN_POINT('Ctrl Pts',(9.29149540308999,22.5711639036601,-23.1589885202901));
#56720=CARTESIAN_POINT('Ctrl Pts',(9.29365149253128,22.5783941813333,-23.1573593061216));
#56721=CARTESIAN_POINT('Ctrl Pts',(9.29579199751476,22.5856321222163,-23.15574140122));
#56722=CARTESIAN_POINT('Ctrl Pts',(9.29791690448533,22.5928777430096,-23.1541348371914));
#56723=CARTESIAN_POINT('Ctrl Pts',(9.31795789315131,22.6612145719663,-23.1389825825589));
#56724=CARTESIAN_POINT('Ctrl Pts',(9.33661353356725,22.7302314074187,-23.1248370273146));
#56725=CARTESIAN_POINT('Ctrl Pts',(9.35385081456094,22.7999466691982,-23.1117399026863));
#56726=CARTESIAN_POINT('Ctrl Pts',(9.35769303749758,22.8154863345283,-23.1088205285304));
#56727=CARTESIAN_POINT('Ctrl Pts',(9.36146465901819,22.8310608309738,-23.1059533376774));
#56728=CARTESIAN_POINT('Ctrl Pts',(9.36516507939254,22.8466705668119,-23.1031389595914));
#56729=CARTESIAN_POINT('Ctrl Pts',(9.36652977322612,22.8524273479576,-23.1021010330775));
#56730=CARTESIAN_POINT('Ctrl Pts',(9.36788477789199,22.8581889130261,-23.1010702944162));
#56731=CARTESIAN_POINT('Ctrl Pts',(9.36923008056748,22.8639552738464,-23.1000467608728));
#56732=CARTESIAN_POINT('Ctrl Pts',(9.38542504339938,22.9333716221974,-23.0877253048954));
#56733=CARTESIAN_POINT('Ctrl Pts',(9.40021701095275,23.0034807157845,-23.0764457182034));
#56734=CARTESIAN_POINT('Ctrl Pts',(9.41356185654141,23.0743088141014,-23.0662539355901));
#56735=CARTESIAN_POINT('Ctrl Pts',(9.41707313527556,23.0929450129055,-23.0635722867606));
#56736=CARTESIAN_POINT('Ctrl Pts',(9.42048401358343,23.1116310616337,-23.0609661105274));
#56737=CARTESIAN_POINT('Ctrl Pts',(9.42379321375124,23.1303675580568,-23.0584366052813));
#56738=CARTESIAN_POINT('Ctrl Pts',(9.42449386001645,23.1343345759392,-23.0579010413039));
#56739=CARTESIAN_POINT('Ctrl Pts',(9.4251899470015,23.1383038499722,-23.0573689155869));
#56740=CARTESIAN_POINT('Ctrl Pts',(9.42588146840096,23.1422753857726,-23.0568402345328));
#56741=CARTESIAN_POINT('Ctrl Pts',(9.42997413403966,23.1657803244711,-23.0537113150433));
#56742=CARTESIAN_POINT('Ctrl Pts',(9.43390864964305,23.1893767278427,-23.0507017475785));
#56743=CARTESIAN_POINT('Ctrl Pts',(9.43767033422762,23.2129792231054,-23.0478230658526));
#56744=CARTESIAN_POINT('Ctrl Pts',(9.4414320188122,23.2365817183681,-23.0449443841267));
#56745=CARTESIAN_POINT('Ctrl Pts',(9.44502387076404,23.2602064841671,-23.0421942983327));
#56746=CARTESIAN_POINT('Ctrl Pts',(9.44844616386932,23.2838534804762,-23.0395729439543));
#56747=CARTESIAN_POINT('Ctrl Pts',(9.45496209937024,23.3288765974333,-23.0345819699118));
#56748=CARTESIAN_POINT('Ctrl Pts',(9.46086375084296,23.3739801923503,-23.0300574787948));
#56749=CARTESIAN_POINT('Ctrl Pts',(9.46614854505998,23.4191653817027,-23.0260035275154));
#56750=CARTESIAN_POINT('Ctrl Pts',(9.4664150994741,23.4214444319703,-23.0257990543489));
#56751=CARTESIAN_POINT('Ctrl Pts',(9.4666800837967,23.4237236883581,-23.0255957789381));
#56752=CARTESIAN_POINT('Ctrl Pts',(9.46694349854553,23.4260031516636,-23.0253937010497));
#56753=CARTESIAN_POINT('Ctrl Pts',(9.4756046317945,23.5009523924046,-23.0187493368808));
#56754=CARTESIAN_POINT('Ctrl Pts',(9.48257224642999,23.5761241008637,-23.013397473722));
#56755=CARTESIAN_POINT('Ctrl Pts',(9.48784091893683,23.6515208762116,-23.0093485597976));
#56756=CARTESIAN_POINT('Ctrl Pts',(9.48920116350281,23.6709865108331,-23.0083032275708));
#56757=CARTESIAN_POINT('Ctrl Pts',(9.49044795297831,23.6904671255976,-23.0073449072976));
#56758=CARTESIAN_POINT('Ctrl Pts',(9.49158074820728,23.7099626891003,-23.0064741240536));
#56759=CARTESIAN_POINT('Ctrl Pts',(9.49161858693997,23.7106138989546,-23.0064450373012));
#56760=CARTESIAN_POINT('Ctrl Pts',(9.49165629872179,23.7112651256649,-23.0064160480089));
#56761=CARTESIAN_POINT('Ctrl Pts',(9.49169388354751,23.7119163692475,-23.0063871561828));
#56762=CARTESIAN_POINT('Ctrl Pts',(9.49444525199611,23.7595901580923,-23.0042721521318));
#56763=CARTESIAN_POINT('Ctrl Pts',(9.49651672032079,23.8073536980638,-23.0026791277276));
#56764=CARTESIAN_POINT('Ctrl Pts',(9.49790308066639,23.855207727697,-23.0016128839398));
#56765=CARTESIAN_POINT('Ctrl Pts',(9.49790768768555,23.8553667515986,-23.0016093407011));
#56766=CARTESIAN_POINT('Ctrl Pts',(9.49791228713674,23.8555257765012,-23.0016058032811));
#56767=CARTESIAN_POINT('Ctrl Pts',(9.49791687901979,23.8556848024049,-23.0016022716799));
#56768=CARTESIAN_POINT('Ctrl Pts',(9.49860889038041,23.8796505112222,-23.001070048161));
#56769=CARTESIAN_POINT('Ctrl Pts',(9.49912904440715,23.9036389170042,-23.0006699492993));
#56770=CARTESIAN_POINT('Ctrl Pts',(9.49947652234889,23.9276501335531,-23.0004026681431));
#56771=CARTESIAN_POINT('Ctrl Pts',(9.49947711854897,23.927691331821,-23.0004022095441));
#56772=CARTESIAN_POINT('Ctrl Pts',(9.49947771424067,23.927732530156,-23.0004017513361));
#56773=CARTESIAN_POINT('Ctrl Pts',(9.49947830942397,23.9277737285583,-23.0004012935191));
#56774=CARTESIAN_POINT('Ctrl Pts',(9.49965176461952,23.939780243019,-23.0002678712071));
#56775=CARTESIAN_POINT('Ctrl Pts',(9.49978204199234,23.9517924031958,-23.0001676588957));
#56776=CARTESIAN_POINT('Ctrl Pts',(9.49986902956221,23.9638103980238,-23.0001007462648));
#56777=CARTESIAN_POINT('Ctrl Pts',(9.49986917252242,23.9638301490662,-23.0001006362969));
#56778=CARTESIAN_POINT('Ctrl Pts',(9.49986931536621,23.9638499000761,-23.0001005264185));
#56779=CARTESIAN_POINT('Ctrl Pts',(9.49986945809355,23.9638696510541,-23.0001004166297));
#56780=CARTESIAN_POINT('Ctrl Pts',(9.49991295239155,23.9698885043324,-23.0000669599194));
#56781=CARTESIAN_POINT('Ctrl Pts',(9.49994564654914,23.975908791834,-23.0000418550542));
#56782=CARTESIAN_POINT('Ctrl Pts',(9.49996740821826,23.9819305160761,-23.0000251152831));
#56783=CARTESIAN_POINT('Ctrl Pts',(9.49997828905281,23.9849413781972,-23.0000167453976));
#56784=CARTESIAN_POINT('Ctrl Pts',(9.49998644052914,23.9879525994516,-23.0000104666332));
#56785=CARTESIAN_POINT('Ctrl Pts',(9.49999186825306,23.9909641800319,-23.0000062802908));
#56786=CARTESIAN_POINT('Ctrl Pts',(9.49999458211502,23.9924699703221,-23.0000041871195));
#56787=CARTESIAN_POINT('Ctrl Pts',(9.49999661789029,23.9939777893432,-23.000002617044));
#56788=CARTESIAN_POINT('Ctrl Pts',(9.49999797235682,23.9954847287786,-23.0000015702666));
#56789=CARTESIAN_POINT('Ctrl Pts',(9.49999932682335,23.996991668214,-23.0000005234893));
#56790=CARTESIAN_POINT('Ctrl Pts',(9.5,23.9984977280603,-23.));
#56791=CARTESIAN_POINT('Ctrl Pts',(9.5,24.,-23.));
#56792=CARTESIAN_POINT('Ctrl Pts',(9.5,24.,-23.));
#56793=CARTESIAN_POINT('Ctrl Pts',(9.5,24.,-23.));
#56794=CARTESIAN_POINT('Ctrl Pts',(9.5,24.,-23.));
#56795=CARTESIAN_POINT('Ctrl Pts',(9.5,24.0107707732946,-23.0036032454852));
#56796=CARTESIAN_POINT('Ctrl Pts',(9.5,24.0113713024762,-23.0018019637283));
#56797=CARTESIAN_POINT('Ctrl Pts',(9.5,24.0119705177798,-22.9999999997818));
#56798=CARTESIAN_POINT('Ctrl Pts',(9.5,24.0215761177811,-23.0072252079635));
#56799=CARTESIAN_POINT('Ctrl Pts',(9.50000000000038,24.0227863409126,-23.0036292697814));
#56800=CARTESIAN_POINT('Ctrl Pts',(9.49995688111502,24.0239955794358,-23.0000331685107));
#56801=CARTESIAN_POINT('Ctrl Pts',(9.5,24.043142522989,-23.0145455206898));
#56802=CARTESIAN_POINT('Ctrl Pts',(9.49999999999963,24.0455947193631,-23.007354661754));
#56803=CARTESIAN_POINT('Ctrl Pts',(9.49978362345037,24.0480449740998,-23.0001664423046));
#56804=CARTESIAN_POINT('Ctrl Pts',(9.5,24.0539140788076,-23.0182343307261));
#56805=CARTESIAN_POINT('Ctrl Pts',(9.49999999999958,24.0569979580795,-23.0092477784199));
#56806=CARTESIAN_POINT('Ctrl Pts',(9.49965355251852,24.0600779429846,-23.0002664951942));
#56807=CARTESIAN_POINT('Ctrl Pts',(9.5,24.0861946039291,-23.0293847585427));
#56808=CARTESIAN_POINT('Ctrl Pts',(9.50000000000091,24.0912049332124,-23.0150154749917));
#56809=CARTESIAN_POINT('Ctrl Pts',(9.49913249141161,24.0961995403903,-23.0006672945158));
#56810=CARTESIAN_POINT('Ctrl Pts',(9.5,24.1076694276147,-23.0369303821088));
#56811=CARTESIAN_POINT('Ctrl Pts',(9.49999999999987,24.11400596502,-23.0189785154945));
#56812=CARTESIAN_POINT('Ctrl Pts',(9.49861063759759,24.1203108890296,-23.0010686949064));
#56813=CARTESIAN_POINT('Ctrl Pts',(9.5,24.1719637401203,-23.0598874716861));
#56814=CARTESIAN_POINT('Ctrl Pts',(9.50000000000028,24.1824051319777,-23.0311985864123));
#56815=CARTESIAN_POINT('Ctrl Pts',(9.49651797711653,24.1927178505562,-23.002678159501));
#56816=CARTESIAN_POINT('Ctrl Pts',(9.5,24.2146530324576,-23.0756192498966));
#56817=CARTESIAN_POINT('Ctrl Pts',(9.5,24.2279999517257,-23.0397882481961));
#56818=CARTESIAN_POINT('Ctrl Pts',(9.49441978273465,24.2410867609359,-23.0042917444127));
#56819=CARTESIAN_POINT('Ctrl Pts',(9.5,24.342252592613,-23.1239667477747));
#56820=CARTESIAN_POINT('Ctrl Pts',(9.50000000000001,24.3648279313251,-23.0666954340358));
#56821=CARTESIAN_POINT('Ctrl Pts',(9.4859961316791,24.3863285463,-23.0107670313098));
#56822=CARTESIAN_POINT('Ctrl Pts',(9.5,24.4266936912028,-23.1577367277137));
#56823=CARTESIAN_POINT('Ctrl Pts',(9.5,24.456115688764,-23.0861754816071));
#56824=CARTESIAN_POINT('Ctrl Pts',(9.47753582904777,24.4833406390942,-23.0172682908757));
#56825=CARTESIAN_POINT('Ctrl Pts',(9.5,24.5946215322546,-23.2276246151516));
#56826=CARTESIAN_POINT('Ctrl Pts',(9.5,24.6380844425336,-23.1268503195308));
#56827=CARTESIAN_POINT('Ctrl Pts',(9.4549436591157,24.6767676391327,-23.0345986860669));
#56828=CARTESIAN_POINT('Ctrl Pts',(9.5,24.6781079464887,-23.2637433301653));
#56829=CARTESIAN_POINT('Ctrl Pts',(9.5,24.7293174158525,-23.1481886748754));
#56830=CARTESIAN_POINT('Ctrl Pts',(9.44081101359461,24.7731794793018,-23.0454283451806));
#56831=CARTESIAN_POINT('Ctrl Pts',(9.5,24.8444527832798,-23.3375257588818));
#56832=CARTESIAN_POINT('Ctrl Pts',(9.5,24.911229778195,-23.1912116065894));
#56833=CARTESIAN_POINT('Ctrl Pts',(9.40708347472986,24.9643400592328,-23.0712092888382));
#56834=CARTESIAN_POINT('Ctrl Pts',(9.5,24.9273157101134,-23.3751926161801));
#56835=CARTESIAN_POINT('Ctrl Pts',(9.49999999999999,25.0024985119011,-23.2130417643524));
#56836=CARTESIAN_POINT('Ctrl Pts',(9.38748745363412,25.0590910627534,-23.0861612580384));
#56837=CARTESIAN_POINT('Ctrl Pts',(9.5,25.0927535278966,-23.4511555606396));
#56838=CARTESIAN_POINT('Ctrl Pts',(9.5,25.1844829408851,-23.2553985341106));
#56839=CARTESIAN_POINT('Ctrl Pts',(9.34325331477361,25.2458349876977,-23.1198043547188));
#56840=CARTESIAN_POINT('Ctrl Pts',(9.5,25.1753282792467,-23.489453136662));
#56841=CARTESIAN_POINT('Ctrl Pts',(9.50000000000008,25.2758237696641,-23.2760366549509));
#56842=CARTESIAN_POINT('Ctrl Pts',(9.318617008943,25.337826228914,-23.1384938689611));
#56843=CARTESIAN_POINT('Ctrl Pts',(9.5,25.3406539206004,-23.5656620578112));
#56844=CARTESIAN_POINT('Ctrl Pts',(9.49999999999992,25.4579441583579,-23.313966433972));
#56845=CARTESIAN_POINT('Ctrl Pts',(9.26488590318243,25.5181275405444,-23.1790959473744));
#56846=CARTESIAN_POINT('Ctrl Pts',(9.5,25.423403494808,-23.6035762881703));
#56847=CARTESIAN_POINT('Ctrl Pts',(9.5,25.5494052497834,-23.3312829901189));
#56848=CARTESIAN_POINT('Ctrl Pts',(9.23579261828811,25.6064362448348,-23.2010070869905));
#56849=CARTESIAN_POINT('Ctrl Pts',(9.5,25.5480717646467,-23.6592549694445));
#56850=CARTESIAN_POINT('Ctrl Pts',(9.5,25.6844789749892,-23.3524683984995));
#56851=CARTESIAN_POINT('Ctrl Pts',(9.18934162578665,25.7355596799467,-23.2358304718725));
#56852=CARTESIAN_POINT('Ctrl Pts',(9.5,25.5897238328085,-23.6776159939313));
#56853=CARTESIAN_POINT('Ctrl Pts',(9.5,25.7300285903091,-23.358820780593));
#56854=CARTESIAN_POINT('Ctrl Pts',(9.17338849315615,25.7780500646053,-23.2477650930033));
#56855=CARTESIAN_POINT('Ctrl Pts',(9.5,25.6732669052373,-23.7137476754764));
#56856=CARTESIAN_POINT('Ctrl Pts',(9.50000000000001,25.8208995483994,-23.3695293737685));
#56857=CARTESIAN_POINT('Ctrl Pts',(9.1406536309599,25.8618152227635,-23.2721956166015));
#56858=CARTESIAN_POINT('Ctrl Pts',(9.5,25.7151562043981,-23.7315179679288));
#56859=CARTESIAN_POINT('Ctrl Pts',(9.50000000000004,25.8663165149287,-23.3738465749513));
#56860=CARTESIAN_POINT('Ctrl Pts',(9.12387264986927,25.9030885502717,-23.2846909536321));
#56861=CARTESIAN_POINT('Ctrl Pts',(9.5,25.799252971265,-23.7662600488738));
#56862=CARTESIAN_POINT('Ctrl Pts',(9.49999999999996,25.9567720637753,-23.3799202018829));
#56863=CARTESIAN_POINT('Ctrl Pts',(9.08958987284599,25.9843409786744,-23.310153196582));
#56864=CARTESIAN_POINT('Ctrl Pts',(9.5,25.8414602653049,-23.7832322732144));
#56865=CARTESIAN_POINT('Ctrl Pts',(9.49999999999993,26.001911994365,-23.3816095528176));
#56866=CARTESIAN_POINT('Ctrl Pts',(9.0720880958929,26.0243201247937,-23.3231200767674));
#56867=CARTESIAN_POINT('Ctrl Pts',(9.5,25.9262896923711,-23.8161356052345));
#56868=CARTESIAN_POINT('Ctrl Pts',(9.50000000000008,26.091562040964,-23.381710222438));
#56869=CARTESIAN_POINT('Ctrl Pts',(9.0364737853881,26.1029187167218,-23.3494349509243));
#56870=CARTESIAN_POINT('Ctrl Pts',(9.5,25.9689115826802,-23.8320674299984));
#56871=CARTESIAN_POINT('Ctrl Pts',(9.49999999999992,26.1361727648094,-23.3800129429126));
#56872=CARTESIAN_POINT('Ctrl Pts',(9.01836122083488,26.1415382980706,-23.3627829574348));
#56873=CARTESIAN_POINT('Ctrl Pts',(9.5,26.0117995124034,-23.8473313628081));
#56874=CARTESIAN_POINT('Ctrl Pts',(9.5,26.1794494717704,-23.3762756430421));
#56875=CARTESIAN_POINT('Ctrl Pts',(9.,26.1794494717703,-23.3762756430421));
#56876=CARTESIAN_POINT('Ctrl Pts',(9.5,24.0000000040242,-23.));
#56877=CARTESIAN_POINT('Ctrl Pts',(9.49999999999996,24.0000472133395,-23.));
#56878=CARTESIAN_POINT('Ctrl Pts',(9.49999999932927,24.0000944225004,-23.0000000005142));
#56879=CARTESIAN_POINT('Ctrl Pts',(9.49999999798799,24.000141631506,-23.0000000015451));
#56880=CARTESIAN_POINT('Ctrl Pts',(9.49999965791715,24.0121110966267,-23.0000002629244));
#56881=CARTESIAN_POINT('Ctrl Pts',(9.49995633974189,24.0240707258725,-23.0000335849474));
#56882=CARTESIAN_POINT('Ctrl Pts',(9.4998702522827,24.0360202767678,-23.0000998054077));
#56883=CARTESIAN_POINT('Ctrl Pts',(9.49978349403696,24.0480629376004,-23.0001665418524));
#56884=CARTESIAN_POINT('Ctrl Pts',(9.49965329563524,24.0600957509431,-23.0002666927884));
#56885=CARTESIAN_POINT('Ctrl Pts',(9.49947986548288,24.0721184754532,-23.0004000949681));
#56886=CARTESIAN_POINT('Ctrl Pts',(9.49913150351934,24.0962680241944,-23.0006680544009));
#56887=CARTESIAN_POINT('Ctrl Pts',(9.4986087194461,24.1203772579043,-23.0010701701562));
#56888=CARTESIAN_POINT('Ctrl Pts',(9.4979130841039,24.1444465428718,-23.0016051831046));
#56889=CARTESIAN_POINT('Ctrl Pts',(9.49652417723532,24.1925033237533,-23.0026733909914));
#56890=CARTESIAN_POINT('Ctrl Pts',(9.49444633029441,24.2404008834145,-23.0042713242624));
#56891=CARTESIAN_POINT('Ctrl Pts',(9.49169052182656,24.2881418631175,-23.0063897356217));
#56892=CARTESIAN_POINT('Ctrl Pts',(9.49166437530495,24.2885948193269,-23.0064098346558));
#56893=CARTESIAN_POINT('Ctrl Pts',(9.49163816771039,24.2890477614159,-23.0064299805766));
#56894=CARTESIAN_POINT('Ctrl Pts',(9.49161189904947,24.2895006893906,-23.0064501733784));
#56895=CARTESIAN_POINT('Ctrl Pts',(9.48730051344177,24.3638382110829,-23.0097643489723));
#56896=CARTESIAN_POINT('Ctrl Pts',(9.48134411970086,24.4377967804438,-23.0143417189762));
#56897=CARTESIAN_POINT('Ctrl Pts',(9.47377934160028,24.5113827873064,-23.020148189609));
#56898=CARTESIAN_POINT('Ctrl Pts',(9.47168117088454,24.531792639735,-23.0217586752678));
#56899=CARTESIAN_POINT('Ctrl Pts',(9.46945903057479,24.5521739042804,-23.0234638993713));
#56900=CARTESIAN_POINT('Ctrl Pts',(9.46711315648692,24.57252684519,-23.0252635570472));
#56901=CARTESIAN_POINT('Ctrl Pts',(9.46682390991272,24.5750363653997,-23.0254854550682));
#56902=CARTESIAN_POINT('Ctrl Pts',(9.46653278205055,24.5775454534323,-23.0257087886514));
#56903=CARTESIAN_POINT('Ctrl Pts',(9.46623977302995,24.5800541104005,-23.0259335574633));
#56904=CARTESIAN_POINT('Ctrl Pts',(9.45768749975581,24.653276156256,-23.0324940527649));
#56905=CARTESIAN_POINT('Ctrl Pts',(9.44753564798023,24.7261294634645,-23.0402748674687));
#56906=CARTESIAN_POINT('Ctrl Pts',(9.43580765439745,24.7986205596957,-23.0492484623702));
#56907=CARTESIAN_POINT('Ctrl Pts',(9.43285767757367,24.8168544589815,-23.0515056171681));
#56908=CARTESIAN_POINT('Ctrl Pts',(9.42980777682099,24.8350654145798,-23.0538383945911));
#56909=CARTESIAN_POINT('Ctrl Pts',(9.42665792176129,24.8532534454377,-23.0562466662163));
#56910=CARTESIAN_POINT('Ctrl Pts',(9.4257624556697,24.8584240849108,-23.0569313090138));
#56911=CARTESIAN_POINT('Ctrl Pts',(9.42485891395591,24.8635928460027,-23.0576220492631));
#56912=CARTESIAN_POINT('Ctrl Pts',(9.42394729195393,24.8687597382769,-23.0583188868783));
#56913=CARTESIAN_POINT('Ctrl Pts',(9.41145567335872,24.9395597491057,-23.0678673945851));
#56914=CARTESIAN_POINT('Ctrl Pts',(9.39744936228768,25.0100120041573,-23.0785588266677));
#56915=CARTESIAN_POINT('Ctrl Pts',(9.38193889032673,25.0801218265281,-23.0903723732737));
#56916=CARTESIAN_POINT('Ctrl Pts',(9.37822780110935,25.0968965453431,-23.0931989233322));
#56917=CARTESIAN_POINT('Ctrl Pts',(9.37443043919756,25.1136515462175,-23.0960898323589));
#56918=CARTESIAN_POINT('Ctrl Pts',(9.37054664849349,25.1303866581631,-23.0990450356101));
#56919=CARTESIAN_POINT('Ctrl Pts',(9.36883796974238,25.1377492923413,-23.1003451811085));
#56920=CARTESIAN_POINT('Ctrl Pts',(9.36711255863857,25.1451080841838,-23.1016577737905));
#56921=CARTESIAN_POINT('Ctrl Pts',(9.36537039239686,25.152463021566,-23.1029828143487));
#56922=CARTESIAN_POINT('Ctrl Pts',(9.34910220872428,25.2211427315552,-23.1153559178207));
#56923=CARTESIAN_POINT('Ctrl Pts',(9.33137622513788,25.2894886756205,-23.1288120750233));
#56924=CARTESIAN_POINT('Ctrl Pts',(9.31218977706049,25.357505871556,-23.1433366982879));
#56925=CARTESIAN_POINT('Ctrl Pts',(9.30781686779381,25.3730081169535,-23.1466471004745));
#56926=CARTESIAN_POINT('Ctrl Pts',(9.30336798794396,25.3884931139944,-23.1500130748811));
#56927=CARTESIAN_POINT('Ctrl Pts',(9.29884292932147,25.403960598041,-23.1534345633324));
#56928=CARTESIAN_POINT('Ctrl Pts',(9.29649960113489,25.4119705255062,-23.1552064012238));
#56929=CARTESIAN_POINT('Ctrl Pts',(9.29413504811856,25.4199784648416,-23.1569937465278));
#56930=CARTESIAN_POINT('Ctrl Pts',(9.29175146133725,25.4279768831427,-23.1587949116094));
#56931=CARTESIAN_POINT('Ctrl Pts',(9.29076497192154,25.4312871695809,-23.1595403555358));
#56932=CARTESIAN_POINT('Ctrl Pts',(9.28977522583227,25.4345958245047,-23.1602881635823));
#56933=CARTESIAN_POINT('Ctrl Pts',(9.28878238789445,25.4379023226279,-23.1610382090628));
#56934=CARTESIAN_POINT('Ctrl Pts',(9.28539062367631,25.4491980856065,-23.1636005380451));
#56935=CARTESIAN_POINT('Ctrl Pts',(9.2819628000743,25.4604686495923,-23.1661889748205));
#56936=CARTESIAN_POINT('Ctrl Pts',(9.27849919458189,25.4717142458895,-23.1688032058496));
#56937=CARTESIAN_POINT('Ctrl Pts',(9.27157198359708,25.4942054384839,-23.1740316679079));
#56938=CARTESIAN_POINT('Ctrl Pts',(9.26450166607491,25.5165967715549,-23.1793632829727));
#56939=CARTESIAN_POINT('Ctrl Pts',(9.25729019799641,25.5388898580472,-23.1847957915743));
#56940=CARTESIAN_POINT('Ctrl Pts',(9.24286726183941,25.5834760310319,-23.1956608087775));
#56941=CARTESIAN_POINT('Ctrl Pts',(9.22787987878526,25.6276693970273,-23.2069289952489));
#56942=CARTESIAN_POINT('Ctrl Pts',(9.21234040799161,25.671480427866,-23.2185867719651));
#56943=CARTESIAN_POINT('Ctrl Pts',(9.20984952418265,25.6785030728981,-23.2204554435342));
#56944=CARTESIAN_POINT('Ctrl Pts',(9.20734448156849,25.6855157445879,-23.222334090199));
#56945=CARTESIAN_POINT('Ctrl Pts',(9.20482529266609,25.6925185344127,-23.2242226780239));
#56946=CARTESIAN_POINT('Ctrl Pts',(9.18941669728229,25.7353510329467,-23.2357742078093));
#56947=CARTESIAN_POINT('Ctrl Pts',(9.17347821168034,25.7778206195918,-23.2476981969414));
#56948=CARTESIAN_POINT('Ctrl Pts',(9.15702114870062,25.8199326323079,-23.259980381107));
#56949=CARTESIAN_POINT('Ctrl Pts',(9.14259793406752,25.856840226256,-23.270744669887));
#56950=CARTESIAN_POINT('Ctrl Pts',(9.1277768646073,25.8934718677887,-23.2817837311289));
#56951=CARTESIAN_POINT('Ctrl Pts',(9.11256256614465,25.9298360791784,-23.2930899518817));
#56952=CARTESIAN_POINT('Ctrl Pts',(9.11062517609986,25.9344667009126,-23.2945296869825));
#56953=CARTESIAN_POINT('Ctrl Pts',(9.10868143263058,25.9390929204726,-23.2959737374947));
#56954=CARTESIAN_POINT('Ctrl Pts',(9.10673134009713,25.943714757904,-23.2974220910081));
#56955=CARTESIAN_POINT('Ctrl Pts',(9.08972898401147,25.9840113717474,-23.3100499134061));
#56956=CARTESIAN_POINT('Ctrl Pts',(9.0722440168628,26.0239760614906,-23.3230048868648));
#56957=CARTESIAN_POINT('Ctrl Pts',(9.05428095101056,26.0636194203482,-23.3362775149017));
#56958=CARTESIAN_POINT('Ctrl Pts',(9.03664587444704,26.1025389274324,-23.3493077967898));
#56959=CARTESIAN_POINT('Ctrl Pts',(9.01854981494457,26.1411488999954,-23.3626443696441));
#56960=CARTESIAN_POINT('Ctrl Pts',(9.,26.1794494717703,-23.3762756430421));
#56961=CARTESIAN_POINT('Origin',(0.5,48.5249973351313,-4.97500266486866));
#56962=CARTESIAN_POINT('Ctrl Pts',(9.5,24.,-36.));
#56963=CARTESIAN_POINT('Ctrl Pts',(9.5,24.,-36.));
#56964=CARTESIAN_POINT('Ctrl Pts',(9.5,24.,-36.));
#56965=CARTESIAN_POINT('Ctrl Pts',(9.5,23.9892292267054,-35.9963967545148));
#56966=CARTESIAN_POINT('Ctrl Pts',(9.5,23.9886286975238,-35.9981980362717));
#56967=CARTESIAN_POINT('Ctrl Pts',(9.5,23.9880294822202,-36.0000000002183));
#56968=CARTESIAN_POINT('Ctrl Pts',(9.5,23.9784238822189,-35.9927747920365));
#56969=CARTESIAN_POINT('Ctrl Pts',(9.50000000000064,23.9772136590874,-35.9963707302186));
#56970=CARTESIAN_POINT('Ctrl Pts',(9.49995688111502,23.9760044205641,-35.9999668314893));
#56971=CARTESIAN_POINT('Ctrl Pts',(9.5,23.956857477011,-35.9854544793102));
#56972=CARTESIAN_POINT('Ctrl Pts',(9.49999999999976,23.9544052806369,-35.992645338246));
#56973=CARTESIAN_POINT('Ctrl Pts',(9.49978362345037,23.9519550259002,-35.9998335576954));
#56974=CARTESIAN_POINT('Ctrl Pts',(9.5,23.9460859211924,-35.9817656692739));
#56975=CARTESIAN_POINT('Ctrl Pts',(9.49999999999952,23.9430020419206,-35.9907522215798));
#56976=CARTESIAN_POINT('Ctrl Pts',(9.49965355251852,23.9399220570155,-35.9997335048058));
#56977=CARTESIAN_POINT('Ctrl Pts',(9.5,23.9138053960708,-35.9706152414573));
#56978=CARTESIAN_POINT('Ctrl Pts',(9.50000000000086,23.9087950667873,-35.9849845250087));
#56979=CARTESIAN_POINT('Ctrl Pts',(9.49913249141161,23.9038004596097,-35.9993327054842));
#56980=CARTESIAN_POINT('Ctrl Pts',(9.5,23.8923305723853,-35.9630696178911));
#56981=CARTESIAN_POINT('Ctrl Pts',(9.49999999999997,23.88599403498,-35.9810214845054));
#56982=CARTESIAN_POINT('Ctrl Pts',(9.49861063759758,23.8796891109704,-35.9989313050937));
#56983=CARTESIAN_POINT('Ctrl Pts',(9.5,23.8280362598797,-35.940112528314));
#56984=CARTESIAN_POINT('Ctrl Pts',(9.50000000000009,23.8175948680224,-35.9688014135879));
#56985=CARTESIAN_POINT('Ctrl Pts',(9.49651797711654,23.8072821494439,-35.9973218404989));
#56986=CARTESIAN_POINT('Ctrl Pts',(9.5,23.7853469675425,-35.9243807501034));
#56987=CARTESIAN_POINT('Ctrl Pts',(9.50000000000004,23.7720000482745,-35.9602117518039));
#56988=CARTESIAN_POINT('Ctrl Pts',(9.49441978273462,23.7589132390644,-35.9957082555875));
#56989=CARTESIAN_POINT('Ctrl Pts',(9.5,23.6577474073867,-35.8760332522253));
#56990=CARTESIAN_POINT('Ctrl Pts',(9.49999999999992,23.6351720686746,-35.9333045659642));
#56991=CARTESIAN_POINT('Ctrl Pts',(9.48599613167915,23.6136714536995,-35.9892329686897));
#56992=CARTESIAN_POINT('Ctrl Pts',(9.5,23.5733063087972,-35.842263272286));
#56993=CARTESIAN_POINT('Ctrl Pts',(9.49999999999999,23.5438843112363,-35.9138245183926));
#56994=CARTESIAN_POINT('Ctrl Pts',(9.47753582904787,23.5166593609058,-35.982731709124));
#56995=CARTESIAN_POINT('Ctrl Pts',(9.5,23.4053784677454,-35.7723753848487));
#56996=CARTESIAN_POINT('Ctrl Pts',(9.5,23.361915557466,-35.8731496804695));
#56997=CARTESIAN_POINT('Ctrl Pts',(9.45494365911559,23.3232323608673,-35.9654013139334));
#56998=CARTESIAN_POINT('Ctrl Pts',(9.5,23.3218920535115,-35.7362566698346));
#56999=CARTESIAN_POINT('Ctrl Pts',(9.49999999999992,23.2706825841475,-35.8518113251246));
#57000=CARTESIAN_POINT('Ctrl Pts',(9.44081101359471,23.2268205206985,-35.9545716548194));
#57001=CARTESIAN_POINT('Ctrl Pts',(9.5,23.15554721672,-35.6624742411183));
#57002=CARTESIAN_POINT('Ctrl Pts',(9.50000000000008,23.088770221805,-35.8087883934105));
#57003=CARTESIAN_POINT('Ctrl Pts',(9.40708347472976,23.035659940767,-35.9287907111618));
#57004=CARTESIAN_POINT('Ctrl Pts',(9.5,23.0726842898868,-35.6248073838195));
#57005=CARTESIAN_POINT('Ctrl Pts',(9.5,22.9975014880992,-35.7869582356476));
#57006=CARTESIAN_POINT('Ctrl Pts',(9.38748745363404,22.9409089372467,-35.9138387419617));
#57007=CARTESIAN_POINT('Ctrl Pts',(9.5,22.9072464721032,-35.5488444393607));
#57008=CARTESIAN_POINT('Ctrl Pts',(9.5,22.8155170591146,-35.7446014658894));
#57009=CARTESIAN_POINT('Ctrl Pts',(9.34325331477368,22.7541650123022,-35.8801956452811));
#57010=CARTESIAN_POINT('Ctrl Pts',(9.5,22.8246717207533,-35.5105468633386));
#57011=CARTESIAN_POINT('Ctrl Pts',(9.5,22.7241762303391,-35.7239633450498));
#57012=CARTESIAN_POINT('Ctrl Pts',(9.31861700894411,22.6621737710915,-35.8615061310396));
#57013=CARTESIAN_POINT('Ctrl Pts',(9.5,22.6593460793993,-35.4343379421891));
#57014=CARTESIAN_POINT('Ctrl Pts',(9.50000000000001,22.5420558416456,-35.6860335660284));
#57015=CARTESIAN_POINT('Ctrl Pts',(9.26488590318484,22.4818724594602,-35.8209040526278));
#57016=CARTESIAN_POINT('Ctrl Pts',(9.5,22.5765965051919,-35.3964237118294));
#57017=CARTESIAN_POINT('Ctrl Pts',(9.5,22.4505947502163,-35.6687170098806));
#57018=CARTESIAN_POINT('Ctrl Pts',(9.23579261828804,22.3935637551648,-35.7989929130094));
#57019=CARTESIAN_POINT('Ctrl Pts',(9.5,22.4519282353534,-35.3407450305557));
#57020=CARTESIAN_POINT('Ctrl Pts',(9.5,22.3155210250109,-35.6475316015007));
#57021=CARTESIAN_POINT('Ctrl Pts',(9.18934162578669,22.2644403200535,-35.7641695281276));
#57022=CARTESIAN_POINT('Ctrl Pts',(9.5,22.4102761671915,-35.3223840060685));
#57023=CARTESIAN_POINT('Ctrl Pts',(9.50000000000004,22.2699714096911,-35.641179219407));
#57024=CARTESIAN_POINT('Ctrl Pts',(9.17338849315615,22.2219499353948,-35.7522349069968));
#57025=CARTESIAN_POINT('Ctrl Pts',(9.5,22.3267330947627,-35.2862523245238));
#57026=CARTESIAN_POINT('Ctrl Pts',(9.49999999999996,22.1791004516003,-35.6304706262315));
#57027=CARTESIAN_POINT('Ctrl Pts',(9.1406536309599,22.1381847772365,-35.7278043833984));
#57028=CARTESIAN_POINT('Ctrl Pts',(9.5,22.2848437956018,-35.2684820320708));
#57029=CARTESIAN_POINT('Ctrl Pts',(9.49999999999997,22.1336834850712,-35.6261534250485));
#57030=CARTESIAN_POINT('Ctrl Pts',(9.12387264986921,22.0969114497283,-35.7153090463679));
#57031=CARTESIAN_POINT('Ctrl Pts',(9.5,22.2007470287351,-35.2337399511265));
#57032=CARTESIAN_POINT('Ctrl Pts',(9.50000000000004,22.0432279362249,-35.6200797981173));
#57033=CARTESIAN_POINT('Ctrl Pts',(9.08958987284604,22.0156590213257,-35.689846803418));
#57034=CARTESIAN_POINT('Ctrl Pts',(9.5,22.1585397346952,-35.2167677267856));
#57035=CARTESIAN_POINT('Ctrl Pts',(9.5,21.998088005635,-35.6183904471824));
#57036=CARTESIAN_POINT('Ctrl Pts',(9.07208809589285,21.9756798752063,-35.6768799232326));
#57037=CARTESIAN_POINT('Ctrl Pts',(9.5,22.0737103076288,-35.1838643947655));
#57038=CARTESIAN_POINT('Ctrl Pts',(9.5,21.908437959036,-35.618289777562));
#57039=CARTESIAN_POINT('Ctrl Pts',(9.03647378538813,21.8970812832782,-35.6505650490757));
#57040=CARTESIAN_POINT('Ctrl Pts',(9.5,22.0310884173198,-35.1679325700017));
#57041=CARTESIAN_POINT('Ctrl Pts',(9.5,21.8638272351906,-35.619987057087));
#57042=CARTESIAN_POINT('Ctrl Pts',(9.0183612208349,21.8584617019294,-35.6372170425652));
#57043=CARTESIAN_POINT('Ctrl Pts',(9.5,21.9882004875966,-35.1526686371919));
#57044=CARTESIAN_POINT('Ctrl Pts',(9.5,21.8205505282297,-35.6237243569579));
#57045=CARTESIAN_POINT('Ctrl Pts',(9.,21.8205505282297,-35.6237243569579));
#57046=CARTESIAN_POINT('Origin',(4.5,24.,6.93889390390723E-15));
#57047=CARTESIAN_POINT('',(-0.474937191429098,24.5000000003648,-16.9721648040778));
#57048=CARTESIAN_POINT('',(-0.474937185533101,24.5,6.93889390390723E-15));
#57049=CARTESIAN_POINT('',(-0.474939105079448,23.4999999870496,-16.9721648040678));
#57050=CARTESIAN_POINT('Ctrl Pts',(-0.474937185533101,24.5,-16.9721648040778));
#57051=CARTESIAN_POINT('Ctrl Pts',(-0.470797194023869,24.5411923954141,
-16.9724257278495));
#57052=CARTESIAN_POINT('Ctrl Pts',(-0.466146469130312,24.5823254588545,
-16.9727170296826));
#57053=CARTESIAN_POINT('Ctrl Pts',(-0.458404454236442,24.6439360926595,
-16.9731972461152));
#57054=CARTESIAN_POINT('Ctrl Pts',(-0.455695504183399,24.6644618374713,
-16.9733645613487));
#57055=CARTESIAN_POINT('Ctrl Pts',(-0.45003097975852,24.7054224004596,-16.9737126265433));
#57056=CARTESIAN_POINT('Ctrl Pts',(-0.435248508164381,24.8076327210798,
-16.9746165749486));
#57057=CARTESIAN_POINT('Ctrl Pts',(-0.417381523850264,24.9088942257275,
-16.975683228821));
#57058=CARTESIAN_POINT('Ctrl Pts',(-0.368686732985424,25.150134146398,-16.9784953288194));
#57059=CARTESIAN_POINT('Ctrl Pts',(-0.288284000987233,25.4670286188676,
-16.9829238382787));
#57060=CARTESIAN_POINT('Ctrl Pts',(-0.177378303243287,25.7745546543069,
-16.9878975211825));
#57061=CARTESIAN_POINT('Ctrl Pts',(-0.0825936022986651,26.0016402971975,
-16.9914298199687));
#57062=CARTESIAN_POINT('Ctrl Pts',(-0.0490609928049965,26.0767413134168,
-16.9925731939087));
#57063=CARTESIAN_POINT('Ctrl Pts',(-0.00467819423663701,26.169861750507,
-16.9939088357422));
#57064=CARTESIAN_POINT('Ctrl Pts',(0.00432179345813184,26.1884480232583,
-16.9941712588045));
#57065=CARTESIAN_POINT('Ctrl Pts',(0.0225700581715561,26.2255445183813,
-16.9946853096135));
#57066=CARTESIAN_POINT('Ctrl Pts',(0.0318248797997421,26.2440674949246,
-16.9949371041111));
#57067=CARTESIAN_POINT('Ctrl Pts',(0.0599035246156764,26.2994030954782,
-16.995672587935));
#57068=CARTESIAN_POINT('Ctrl Pts',(0.0790429353757529,26.3359874557493,
-16.9961364897616));
#57069=CARTESIAN_POINT('Ctrl Pts',(0.176818437108739,26.5173957465966,-16.9982977437359));
#57070=CARTESIAN_POINT('Ctrl Pts',(0.261674360831238,26.6576904507745,-16.9995234138429));
#57071=CARTESIAN_POINT('Ctrl Pts',(0.444321993216878,26.9288562035493,-17.0002526361575));
#57072=CARTESIAN_POINT('Ctrl Pts',(0.542114396216129,27.0597267530717,-16.9997573671339));
#57073=CARTESIAN_POINT('Ctrl Pts',(0.750680443960419,27.3120068120101,-16.9962341377482));
#57074=CARTESIAN_POINT('Ctrl Pts',(0.861452940867902,27.4334171664224,-16.9932079888594));
#57075=CARTESIAN_POINT('Ctrl Pts',(0.99361456223937,27.5645040251486,-16.9878439808329));
#57076=CARTESIAN_POINT('Ctrl Pts',(1.00840115368406,27.5789893043023,-16.9872207317832));
#57077=CARTESIAN_POINT('Ctrl Pts',(1.03810042360633,27.6077248047586,-16.9859214394814));
#57078=CARTESIAN_POINT('Ctrl Pts',(1.08286917614699,27.6505060822827,-16.9838920859762));
#57079=CARTESIAN_POINT('Ctrl Pts',(1.188858130302,27.7480881794548,-16.9785796041949));
#57080=CARTESIAN_POINT('Ctrl Pts',(1.28229298272252,27.8279292267126,-16.9729868122735));
#57081=CARTESIAN_POINT('Ctrl Pts',(1.47254721988554,27.9826187514255,-16.9602800962833));
#57082=CARTESIAN_POINT('Ctrl Pts',(1.60388844894043,28.0790994660127,-16.9497830742527));
#57083=CARTESIAN_POINT('Ctrl Pts',(1.87542831134558,28.2588892942784,-16.923971022276));
#57084=CARTESIAN_POINT('Ctrl Pts',(2.01562691262817,28.3421986363132,-16.9086574377018));
#57085=CARTESIAN_POINT('Ctrl Pts',(2.19646956016925,28.4379525039625,-16.8859701915491));
#57086=CARTESIAN_POINT('Ctrl Pts',(2.23291842136431,28.4566832330055,-16.8812551930949));
#57087=CARTESIAN_POINT('Ctrl Pts',(2.2880151864085,28.4841436490512,-16.873905381881));
#57088=CARTESIAN_POINT('Ctrl Pts',(2.30645431779413,28.4931925899314,-16.8714088149193));
#57089=CARTESIAN_POINT('Ctrl Pts',(2.34346217828623,28.5110715948272,-16.8663230193847));
#57090=CARTESIAN_POINT('Ctrl Pts',(2.43612492640257,28.5551344144511,-16.8534017967175));
#57091=CARTESIAN_POINT('Ctrl Pts',(2.52949327362936,28.5960520347272,-16.8394382727757));
#57092=CARTESIAN_POINT('Ctrl Pts',(2.75487169864856,28.6883783411955,-16.803857516293));
#57093=CARTESIAN_POINT('Ctrl Pts',(2.90684631178956,28.7421072493515,-16.7773800236118));
#57094=CARTESIAN_POINT('Ctrl Pts',(3.21401274740079,28.834455152834,-16.7185414151844));
#57095=CARTESIAN_POINT('Ctrl Pts',(3.3692050437863,28.873072940841,-16.686180930445));
#57096=CARTESIAN_POINT('Ctrl Pts',(3.60431757046051,28.9197700419179,-16.6329277059702));
#57097=CARTESIAN_POINT('Ctrl Pts',(3.72245604807308,28.9403067675921,-16.6051225169927));
#57098=CARTESIAN_POINT('Ctrl Pts',(3.84146173671369,28.9566050075574,-16.5754879243563));
#57099=CARTESIAN_POINT('Ctrl Pts',(3.90110916247106,28.964043838043,-16.5603602636752));
#57100=CARTESIAN_POINT('Ctrl Pts',(3.92102330682397,28.966405932644,-16.5552640265692));
#57101=CARTESIAN_POINT('Ctrl Pts',(3.96086673143964,28.9708889766091,-16.544975726032));
#57102=CARTESIAN_POINT('Ctrl Pts',(4.13998708103765,28.9899485771674,-16.4983101446476));
#57103=CARTESIAN_POINT('Ctrl Pts',(4.31754265331675,28.9991242551688,-16.4483414929103));
#57104=CARTESIAN_POINT('Ctrl Pts',(4.63080514657345,29.0007423464527,-16.3543944500403));
#57105=CARTESIAN_POINT('Ctrl Pts',(4.94167551686651,28.9876617690864,-16.2553333964929));
#57106=CARTESIAN_POINT('Ctrl Pts',(5.24786893282216,28.946165318101,-16.146223149621));
#57107=CARTESIAN_POINT('Ctrl Pts',(5.43779727915631,28.9114180710996,-16.0749371695464));
#57108=CARTESIAN_POINT('Ctrl Pts',(5.47571076690044,28.9040271040352,-16.060525344647));
#57109=CARTESIAN_POINT('Ctrl Pts',(5.55139363775732,28.8883601295569,-16.0313935531728));
#57110=CARTESIAN_POINT('Ctrl Pts',(5.5891799220155,28.8800794888932,-16.016666632018));
#57111=CARTESIAN_POINT('Ctrl Pts',(5.70195424529067,28.8539943215851,-15.9721724441926));
#57112=CARTESIAN_POINT('Ctrl Pts',(5.85099160100143,28.8158563894363,-15.9119240256477));
#57113=CARTESIAN_POINT('Ctrl Pts',(5.99743544461135,28.7711143481946,-15.8499070518029));
#57114=CARTESIAN_POINT('Ctrl Pts',(6.08816789477528,28.7411062055865,-15.8106180317806));
#57115=CARTESIAN_POINT('Ctrl Pts',(6.10627462109521,28.7350022996597,-15.8027338085013));
#57116=CARTESIAN_POINT('Ctrl Pts',(6.14240887067895,28.7225901831169,-15.7869131363904));
#57117=CARTESIAN_POINT('Ctrl Pts',(6.16043745190374,28.7162814808635,-15.7789761765381));
#57118=CARTESIAN_POINT('Ctrl Pts',(6.21431854028686,28.6970805928907,-15.7551263393622));
#57119=CARTESIAN_POINT('Ctrl Pts',(6.24999547230599,28.6839038442371,-15.7391618389056));
#57120=CARTESIAN_POINT('Ctrl Pts',(6.42718457724082,28.6161661156919,-15.659032731462));
#57121=CARTESIAN_POINT('Ctrl Pts',(6.56511818970728,28.5560582468655,-15.5939476458852));
#57122=CARTESIAN_POINT('Ctrl Pts',(6.83381314471484,28.4244430261726,-15.4622423546226));
#57123=CARTESIAN_POINT('Ctrl Pts',(6.96457354178166,28.3529347516141,-15.3956213100042));
#57124=CARTESIAN_POINT('Ctrl Pts',(7.21919473296188,28.1985882983322,-15.2613017155268));
#57125=CARTESIAN_POINT('Ctrl Pts',(7.34305540407025,28.1157508742713,-15.1936020965576));
#57126=CARTESIAN_POINT('Ctrl Pts',(7.52374793236161,27.9827805317339,-15.0916317207699));
#57127=CARTESIAN_POINT('Ctrl Pts',(7.58312770045258,27.9370018403625,-15.0575719928629));
#57128=CARTESIAN_POINT('Ctrl Pts',(7.65628611371722,27.8779133193801,-15.0149561206365));
#57129=CARTESIAN_POINT('Ctrl Pts',(7.67087193525932,27.8659960500774,-15.0064264965047));
#57130=CARTESIAN_POINT('Ctrl Pts',(7.69988883952031,27.8420132357583,-14.989392534012));
#57131=CARTESIAN_POINT('Ctrl Pts',(7.74318619480258,27.8058137690161,-14.963877248045));
#57132=CARTESIAN_POINT('Ctrl Pts',(7.89944767767118,27.6706041349955,-14.8707339720428));
#57133=CARTESIAN_POINT('Ctrl Pts',(8.03404572312412,27.5402060694125,-14.7874203361386));
#57134=CARTESIAN_POINT('Ctrl Pts',(8.24008043953904,27.3217971781574,-14.6565549244909));
#57135=CARTESIAN_POINT('Ctrl Pts',(8.33843721101683,27.2077082196918,-14.5923386141809));
#57136=CARTESIAN_POINT('Ctrl Pts',(8.47893005098055,27.0288386736179,-14.4984704418604));
#57137=CARTESIAN_POINT('Ctrl Pts',(8.52458497644703,26.9679233156009,-14.4675917513094));
#57138=CARTESIAN_POINT('Ctrl Pts',(8.59127443651523,26.874532439389,-14.4219830489157));
#57139=CARTESIAN_POINT('Ctrl Pts',(8.62417068589193,26.827332220894,-14.3993562003764));
#57140=CARTESIAN_POINT('Ctrl Pts',(8.65638641071583,26.77935680123,-14.3770147803195));
#57141=CARTESIAN_POINT('Ctrl Pts',(8.67771128879629,26.7471986843312,-14.3621861888618));
#57142=CARTESIAN_POINT('Ctrl Pts',(8.68830265601785,26.7310244203614,-14.3548011832054));
#57143=CARTESIAN_POINT('Ctrl Pts',(8.78274530658054,26.5849561141366,-14.2887748070903));
#57144=CARTESIAN_POINT('Ctrl Pts',(8.86068739391458,26.451236520966,-14.2330361409186));
#57145=CARTESIAN_POINT('Ctrl Pts',(9.00450920734481,26.1756727304695,-14.1284366214839));
#57146=CARTESIAN_POINT('Ctrl Pts',(9.07039068412542,26.0338301335152,-14.0795735600124));
#57147=CARTESIAN_POINT('Ctrl Pts',(9.15981295337757,25.8144909048872,-14.0123396480294));
#57148=CARTESIAN_POINT('Ctrl Pts',(9.18805026088068,25.7402795991016,-13.9909404624635));
#57149=CARTESIAN_POINT('Ctrl Pts',(9.22797174914896,25.6272308447628,-13.9604942443429));
#57150=CARTESIAN_POINT('Ctrl Pts',(9.24087290416293,25.5892591123023,-13.9506210958618));
#57151=CARTESIAN_POINT('Ctrl Pts',(9.25960317580872,25.5318559702848,-13.9362431667154));
#57152=CARTESIAN_POINT('Ctrl Pts',(9.26574746248233,25.5126328195426,-13.9315190639132));
#57153=CARTESIAN_POINT('Ctrl Pts',(9.27779745460633,25.4741297112776,-13.9222404425594));
#57154=CARTESIAN_POINT('Ctrl Pts',(9.33095684496213,25.3005840318675,-13.8812425302914));
#57155=CARTESIAN_POINT('Ctrl Pts',(9.37458706885838,25.1245081402695,-13.8470876782007));
#57156=CARTESIAN_POINT('Ctrl Pts',(9.43702932022959,24.8073779416153,-13.7979107470922));
#57157=CARTESIAN_POINT('Ctrl Pts',(9.4606902410544,24.6467599064343,-13.7790931247428));
#57158=CARTESIAN_POINT('Ctrl Pts',(9.48443586383693,24.4025985970691,-13.7601683668309));
#57159=CARTESIAN_POINT('Ctrl Pts',(9.49038965464922,24.3206716651867,-13.7554114608306));
#57160=CARTESIAN_POINT('Ctrl Pts',(9.49530693739123,24.2175656283315,-13.7514807390208));
#57161=CARTESIAN_POINT('Ctrl Pts',(9.49616405833992,24.196909533951,-13.7507953914246));
#57162=CARTESIAN_POINT('Ctrl Pts',(9.4976234388156,24.1555269308167,-13.7496283039473));
#57163=CARTESIAN_POINT('Ctrl Pts',(9.49822591174895,24.134783546786,-13.7491463933653));
#57164=CARTESIAN_POINT('Ctrl Pts',(9.4996434096454,24.0726722356942,-13.7480124558415));
#57165=CARTESIAN_POINT('Ctrl Pts',(9.50007135421376,24.0313686878477,-13.7476699921584));
#57166=CARTESIAN_POINT('Ctrl Pts',(9.4996662443851,23.8253629087153,-13.7479941330758));
#57167=CARTESIAN_POINT('Ctrl Pts',(9.49121911949272,23.6621935801189,-13.7547654157194));
#57168=CARTESIAN_POINT('Ctrl Pts',(9.4587721863421,23.338970590622,-13.7806183021659));
#57169=CARTESIAN_POINT('Ctrl Pts',(9.43477056821329,23.1789172141967,-13.7997005349618));
#57170=CARTESIAN_POINT('Ctrl Pts',(9.38725771360426,22.9411107629561,-13.837102628237));
#57171=CARTESIAN_POINT('Ctrl Pts',(9.36949809616687,22.8622214000734,-13.8510338887471));
#57172=CARTESIAN_POINT('Ctrl Pts',(9.33996284664004,22.7444532641515,-13.8740766634445));
#57173=CARTESIAN_POINT('Ctrl Pts',(9.32963490023978,22.7052915694536,-13.8821152835491));
#57174=CARTESIAN_POINT('Ctrl Pts',(9.31341500812318,22.6466904430213,-13.8947039518392));
#57175=CARTESIAN_POINT('Ctrl Pts',(9.30788663841741,22.6271794837453,-13.8989889326369));
#57176=CARTESIAN_POINT('Ctrl Pts',(9.29660876340497,22.5882796068097,-13.9077176220116));
#57177=CARTESIAN_POINT('Ctrl Pts',(9.29085668943634,22.5688812453494,-13.9121633262109));
#57178=CARTESIAN_POINT('Ctrl Pts',(9.27326264463063,22.5108396460112,-13.9257410693577));
#57179=CARTESIAN_POINT('Ctrl Pts',(9.26110733127937,22.4724312394044,-13.9350948377905));
#57180=CARTESIAN_POINT('Ctrl Pts',(9.2359836490324,22.396233117187,-13.9543649402863));
#57181=CARTESIAN_POINT('Ctrl Pts',(9.197068435466,22.2828327167101,-13.9841216702419));
#57182=CARTESIAN_POINT('Ctrl Pts',(9.15454267066618,22.1720448817502,-14.0163206782906));
#57183=CARTESIAN_POINT('Ctrl Pts',(9.06483682491421,21.9537804830714,-14.0837069534237));
#57184=CARTESIAN_POINT('Ctrl Pts',(8.99884082066844,21.8126764667367,-14.1326074671));
#57185=CARTESIAN_POINT('Ctrl Pts',(8.85494723107187,21.5386207964925,-14.2371585789696));
#57186=CARTESIAN_POINT('Ctrl Pts',(8.77704782875675,21.405670813631,-14.2928114145769));
#57187=CARTESIAN_POINT('Ctrl Pts',(8.6722724453834,21.2443471245385,-14.3659925148));
#57188=CARTESIAN_POINT('Ctrl Pts',(8.65094634731038,21.2123262139482,-14.3808099693033));
#57189=CARTESIAN_POINT('Ctrl Pts',(8.61839852912271,21.1646580921797,-14.4032980035455));
#57190=CARTESIAN_POINT('Ctrl Pts',(8.59649962691598,21.132980772232,-14.418386962775));
#57191=CARTESIAN_POINT('Ctrl Pts',(8.52993454319089,21.0390293942814,-14.4639952925715));
#57192=CARTESIAN_POINT('Ctrl Pts',(8.47266948695129,20.9629552569587,-14.5026850770815));
#57193=CARTESIAN_POINT('Ctrl Pts',(8.33186317621717,20.7844442014006,-14.5966605629362));
#57194=CARTESIAN_POINT('Ctrl Pts',(8.23350761084378,20.6708469934847,-14.6607986501892));
#57195=CARTESIAN_POINT('Ctrl Pts',(8.02798664018915,20.4537838351751,-14.7911955493999));
#57196=CARTESIAN_POINT('Ctrl Pts',(7.92082023511189,20.3503201317579,-14.8574563737388));
#57197=CARTESIAN_POINT('Ctrl Pts',(7.69756024180074,20.1532113754902,-14.9914043212885));
#57198=CARTESIAN_POINT('Ctrl Pts',(7.58146698708323,20.0595668291864,-15.0590928014651));
#57199=CARTESIAN_POINT('Ctrl Pts',(7.43053348243285,19.9486574100401,-15.1442265889065));
#57200=CARTESIAN_POINT('Ctrl Pts',(7.40005526334361,19.9267836397779,-15.1612797131196));
#57201=CARTESIAN_POINT('Ctrl Pts',(7.35389412278319,19.8944377549658,-15.1868925868012));
#57202=CARTESIAN_POINT('Ctrl Pts',(7.33842746673253,19.8837295297804,-15.1954388107376));
#57203=CARTESIAN_POINT('Ctrl Pts',(7.30740967665893,19.8625123594981,-15.2125058309299));
#57204=CARTESIAN_POINT('Ctrl Pts',(7.22961967073317,19.8099434141611,-15.2551289862951));
#57205=CARTESIAN_POINT('Ctrl Pts',(7.15060295917947,19.7597291386256,-15.2975172041686));
#57206=CARTESIAN_POINT('Ctrl Pts',(6.95859784236151,19.643663379666,-15.398706660168));
#57207=CARTESIAN_POINT('Ctrl Pts',(6.82744572738336,19.5722063013797,-15.4654418783362));
#57208=CARTESIAN_POINT('Ctrl Pts',(6.55867899441322,19.4410306593027,-15.5970216671956));
#57209=CARTESIAN_POINT('Ctrl Pts',(6.42106479588649,19.3813120766787,-15.661867088802));
#57210=CARTESIAN_POINT('Ctrl Pts',(6.20955760065134,19.3007335858868,-15.7574134301996));
#57211=CARTESIAN_POINT('Ctrl Pts',(6.10253067277946,19.2626984080434,-15.8047564438638));
#57212=CARTESIAN_POINT('Ctrl Pts',(5.97536382738032,19.2223584409551,-15.8591722850903));
#57213=CARTESIAN_POINT('Ctrl Pts',(5.92036101970489,19.2059472624311,-15.8823112157504));
#57214=CARTESIAN_POINT('Ctrl Pts',(5.88357966585399,19.1952029819019,-15.8976959200338));
#57215=CARTESIAN_POINT('Ctrl Pts',(5.86512256314497,19.1899263506937,-15.9053717649071));
#57216=CARTESIAN_POINT('Ctrl Pts',(5.69882430287088,19.1434188736361,-15.9741299312613));
#57217=CARTESIAN_POINT('Ctrl Pts',(5.39999274864541,19.074492569445,-16.0919981634691));
#57218=CARTESIAN_POINT('Ctrl Pts',(5.09467072163286,19.0330721579535,-16.2008146577535));
#57219=CARTESIAN_POINT('Ctrl Pts',(4.78600084505622,19.0057824464796,-16.3049424979477));
#57220=CARTESIAN_POINT('Ctrl Pts',(4.62999231317816,18.9992009497136,-16.3546623504514));
#57221=CARTESIAN_POINT('Ctrl Pts',(4.43279168890305,19.0002961473357,-16.4137722265256));
#57222=CARTESIAN_POINT('Ctrl Pts',(4.39324191842869,19.0009823911873,-16.4254421625891));
#57223=CARTESIAN_POINT('Ctrl Pts',(4.33375048997517,19.0027252741403,-16.442716809202));
#57224=CARTESIAN_POINT('Ctrl Pts',(4.29400704792877,19.004126493904,-16.45416404485));
#57225=CARTESIAN_POINT('Ctrl Pts',(4.17492350751609,19.0097483902536,-16.4879062795999));
#57226=CARTESIAN_POINT('Ctrl Pts',(4.07599373020815,19.0173787327952,-16.5147842062619));
#57227=CARTESIAN_POINT('Ctrl Pts',(3.83915890730805,19.0413234540751,-16.576965626304));
#57228=CARTESIAN_POINT('Ctrl Pts',(3.68206240407646,19.0647839505093,-16.6153200819377));
#57229=CARTESIAN_POINT('Ctrl Pts',(3.36955057108897,19.1268630786063,-16.6861010074616));
#57230=CARTESIAN_POINT('Ctrl Pts',(3.21413490427825,19.1654805263442,-16.7185270353234));
#57231=CARTESIAN_POINT('Ctrl Pts',(2.98239736299467,19.2351926447607,-16.7629034595391));
#57232=CARTESIAN_POINT('Ctrl Pts',(2.90538310626411,19.2603975176526,-16.7769850004889));
#57233=CARTESIAN_POINT('Ctrl Pts',(2.8094228570208,19.2944327021957,-16.7937169440387));
#57234=CARTESIAN_POINT('Ctrl Pts',(2.7710695434467,19.3082998337379,-16.8003227201479));
#57235=CARTESIAN_POINT('Ctrl Pts',(2.73277863773367,19.3226775130946,-16.8067553480941));
#57236=CARTESIAN_POINT('Ctrl Pts',(2.67556054843687,19.344563538547,-16.8162472115744));
#57237=CARTESIAN_POINT('Ctrl Pts',(2.63764917640111,19.3596003724586,-16.8223756344838));
#57238=CARTESIAN_POINT('Ctrl Pts',(2.44925570337053,19.4369969838961,-16.8520532630584));
#57239=CARTESIAN_POINT('Ctrl Pts',(2.30225568162101,19.5059792674876,-16.8727129885635));
#57240=CARTESIAN_POINT('Ctrl Pts',(2.01564514479671,19.6578480696034,-16.908641038543));
#57241=CARTESIAN_POINT('Ctrl Pts',(1.87603458294445,19.740734767493,-16.9239080748372));
#57242=CARTESIAN_POINT('Ctrl Pts',(1.60436758268191,19.9205579138168,-16.9497428239691));
#57243=CARTESIAN_POINT('Ctrl Pts',(1.47231010770517,20.0174927724321,-16.9603095097621));
#57244=CARTESIAN_POINT('Ctrl Pts',(1.32821025370583,20.1347476282247,-16.9699182992239));
#57245=CARTESIAN_POINT('Ctrl Pts',(1.3122526256191,20.1478975984186,-16.9709547966923));
#57246=CARTESIAN_POINT('Ctrl Pts',(1.28055048950018,20.1743535076429,-16.9729602735448));
#57247=CARTESIAN_POINT('Ctrl Pts',(1.23329014449646,20.214292636092,-16.9758690827517));
#57248=CARTESIAN_POINT('Ctrl Pts',(1.12505457098844,20.3092604112095,-16.9819822090053));
#57249=CARTESIAN_POINT('Ctrl Pts',(1.03573996025468,20.3936740696511,-16.9861392336332));
#57250=CARTESIAN_POINT('Ctrl Pts',(0.861658081702048,20.5664587608291,-16.9931895344418));
#57251=CARTESIAN_POINT('Ctrl Pts',(0.751656022760932,20.6869158203573,-16.9962081940318));
#57252=CARTESIAN_POINT('Ctrl Pts',(0.543679601113993,20.9382785472121,-16.9997402754155));
#57253=CARTESIAN_POINT('Ctrl Pts',(0.445704806056031,21.0691838702689,-17.0002523791264));
#57254=CARTESIAN_POINT('Ctrl Pts',(0.307964555949979,21.2735394717123,-16.9997110755045));
#57255=CARTESIAN_POINT('Ctrl Pts',(0.263586336154467,21.3430007932556,-16.9993117133576));
#57256=CARTESIAN_POINT('Ctrl Pts',(0.177996277698543,21.4846214320167,-16.9981645073496));
#57257=CARTESIAN_POINT('Ctrl Pts',(0.137138960301268,21.5561932637163,-16.997421818723));
#57258=CARTESIAN_POINT('Ctrl Pts',(0.0202552462301792,21.7731461194819,
-16.9948346932133));
#57259=CARTESIAN_POINT('Ctrl Pts',(-0.0500966079618834,21.9207591671011,
-16.9926356455613));
#57260=CARTESIAN_POINT('Ctrl Pts',(-0.175972691707234,22.2218265075116,
-16.9879550338172));
#57261=CARTESIAN_POINT('Ctrl Pts',(-0.231496448747289,22.3752809718075,
-16.9854724072299));
#57262=CARTESIAN_POINT('Ctrl Pts',(-0.303568940988182,22.6098855908799,
-16.9819362864954));
#57263=CARTESIAN_POINT('Ctrl Pts',(-0.32572090828689,22.6888255880473,-16.9807879632478));
#57264=CARTESIAN_POINT('Ctrl Pts',(-0.356097812468616,22.808360712486,-16.9791534736861));
#57265=CARTESIAN_POINT('Ctrl Pts',(-0.370573166407556,22.8684096884495,
-16.9783581512183));
#57266=CARTESIAN_POINT('Ctrl Pts',(-0.383967695011297,22.9288852925971,
-16.9776029855594));
#57267=CARTESIAN_POINT('Ctrl Pts',(-0.392655725938007,22.9692977589163,
-16.9771092273512));
#57268=CARTESIAN_POINT('Ctrl Pts',(-0.396879263255509,22.9895540629632,
-16.9768671715761));
#57269=CARTESIAN_POINT('Ctrl Pts',(-0.433731147228075,23.1719555303405,
-16.9747394571526));
#57270=CARTESIAN_POINT('Ctrl Pts',(-0.458389000150122,23.3353476343703,
-16.9732077566867));
#57271=CARTESIAN_POINT('Ctrl Pts',(-0.4749371855331,23.5,-16.9721648040778));
#57272=CARTESIAN_POINT('',(-0.4749371855331,23.5,6.93889390390723E-15));
#57273=CARTESIAN_POINT('Origin',(33.,26.4545372843263,5.29429254368814));
#57274=CARTESIAN_POINT('Ctrl Pts',(16.0339928845406,26.2575775584219,4.83472006151403));
#57275=CARTESIAN_POINT('Ctrl Pts',(16.0482886954921,26.2396927012492,4.84238500383155));
#57276=CARTESIAN_POINT('Ctrl Pts',(16.0628693069814,26.2226807213726,4.85090739382797));
#57277=CARTESIAN_POINT('Ctrl Pts',(16.077753848377,26.2064867817649,4.86016013510863));
#57278=CARTESIAN_POINT('Ctrl Pts',(16.0870581940121,26.1963639296529,4.86594403537529));
#57279=CARTESIAN_POINT('Ctrl Pts',(16.0964813007413,26.1865604802237,4.87201444823721));
#57280=CARTESIAN_POINT('Ctrl Pts',(16.1060278410909,26.1770625127317,4.87835053916283));
#57281=CARTESIAN_POINT('Ctrl Pts',(16.1235862887443,26.159593402571,4.89000417668698));
#57282=CARTESIAN_POINT('Ctrl Pts',(16.1415613272045,26.1431606937632,4.90255192203326));
#57283=CARTESIAN_POINT('Ctrl Pts',(16.1599798307474,26.1277228536324,4.91588492234545));
#57284=CARTESIAN_POINT('Ctrl Pts',(16.1675955531722,26.1213395823205,4.92139787996607));
#57285=CARTESIAN_POINT('Ctrl Pts',(16.175287093708,26.1151264693412,4.92704572621618));
#57286=CARTESIAN_POINT('Ctrl Pts',(16.1830563521511,26.1090811176398,4.93282326850936));
#57287=CARTESIAN_POINT('Ctrl Pts',(16.1896961237522,26.1039146329825,4.93776087761618));
#57288=CARTESIAN_POINT('Ctrl Pts',(16.1964043280784,26.0988626434749,4.94280180897596));
#57289=CARTESIAN_POINT('Ctrl Pts',(16.2031398739707,26.0939549260933,4.94791072700146));
#57290=CARTESIAN_POINT('Ctrl Pts',(16.209875419863,26.0890472087118,4.95301964502696));
#57291=CARTESIAN_POINT('Ctrl Pts',(16.2166324893586,26.0842872989932,4.95819191194151));
#57292=CARTESIAN_POINT('Ctrl Pts',(16.2234120418664,26.0796699800677,4.9634232277976));
#57293=CARTESIAN_POINT('Ctrl Pts',(16.236971146882,26.0704353422166,4.97388585950979));
#57294=CARTESIAN_POINT('Ctrl Pts',(16.2506201839462,26.0617705217472,4.98458418684746));
#57295=CARTESIAN_POINT('Ctrl Pts',(16.2643659505407,26.0536422887736,4.99548959433719));
#57296=CARTESIAN_POINT('Ctrl Pts',(16.2852187040666,26.041311507683,5.01203343515676));
#57297=CARTESIAN_POINT('Ctrl Pts',(16.3062940068527,26.0302132424319,5.02905416908863));
#57298=CARTESIAN_POINT('Ctrl Pts',(16.3276138236464,26.0202722072282,5.04647437887169));
#57299=CARTESIAN_POINT('Ctrl Pts',(16.3344012997453,26.0171073329943,5.05202035793349));
#57300=CARTESIAN_POINT('Ctrl Pts',(16.3412135588188,26.0140599452802,5.05760717962358));
#57301=CARTESIAN_POINT('Ctrl Pts',(16.3480513096296,26.0111282125913,5.06323325453684));
#57302=CARTESIAN_POINT('Ctrl Pts',(16.3716350535321,26.0010165201885,5.08263786777905));
#57303=CARTESIAN_POINT('Ctrl Pts',(16.3955215054915,25.992278737261,5.10250485728671));
#57304=CARTESIAN_POINT('Ctrl Pts',(16.419743160732,25.9848775660295,5.1227706820804));
#57305=CARTESIAN_POINT('Ctrl Pts',(16.4246028876691,25.9833926274139,5.12683672850353));
#57306=CARTESIAN_POINT('Ctrl Pts',(16.4294761080983,25.9819616241679,5.13091893625157));
#57307=CARTESIAN_POINT('Ctrl Pts',(16.4343630844679,25.980584459025,5.13501693542079));
#57308=CARTESIAN_POINT('Ctrl Pts',(16.4416741962513,25.9785241649818,5.141147705809));
#57309=CARTESIAN_POINT('Ctrl Pts',(16.4490048161393,25.9765878758654,5.14730420709631));
#57310=CARTESIAN_POINT('Ctrl Pts',(16.4563305291426,25.9747798143556,5.15346367588301));
#57311=CARTESIAN_POINT('Ctrl Pts',(16.4636562421459,25.9729717528457,5.15962314466971));
#57312=CARTESIAN_POINT('Ctrl Pts',(16.4709846055243,25.9712897602985,5.1657919159592));
#57313=CARTESIAN_POINT('Ctrl Pts',(16.478316560937,25.9697312787863,5.17196864172131));
#57314=CARTESIAN_POINT('Ctrl Pts',(16.4929804717623,25.9666143157621,5.18432209324552));
#57315=CARTESIAN_POINT('Ctrl Pts',(16.5076587507244,25.9639910105231,5.19670725815659));
#57316=CARTESIAN_POINT('Ctrl Pts',(16.5223584328467,25.9618460415304,5.20911426434256));
#57317=CARTESIAN_POINT('Ctrl Pts',(16.5479617237647,25.9581100243382,5.23072426829765));
#57318=CARTESIAN_POINT('Ctrl Pts',(16.5736298479289,25.9558224013621,5.25240059770458));
#57319=CARTESIAN_POINT('Ctrl Pts',(16.5993986719124,25.954945341985,5.27409622848867));
#57320=CARTESIAN_POINT('Ctrl Pts',(16.6032192880079,25.9548153047285,5.277312932372));
#57321=CARTESIAN_POINT('Ctrl Pts',(16.6070421177399,25.9547163648842,5.28053008665054));
#57322=CARTESIAN_POINT('Ctrl Pts',(16.6108672780061,25.9546484933932,5.2837475591227));
#57323=CARTESIAN_POINT('Ctrl Pts',(16.6256795946141,25.9543856719837,5.29620670269277));
#57324=CARTESIAN_POINT('Ctrl Pts',(16.6405268572356,25.9545883150099,5.30867030528035));
#57325=CARTESIAN_POINT('Ctrl Pts',(16.6554162650306,25.9552580516208,5.3211299762963));
#57326=CARTESIAN_POINT('Ctrl Pts',(16.6628609689281,25.9555929199262,5.32735981180427));
#57327=CARTESIAN_POINT('Ctrl Pts',(16.670316209119,25.9560446440895,5.33358865896399));
#57328=CARTESIAN_POINT('Ctrl Pts',(16.6777829536176,25.9566139320155,5.33981545246558));
#57329=CARTESIAN_POINT('Ctrl Pts',(16.681516325867,25.9568985759785,5.34292884921637));
#57330=CARTESIAN_POINT('Ctrl Pts',(16.6852525741933,25.9572126162338,5.34604173240083));
#57331=CARTESIAN_POINT('Ctrl Pts',(16.6889918234758,25.9575561736078,5.34915396537015));
#57332=CARTESIAN_POINT('Ctrl Pts',(16.690861448117,25.9577279522947,5.35071008185481));
#57333=CARTESIAN_POINT('Ctrl Pts',(16.6927318229973,25.9579071106011,5.35226603574635));
#57334=CARTESIAN_POINT('Ctrl Pts',(16.6946029640567,25.958093665698,5.35382180979552));
#57335=CARTESIAN_POINT('Ctrl Pts',(16.6955385345864,25.9581869432465,5.3545996968201));
#57336=CARTESIAN_POINT('Ctrl Pts',(16.6964618802871,25.9582808193014,5.35536728062135));
#57337=CARTESIAN_POINT('Ctrl Pts',(16.6973887994847,25.9583768342247,5.35613757384417));
#57338=CARTESIAN_POINT('Ctrl Pts',(16.6983157186823,25.9584728491481,5.35690786706699));
#57339=CARTESIAN_POINT('Ctrl Pts',(16.6992426416197,25.9585706572376,5.35767793144793));
#57340=CARTESIAN_POINT('Ctrl Pts',(16.7001695682977,25.9586702584785,5.3584477669892));
#57341=CARTESIAN_POINT('Ctrl Pts',(0.321034048597817,44.2777095070773,-16.496876587392));
#57342=CARTESIAN_POINT('Ctrl Pts',(0.334078182671872,44.0705712895835,-16.4966227447236));
#57343=CARTESIAN_POINT('Ctrl Pts',(0.346147593727982,43.9243235322772,-16.6433959637249));
#57344=CARTESIAN_POINT('Ctrl Pts',(0.307535768851996,44.2768333852379,-16.497139267868));
#57345=CARTESIAN_POINT('Ctrl Pts',(0.32115157242211,44.0697030498192,-16.4968849768605));
#57346=CARTESIAN_POINT('Ctrl Pts',(0.333504576783726,43.9234749343164,-16.6436941271133));
#57347=CARTESIAN_POINT('Ctrl Pts',(0.294017346932686,44.2758981934479,-16.4973857263738));
#57348=CARTESIAN_POINT('Ctrl Pts',(0.308206040614918,44.0687776043361,-16.4971323872042));
#57349=CARTESIAN_POINT('Ctrl Pts',(0.320842694094729,43.9225707071434,-16.6439790196373));
#57350=CARTESIAN_POINT('Ctrl Pts',(0.267039396841221,44.27391662747,-16.4978444642199));
#57351=CARTESIAN_POINT('Ctrl Pts',(0.282371646107752,44.0668191614445,-16.4975958245399));
#57352=CARTESIAN_POINT('Ctrl Pts',(0.295574090707277,43.9206577286911,-16.6445202461941));
#57353=CARTESIAN_POINT('Ctrl Pts',(0.253563318677811,44.2728691821441,-16.4980570656251));
#57354=CARTESIAN_POINT('Ctrl Pts',(0.269466916331725,44.0657850965016,-16.4978121729084));
#57355=CARTESIAN_POINT('Ctrl Pts',(0.282951868731823,43.9196479380401,-16.644776944703));
#57356=CARTESIAN_POINT('Ctrl Pts',(0.213173600931101,44.2695576149692,-16.4986448596443));
#57357=CARTESIAN_POINT('Ctrl Pts',(0.230789208343801,44.0625190499157,-16.4984153937458));
#57358=CARTESIAN_POINT('Ctrl Pts',(0.245121279113449,43.9164593690092,-16.6455055488628));
#57359=CARTESIAN_POINT('Ctrl Pts',(0.186298475258698,44.2671242747577,-16.4989700430965));
#57360=CARTESIAN_POINT('Ctrl Pts',(0.205054254630706,44.0601233301731,-16.4987564104361));
#57361=CARTESIAN_POINT('Ctrl Pts',(0.219948985085661,43.9141214063132,-16.6459359637993));
#57362=CARTESIAN_POINT('Ctrl Pts',(0.105825878010724,44.2591529071548,-16.4997478557418));
#57363=CARTESIAN_POINT('Ctrl Pts',(0.127994124910921,44.0522861114256,-16.4995982912245));
#57364=CARTESIAN_POINT('Ctrl Pts',(0.144575202554741,43.906475946942,-16.6470632548686));
#57365=CARTESIAN_POINT('Ctrl Pts',(0.0523811410166356,44.2529437369118,
-16.5000027615431));
#57366=CARTESIAN_POINT('Ctrl Pts',(0.0768198248561238,44.0461951243862,
-16.4999178604957));
#57367=CARTESIAN_POINT('Ctrl Pts',(0.0945167711882191,43.9005370741829,
-16.6475961824246));
#57368=CARTESIAN_POINT('Ctrl Pts',(-0.107350614477069,44.2316680864431,
-16.4999944092424));
#57369=CARTESIAN_POINT('Ctrl Pts',(-0.0761321294294826,44.0253574854767,
-16.5001684527276));
#57370=CARTESIAN_POINT('Ctrl Pts',(-0.0550942394312359,43.8802288896034,
-16.6485550431313));
#57371=CARTESIAN_POINT('Ctrl Pts',(-0.213035833808924,44.2139564350666,
-16.4989582457926));
#57372=CARTESIAN_POINT('Ctrl Pts',(-0.177314759062477,44.0080500010336,
-16.4993908078766));
#57373=CARTESIAN_POINT('Ctrl Pts',(-0.154083150146027,43.8633708391614,
-16.6483410814393));
#57374=CARTESIAN_POINT('Ctrl Pts',(-0.422829790157967,44.1715971665048,
-16.4949150477184));
#57375=CARTESIAN_POINT('Ctrl Pts',(-0.378133313017958,43.9667246375007,
-16.4960324415121));
#57376=CARTESIAN_POINT('Ctrl Pts',(-0.350584376434533,43.8231263425323,
-16.6462901344215));
#57377=CARTESIAN_POINT('Ctrl Pts',(-0.526938468414131,44.1469492910955,
-16.491907937397));
#57378=CARTESIAN_POINT('Ctrl Pts',(-0.477778440005314,43.9427009960084,
-16.4934505609926));
#57379=CARTESIAN_POINT('Ctrl Pts',(-0.448096637091592,43.7997396541264,
-16.6444530862772));
#57380=CARTESIAN_POINT('Ctrl Pts',(-0.733587594662706,44.0907445802113,
-16.4840086388606));
#57381=CARTESIAN_POINT('Ctrl Pts',(-0.675522285528619,43.8879685573675,
-16.4865649802999));
#57382=CARTESIAN_POINT('Ctrl Pts',(-0.641652292512058,43.7464596423238,
-16.6392391144044));
#57383=CARTESIAN_POINT('Ctrl Pts',(-0.836128020523552,44.0591876523663,
-16.4791163820797));
#57384=CARTESIAN_POINT('Ctrl Pts',(-0.773630842788747,43.85725253155,-16.4822597770412));
#57385=CARTESIAN_POINT('Ctrl Pts',(-0.737695666593328,43.7165662342863,
-16.6358621269656));
#57386=CARTESIAN_POINT('Ctrl Pts',(-0.988754343263762,44.0066257334661,
-16.4704268781621));
#57387=CARTESIAN_POINT('Ctrl Pts',(-0.919592667679679,43.8061296100387,
-16.4745719708769));
#57388=CARTESIAN_POINT('Ctrl Pts',(-0.880651450997229,43.6668004399974,
-16.62970542955));
#57389=CARTESIAN_POINT('Ctrl Pts',(-1.03943225076959,43.988233336078,-16.4673051794513));
#57390=CARTESIAN_POINT('Ctrl Pts',(-0.968061533919264,43.7882402439072,
-16.471803341561));
#57391=CARTESIAN_POINT('Ctrl Pts',(-0.92811836158864,43.6493902559039,-16.6274713470767));
#57392=CARTESIAN_POINT('Ctrl Pts',(-1.11515046567206,43.9593254565497,-16.462292648905));
#57393=CARTESIAN_POINT('Ctrl Pts',(-1.04046157511159,43.760131242437,-16.4673503544702));
#57394=CARTESIAN_POINT('Ctrl Pts',(-0.999039003666644,43.6220311175392,
-16.6238556629229));
#57395=CARTESIAN_POINT('Ctrl Pts',(-1.14034008702055,43.9494695740836,-16.4605668083992));
#57396=CARTESIAN_POINT('Ctrl Pts',(-1.06454821112494,43.7505474186053,-16.4658157518771));
#57397=CARTESIAN_POINT('Ctrl Pts',(-1.02263258838498,43.6127040541935,-16.6226063432779));
#57398=CARTESIAN_POINT('Ctrl Pts',(-1.19061925892548,43.9293155100069,-16.4570064394505));
#57399=CARTESIAN_POINT('Ctrl Pts',(-1.11262228707775,43.7309512076575,-16.4626476168865));
#57400=CARTESIAN_POINT('Ctrl Pts',(-1.06972602765263,43.5936328230074,-16.6200209173139));
#57401=CARTESIAN_POINT('Ctrl Pts',(-1.21573107838862,43.9190077883623,-16.4551701883059));
#57402=CARTESIAN_POINT('Ctrl Pts',(-1.13663118653057,43.7209293797071,-16.4610125155677));
#57403=CARTESIAN_POINT('Ctrl Pts',(-1.09324674012034,43.5838796294641,-16.618683550189));
#57404=CARTESIAN_POINT('Ctrl Pts',(-1.3406740926079,43.8665114056024,-16.4457484072491));
#57405=CARTESIAN_POINT('Ctrl Pts',(-1.25611592982861,43.6698761529651,-16.4526150324278));
#57406=CARTESIAN_POINT('Ctrl Pts',(-1.21027325465697,43.5342106859547,-16.6118037002477));
#57407=CARTESIAN_POINT('Ctrl Pts',(-1.43874378672612,43.8214268381111,-16.4374378027854));
#57408=CARTESIAN_POINT('Ctrl Pts',(-1.34984750421121,43.6260493224596,-16.445193094768));
#57409=CARTESIAN_POINT('Ctrl Pts',(-1.3021291667423,43.4915646194171,-16.6056797596469));
#57410=CARTESIAN_POINT('Ctrl Pts',(-1.72749788443196,43.6771991720061,-16.4104580032492));
#57411=CARTESIAN_POINT('Ctrl Pts',(-1.62585456299005,43.4858144841423,-16.4210581992283));
#57412=CARTESIAN_POINT('Ctrl Pts',(-1.5725875499331,43.3551562723534,-16.5857017103286));
#57413=CARTESIAN_POINT('Ctrl Pts',(-1.9127446936616,43.5691113883,-16.3897439917078));
#57414=CARTESIAN_POINT('Ctrl Pts',(-1.80274205830027,43.3807393221566,-16.4024878858354));
#57415=CARTESIAN_POINT('Ctrl Pts',(-1.74609695837727,43.2529516481594,-16.5702431598975));
#57416=CARTESIAN_POINT('Ctrl Pts',(-2.1801557392676,43.3896071926388,-16.3555799666888));
#57417=CARTESIAN_POINT('Ctrl Pts',(-2.05760446502451,43.2064579036073,-16.3718931324892));
#57418=CARTESIAN_POINT('Ctrl Pts',(-1.99656460420932,43.0832067018407,-16.5448031114995));
#57419=CARTESIAN_POINT('Ctrl Pts',(-2.26754491058278,43.3268692367125,-16.3436754924434));
#57420=CARTESIAN_POINT('Ctrl Pts',(-2.14090553035905,43.1454987345458,-16.3612235417513));
#57421=CARTESIAN_POINT('Ctrl Pts',(-2.07841672068826,43.0238779812105,-16.5359471304104));
#57422=CARTESIAN_POINT('Ctrl Pts',(-2.39602241125449,43.2284104250473,-16.3251630538784));
#57423=CARTESIAN_POINT('Ctrl Pts',(-2.26324112913542,43.0498815519994,-16.3446457798798));
#57424=CARTESIAN_POINT('Ctrl Pts',(-2.19875377361068,42.9307615436581,-16.5222160833336));
#57425=CARTESIAN_POINT('Ctrl Pts',(-2.4384136297981,43.1948651021794,-16.3188829280199));
#57426=CARTESIAN_POINT('Ctrl Pts',(-2.30360778271325,43.0172911666837,-16.3390206470251));
#57427=CARTESIAN_POINT('Ctrl Pts',(-2.23845904720143,42.8990351188427,-16.5175645484453));
#57428=CARTESIAN_POINT('Ctrl Pts',(-2.5013483955168,43.1434553651894,-16.3093134885055));
#57429=CARTESIAN_POINT('Ctrl Pts',(-2.36350239470388,42.9673565647272,-16.3304535133341));
#57430=CARTESIAN_POINT('Ctrl Pts',(-2.29740621067309,42.8504103436033,-16.5104900878419));
#57431=CARTESIAN_POINT('Ctrl Pts',(-2.52221795974619,43.1261368034609,-16.3060987995381));
#57432=CARTESIAN_POINT('Ctrl Pts',(-2.38336413494237,42.9505314385688,-16.3275753119188));
#57433=CARTESIAN_POINT('Ctrl Pts',(-2.31695346092089,42.8340295394261,-16.508115741492));
#57434=CARTESIAN_POINT('Ctrl Pts',(-2.56373951624231,43.0911348998851,-16.2996221180008));
#57435=CARTESIAN_POINT('Ctrl Pts',(-2.42287279694903,42.9165270650644,-16.321777494731));
#57436=CARTESIAN_POINT('Ctrl Pts',(-2.3558441749912,42.8009219471062,-16.5033371082496));
#57437=CARTESIAN_POINT('Ctrl Pts',(-2.58440772848289,43.0734372910358,-16.2963575090795));
#57438=CARTESIAN_POINT('Ctrl Pts',(-2.44253529767474,42.8993336069646,-16.3188554855158));
#57439=CARTESIAN_POINT('Ctrl Pts',(-2.37520283114705,42.7841816631336,-16.5009308965196));
#57440=CARTESIAN_POINT('Ctrl Pts',(-2.76898876271576,42.9129091805958,-16.2668469274607));
#57441=CARTESIAN_POINT('Ctrl Pts',(-2.61835540789446,42.7431513199272,-16.2924080344925));
#57442=CARTESIAN_POINT('Ctrl Pts',(-2.54808864778449,42.6323323225514,-16.4792048254679));
#57443=CARTESIAN_POINT('Ctrl Pts',(-2.92301708649477,42.7613001461326,-16.2396947338131));
#57444=CARTESIAN_POINT('Ctrl Pts',(-2.76462847126197,42.5957682985728,-16.2681310777436));
#57445=CARTESIAN_POINT('Ctrl Pts',(-2.69235760204375,42.488886199182,-16.4593927479317));
#57446=CARTESIAN_POINT('Ctrl Pts',(-3.21259129366432,42.4414613853005,-16.1848994780706));
#57447=CARTESIAN_POINT('Ctrl Pts',(-3.03897378350019,42.2850128986459,-16.2192940222789));
#57448=CARTESIAN_POINT('Ctrl Pts',(-2.96358413143859,42.1861517320565,-16.4200413247235));
#57449=CARTESIAN_POINT('Ctrl Pts',(-3.34812899112022,42.2732247223232,-16.1572537757578));
#57450=CARTESIAN_POINT('Ctrl Pts',(-3.16707816112672,42.1214334676319,-16.1947098049125));
#57451=CARTESIAN_POINT('Ctrl Pts',(-3.09053404151204,42.0268568930642,-16.4004996968118));
#57452=CARTESIAN_POINT('Ctrl Pts',(-3.53828868842179,42.0088979382797,-16.1162873356813));
#57453=CARTESIAN_POINT('Ctrl Pts',(-3.34597462567252,41.8649168770618,-16.1584948890192));
#57454=CARTESIAN_POINT('Ctrl Pts',(-3.26864505239508,41.7764635010048,-16.3722252421456));
#57455=CARTESIAN_POINT('Ctrl Pts',(-3.5994799346103,41.9187901440346,-16.1027143504919));
#57456=CARTESIAN_POINT('Ctrl Pts',(-3.40351260983138,41.7773425460961,-16.1465055224545));
#57457=CARTESIAN_POINT('Ctrl Pts',(-3.32595916749315,41.6910871652366,-16.362972412406));
#57458=CARTESIAN_POINT('Ctrl Pts',(-3.67327289887432,41.8036856256223,-16.0859347036074));
#57459=CARTESIAN_POINT('Ctrl Pts',(-3.47268299468521,41.6656131275086,-16.1317391824527));
#57460=CARTESIAN_POINT('Ctrl Pts',(-3.3950765443778,41.5820004939642,-16.3517021387782));
#57461=CARTESIAN_POINT('Ctrl Pts',(-3.68790324489889,41.7805305132082,-16.0825865601582));
#57462=CARTESIAN_POINT('Ctrl Pts',(-3.48640397870713,41.6431129782816,-16.1287915877042));
#57463=CARTESIAN_POINT('Ctrl Pts',(-3.40877989888389,41.5600546868429,-16.3494618416137));
#57464=CARTESIAN_POINT('Ctrl Pts',(-3.71686467531462,41.7340227710879,-16.0759179456141));
#57465=CARTESIAN_POINT('Ctrl Pts',(-3.51355022417322,41.5979213056804,-16.122924842068));
#57466=CARTESIAN_POINT('Ctrl Pts',(-3.43590630737669,41.5159732371528,-16.3450174403968));
#57467=CARTESIAN_POINT('Ctrl Pts',(-3.73118318182571,41.7106906886745,-16.0726003938663));
#57468=CARTESIAN_POINT('Ctrl Pts',(-3.52696370022908,41.5752492629553,-16.1200082324879));
#57469=CARTESIAN_POINT('Ctrl Pts',(-3.44931758085173,41.493857071485,-16.3428152733996));
#57470=CARTESIAN_POINT('Ctrl Pts',(-3.77365910783509,41.6404628298273,-16.0627003448006));
#57471=CARTESIAN_POINT('Ctrl Pts',(-3.56674649451528,41.5069837011863,-16.1113077604514));
#57472=CARTESIAN_POINT('Ctrl Pts',(-3.48910219450987,41.427285026544,-16.3362710369363));
#57473=CARTESIAN_POINT('Ctrl Pts',(-3.80133703055952,41.5933354841588,-16.0561704793561));
#57474=CARTESIAN_POINT('Ctrl Pts',(-3.59262873818026,41.4611883744804,-16.105579589636));
#57475=CARTESIAN_POINT('Ctrl Pts',(-3.51502641995466,41.3826056395206,-16.3319912551902));
#57476=CARTESIAN_POINT('Ctrl Pts',(-3.93661737229858,41.3561924516797,-16.0239016028219));
#57477=CARTESIAN_POINT('Ctrl Pts',(-3.71926534359318,41.2302267666986,-16.0772522172006));
#57478=CARTESIAN_POINT('Ctrl Pts',(-3.64173527925152,41.1577530499255,-16.3110349773682));
#57479=CARTESIAN_POINT('Ctrl Pts',(-4.03491747293985,41.1616690216634,-15.9993106710039));
#57480=CARTESIAN_POINT('Ctrl Pts',(-3.8105351856191,41.0410889990247,-16.0558581848326));
#57481=CARTESIAN_POINT('Ctrl Pts',(-3.73380699989436,40.9732232360452,-16.2956924811267));
#57482=CARTESIAN_POINT('Ctrl Pts',(-4.21346560575097,40.7637707951905,-15.9532193788555));
#57483=CARTESIAN_POINT('Ctrl Pts',(-3.97517918815052,40.6545075845859,-16.0161173849287));
#57484=CARTESIAN_POINT('Ctrl Pts',(-3.90104216471963,40.5955698374873,-16.2684493117706));
#57485=CARTESIAN_POINT('Ctrl Pts',(-4.29370773194948,40.5603934046897,-15.9317175178876));
#57486=CARTESIAN_POINT('Ctrl Pts',(-4.04850396862992,40.4567958249106,-15.9977704901831));
#57487=CARTESIAN_POINT('Ctrl Pts',(-3.97620007983221,40.4024438484038,-16.2565472800635));
#57488=CARTESIAN_POINT('Ctrl Pts',(-4.40146481480481,40.2490824569658,-15.9021537778166));
#57489=CARTESIAN_POINT('Ctrl Pts',(-4.14571728004939,40.1550827275247,-15.9729333571334));
#57490=CARTESIAN_POINT('Ctrl Pts',(-4.0771295784449,40.1066679258703,-16.2416226946648));
#57491=CARTESIAN_POINT('Ctrl Pts',(-4.43527916848801,40.1442697315678,-15.8927463879809));
#57492=CARTESIAN_POINT('Ctrl Pts',(-4.17607991924084,40.0532812588022,-15.965075967575));
#57493=CARTESIAN_POINT('Ctrl Pts',(-4.10880142516048,40.007059981848,-16.2371350135424));
#57494=CARTESIAN_POINT('Ctrl Pts',(-4.47498970331547,40.0119814226891,-15.8815784864466));
#57495=CARTESIAN_POINT('Ctrl Pts',(-4.21141132770978,39.9250565429304,-15.955847181276));
#57496=CARTESIAN_POINT('Ctrl Pts',(-4.14599586533176,39.8813077925278,-16.2321648104482));
#57497=CARTESIAN_POINT('Ctrl Pts',(-4.48280713505993,39.9854484820733,-15.8793735332333));
#57498=CARTESIAN_POINT('Ctrl Pts',(-4.21836394867178,39.8992957517518,-15.9540264515764));
#57499=CARTESIAN_POINT('Ctrl Pts',(-4.15331797782398,39.8560841569777,-16.2312023454786));
#57500=CARTESIAN_POINT('Ctrl Pts',(-4.49815720553132,39.9323631382508,-15.8750321376815));
#57501=CARTESIAN_POINT('Ctrl Pts',(-4.23198682506552,39.8477579670653,-15.9504505711255));
#57502=CARTESIAN_POINT('Ctrl Pts',(-4.16769545413477,39.805615099322,-16.2293456787121));
#57503=CARTESIAN_POINT('Ctrl Pts',(-4.50569299128003,39.9058006819841,-15.8728948158664));
#57504=CARTESIAN_POINT('Ctrl Pts',(-4.23865969846769,39.8219707212385,-15.9486947308374));
#57505=CARTESIAN_POINT('Ctrl Pts',(-4.1747537660165,39.7803601224423,-16.2284510688984));
#57506=CARTESIAN_POINT('Ctrl Pts',(-4.52788908225558,39.8260548181995,-15.8665830325155));
#57507=CARTESIAN_POINT('Ctrl Pts',(-4.25828083324603,39.7445109973632,-15.9435203785516));
#57508=CARTESIAN_POINT('Ctrl Pts',(-4.19554349286319,39.7045346637349,-16.2258684245472));
#57509=CARTESIAN_POINT('Ctrl Pts',(-4.54213820519509,39.7728129265089,-15.8625087615832));
#57510=CARTESIAN_POINT('Ctrl Pts',(-4.27080745248769,39.6928283677743,-15.9402013833087));
#57511=CARTESIAN_POINT('Ctrl Pts',(-4.20888977911923,39.6539036641976,-16.2242815829051));
#57512=CARTESIAN_POINT('Ctrl Pts',(-4.61072350551952,39.5062243012366,-15.8428055513534));
#57513=CARTESIAN_POINT('Ctrl Pts',(-4.33101064476337,39.4331423066517,-15.9241892497505));
#57514=CARTESIAN_POINT('Ctrl Pts',(-4.27312945361112,39.4003554433727,-16.2170217104017));
#57515=CARTESIAN_POINT('Ctrl Pts',(-4.65710151667135,39.2917430094221,-15.8291830985343));
#57516=CARTESIAN_POINT('Ctrl Pts',(-4.37047377111817,39.2249262086857,-15.9134966630587));
#57517=CARTESIAN_POINT('Ctrl Pts',(-4.3165689141374,39.1962612675561,-16.2133735716419));
#57518=CARTESIAN_POINT('Ctrl Pts',(-4.73455890330831,38.860584008785,-15.8061881582692));
#57519=CARTESIAN_POINT('Ctrl Pts',(-4.43416228480996,38.806836206605,-15.8961542515918));
#57520=CARTESIAN_POINT('Ctrl Pts',(-4.38911853157358,38.7857773011577,-16.2103568495108));
#57521=CARTESIAN_POINT('Ctrl Pts',(-4.7656335172996,38.6439056908728,-15.7968150887316));
#57522=CARTESIAN_POINT('Ctrl Pts',(-4.45824992940577,38.596715083291,-15.8895386759589));
#57523=CARTESIAN_POINT('Ctrl Pts',(-4.41822423140701,38.5793869570085,-16.2109877211159));
#57524=CARTESIAN_POINT('Ctrl Pts',(-4.81366277021719,38.2085119119448,-15.7822457370113));
#57525=CARTESIAN_POINT('Ctrl Pts',(-4.49228715046657,38.1750784013236,-15.8802583836643));
#57526=CARTESIAN_POINT('Ctrl Pts',(-4.46321030786492,38.1644661155498,-16.2164498115114));
#57527=CARTESIAN_POINT('Ctrl Pts',(-4.83061473177268,37.989796110882,-15.7770490650161));
#57528=CARTESIAN_POINT('Ctrl Pts',(-4.50207912059962,37.963297937123,-15.8776364690345));
#57529=CARTESIAN_POINT('Ctrl Pts',(-4.47908817873774,37.9559353121758,-16.2212806621887));
#57530=CARTESIAN_POINT('Ctrl Pts',(-4.85119740418559,37.5504372754616,-15.7707323746352));
#57531=CARTESIAN_POINT('Ctrl Pts',(-4.50825772146479,37.5385831425256,-15.8762196986871));
#57532=CARTESIAN_POINT('Ctrl Pts',(-4.49836671444632,37.5368431558517,-16.2350392361057));
#57533=CARTESIAN_POINT('Ctrl Pts',(-4.85482680237322,37.3297940775806,-15.7696120833341));
#57534=CARTESIAN_POINT('Ctrl Pts',(-4.50446088793284,37.3253626831583,-15.8774765117451));
#57535=CARTESIAN_POINT('Ctrl Pts',(-4.50176615109278,37.3262816596819,-16.2439666982713));
#57536=CARTESIAN_POINT('Ctrl Pts',(-4.85133542686646,37.0528279294366,-15.7706862599499));
#57537=CARTESIAN_POINT('Ctrl Pts',(-4.49167305004904,37.059789020437,-15.8813246755956));
#57538=CARTESIAN_POINT('Ctrl Pts',(-4.49849599207902,37.0618545761177,-16.2576124902641));
#57539=CARTESIAN_POINT('Ctrl Pts',(-4.85023355700303,36.9973424024009,-15.7710252327459));
#57540=CARTESIAN_POINT('Ctrl Pts',(-4.4886839703737,37.0062991010676,-15.8822165992224));
#57541=CARTESIAN_POINT('Ctrl Pts',(-4.49746393778067,37.0088752437307,-16.2604679296177));
#57542=CARTESIAN_POINT('Ctrl Pts',(-4.84724165567112,36.8866091092228,-15.7719450538262));
#57543=CARTESIAN_POINT('Ctrl Pts',(-4.48191083668474,36.8995910435531,-15.884223449632));
#57544=CARTESIAN_POINT('Ctrl Pts',(-4.49466160577087,36.9031322050459,-16.2664058785488));
#57545=CARTESIAN_POINT('Ctrl Pts',(-4.84535166014932,36.8313248270939,-15.7725258903161));
#57546=CARTESIAN_POINT('Ctrl Pts',(-4.47812221634299,36.846334338376,-15.8853396943));
#57547=CARTESIAN_POINT('Ctrl Pts',(-4.49289136220764,36.8503336431165,-16.2694900363544));
#57548=CARTESIAN_POINT('Ctrl Pts',(-4.83852205833163,36.6657142912634,-15.7746228790373));
#57549=CARTESIAN_POINT('Ctrl Pts',(-4.46555605276301,36.6865436945369,-15.8890228148251));
#57550=CARTESIAN_POINT('Ctrl Pts',(-4.48649448972876,36.6921526528426,-16.2790801157266));
#57551=CARTESIAN_POINT('Ctrl Pts',(-4.83242355820479,36.5556302061425,-15.7764934506682));
#57552=CARTESIAN_POINT('Ctrl Pts',(-4.45560823761615,36.5806099310771,-15.8919151266673));
#57553=CARTESIAN_POINT('Ctrl Pts',(-4.48078239625453,36.5869847872263,-16.2859235908837));
#57554=CARTESIAN_POINT('Ctrl Pts',(-4.80964445731595,36.2263139098162,-15.7834588216173));
#57555=CARTESIAN_POINT('Ctrl Pts',(-4.42108305755237,36.2626839420804,-15.9018687747033));
#57556=CARTESIAN_POINT('Ctrl Pts',(-4.45944659885922,36.2723112115469,-16.3077427542653));
#57557=CARTESIAN_POINT('Ctrl Pts',(-4.78849025521988,36.0080156926272,-15.7899064986773));
#57558=CARTESIAN_POINT('Ctrl Pts',(-4.39194405386607,36.0530811161892,-15.9101712621084));
#57559=CARTESIAN_POINT('Ctrl Pts',(-4.43963274611102,36.0636336832212,-16.3240065044515));
#57560=CARTESIAN_POINT('Ctrl Pts',(-4.73479895287024,35.5737873220669,-15.806089492256));
#57561=CARTESIAN_POINT('Ctrl Pts',(-4.32221309888832,35.6372576288513,-15.9296899223679));
#57562=CARTESIAN_POINT('Ctrl Pts',(-4.38934337165934,35.6483850846731,-16.3596596636497));
#57563=CARTESIAN_POINT('Ctrl Pts',(-4.70226083470289,35.3578573765994,-15.8158250321208));
#57564=CARTESIAN_POINT('Ctrl Pts',(-4.28136065754713,35.4308416469974,-15.9409730418437));
#57565=CARTESIAN_POINT('Ctrl Pts',(-4.35886689759704,35.4418142023149,-16.3790492831481));
#57566=CARTESIAN_POINT('Ctrl Pts',(-4.62604323000226,34.9283028530584,-15.838285969081));
#57567=CARTESIAN_POINT('Ctrl Pts',(-4.18843254356921,35.0215742894843,-15.9661140402609));
#57568=CARTESIAN_POINT('Ctrl Pts',(-4.28747850736095,35.030732994809,-16.4206641704048));
#57569=CARTESIAN_POINT('Ctrl Pts',(-4.58236381820235,34.7146782724582,-15.851011583154));
#57570=CARTESIAN_POINT('Ctrl Pts',(-4.13606020425487,34.8185183918786,-15.9800423530578));
#57571=CARTESIAN_POINT('Ctrl Pts',(-4.24656666166447,34.8262226570115,-16.4428896521688));
#57572=CARTESIAN_POINT('Ctrl Pts',(-4.48381152977406,34.2897290978801,-15.8791706501668));
#57573=CARTESIAN_POINT('Ctrl Pts',(-4.02005922178393,34.4162818436401,-16.0101335970749));
#57574=CARTESIAN_POINT('Ctrl Pts',(-4.15425873313437,34.4192706098088,-16.489899151371));
#57575=CARTESIAN_POINT('Ctrl Pts',(-4.42893989399129,34.0784042783794,-15.8946043422336));
#57576=CARTESIAN_POINT('Ctrl Pts',(-3.95608545255841,34.2168878693719,-16.0263702668423));
#57577=CARTESIAN_POINT('Ctrl Pts',(-4.10286381244933,34.2168286739799,-16.5146834150258));
#57578=CARTESIAN_POINT('Ctrl Pts',(-4.30763827259879,33.6581098781651,-15.9279065885377));
#57579=CARTESIAN_POINT('Ctrl Pts',(-3.81658438476888,33.822448010845,-16.0607242667002));
#57580=CARTESIAN_POINT('Ctrl Pts',(-3.9892479689298,33.814078955275,-16.5665395015097));
#57581=CARTESIAN_POINT('Ctrl Pts',(-4.24121110891681,33.4491397713452,-15.9457754442683));
#57582=CARTESIAN_POINT('Ctrl Pts',(-3.7406469800499,33.6271818424222,-16.0789181512321));
#57583=CARTESIAN_POINT('Ctrl Pts',(-3.92702968859027,33.6137706563386,-16.593611645947));
#57584=CARTESIAN_POINT('Ctrl Pts',(-4.15956467569048,33.2154445308089,-15.9670945891216));
#57585=CARTESIAN_POINT('Ctrl Pts',(-3.64949552390511,33.4129433397945,-16.0999721147917));
#57586=CARTESIAN_POINT('Ctrl Pts',(-3.8505564455756,33.3896995093833,-16.6252009188576));
#57587=CARTESIAN_POINT('Ctrl Pts',(-4.15039805956273,33.189502508749,-15.9694798681321));
#57588=CARTESIAN_POINT('Ctrl Pts',(-3.63914933651993,33.3888967259962,-16.102351301209));
#57589=CARTESIAN_POINT('Ctrl Pts',(-3.84197063429969,33.3648249628758,-16.6287259546484));
#57590=CARTESIAN_POINT('Ctrl Pts',(-4.13189835567043,33.1377349934672,-15.9742764246118));
#57591=CARTESIAN_POINT('Ctrl Pts',(-3.61829077577786,33.3409526006064,-16.1071260478771));
#57592=CARTESIAN_POINT('Ctrl Pts',(-3.82464308795729,33.3151858843453,-16.635796298032));
#57593=CARTESIAN_POINT('Ctrl Pts',(-4.12256202229053,33.111900164225,-15.9766885508706));
#57594=CARTESIAN_POINT('Ctrl Pts',(-3.60777388976757,33.3170463264599,-16.1095225753306));
#57595=CARTESIAN_POINT('Ctrl Pts',(-3.81589831288601,33.2904124009369,-16.6393428649039));
#57596=CARTESIAN_POINT('Ctrl Pts',(-4.09429258351795,33.0345428662843,-15.9839653076811));
#57597=CARTESIAN_POINT('Ctrl Pts',(-3.57590653652943,33.2454014404084,-16.1167504752498));
#57598=CARTESIAN_POINT('Ctrl Pts',(-3.78942005068434,33.2162305590499,-16.6500155854832));
#57599=CARTESIAN_POINT('Ctrl Pts',(-4.07509908358835,32.9831675632239,-15.9888703159868));
#57600=CARTESIAN_POINT('Ctrl Pts',(-3.55434588845088,33.1979873053765,-16.1215955300393));
#57601=CARTESIAN_POINT('Ctrl Pts',(-3.77144266781143,33.1669607859179,-16.6571747604242));
#57602=CARTESIAN_POINT('Ctrl Pts',(-4.01646745258513,32.829634429189,-16.0037375413478));
#57603=CARTESIAN_POINT('Ctrl Pts',(-3.48838399516754,33.0560510137945,-16.1362734133368));
#57604=CARTESIAN_POINT('Ctrl Pts',(-3.71652598867197,33.0197101694359,-16.6787750251782));
#57605=CARTESIAN_POINT('Ctrl Pts',(-3.9759789438393,32.728068962807,-16.0138519706474));
#57606=CARTESIAN_POINT('Ctrl Pts',(-3.44313323859855,32.9628501297851,-16.1461489724732));
#57607=CARTESIAN_POINT('Ctrl Pts',(-3.67860286745824,32.9222876367011,-16.6933388861798));
#57608=CARTESIAN_POINT('Ctrl Pts',(-3.85020901317665,32.4257893774983,-16.0447294945566));
#57609=CARTESIAN_POINT('Ctrl Pts',(-3.30213588601185,32.6845768004043,-16.1762600178974));
#57610=CARTESIAN_POINT('Ctrl Pts',(-3.56080183062287,32.6323019776143,-16.7374460185429));
#57611=CARTESIAN_POINT('Ctrl Pts',(-3.76063777621999,32.2274841877532,-16.0660275892435));
#57612=CARTESIAN_POINT('Ctrl Pts',(-3.20289234856102,32.5050107524786,-16.1965656821621));
#57613=CARTESIAN_POINT('Ctrl Pts',(-3.47690590589959,32.4420132288924,-16.767405951522));
#57614=CARTESIAN_POINT('Ctrl Pts',(-3.56918607340305,31.8377243308601,-16.1096415154308));
#57615=CARTESIAN_POINT('Ctrl Pts',(-2.99311023840048,32.1562009537945,-16.2372785343144));
#57616=CARTESIAN_POINT('Ctrl Pts',(-3.29758475214954,32.0679272033942,-16.8280153427249));
#57617=CARTESIAN_POINT('Ctrl Pts',(-3.46731167512559,31.6462664711462,-16.1319583909726));
#57618=CARTESIAN_POINT('Ctrl Pts',(-2.88201843494523,31.9870356344035,-16.2577213825395));
#57619=CARTESIAN_POINT('Ctrl Pts',(-3.20216520503585,31.8841268311116,-16.8586659752245));
#57620=CARTESIAN_POINT('Ctrl Pts',(-3.24986431304015,31.2709079333655,-16.1771664307246));
#57621=CARTESIAN_POINT('Ctrl Pts',(-2.6480156494036,31.6607525771679,-16.2980633785119));
#57622=CARTESIAN_POINT('Ctrl Pts',(-2.99849550013316,31.5237128636391,-16.9201885252478));
#57623=CARTESIAN_POINT('Ctrl Pts',(-3.13430309790084,31.087001037092,-16.2000593106867));
#57624=CARTESIAN_POINT('Ctrl Pts',(-2.52446501017816,31.5038249498316,-16.3179747703128));
#57625=CARTESIAN_POINT('Ctrl Pts',(-2.89025634469189,31.3470932540427,-16.9510624162517));
#57626=CARTESIAN_POINT('Ctrl Pts',(-2.97992813214864,30.8625464320075,-16.2287095736517));
#57627=CARTESIAN_POINT('Ctrl Pts',(-2.36471133653988,31.3195585189969,-16.3416730253026));
#57628=CARTESIAN_POINT('Ctrl Pts',(-2.74566271341961,31.1314993826496,-16.9894416021804));
#57629=CARTESIAN_POINT('Ctrl Pts',(-2.94855445916935,30.817928300523,-16.2344410657162));
#57630=CARTESIAN_POINT('Ctrl Pts',(-2.33186814409271,31.2826216760433,-16.3464413005094));
#57631=CARTESIAN_POINT('Ctrl Pts',(-2.71627690378355,31.0886409312827,-16.9971064561535));
#57632=CARTESIAN_POINT('Ctrl Pts',(-2.88476410492296,30.7292614499473,-16.2458975182613));
#57633=CARTESIAN_POINT('Ctrl Pts',(-2.26536475661494,31.2097212908695,-16.3558796919869));
#57634=CARTESIAN_POINT('Ctrl Pts',(-2.65652836285939,31.0034678637871,-17.0124038567864));
#57635=CARTESIAN_POINT('Ctrl Pts',(-2.85231509096079,30.6851711096193,-16.2516279588096));
#57636=CARTESIAN_POINT('Ctrl Pts',(-2.23166075706606,31.1737321819387,-16.3605534424715));
#57637=CARTESIAN_POINT('Ctrl Pts',(-2.62613534683824,30.9611132622823,-17.0200436860762));
#57638=CARTESIAN_POINT('Ctrl Pts',(-2.75371586507387,30.5543032513299,-16.2687276605509));
#57639=CARTESIAN_POINT('Ctrl Pts',(-2.12916708502008,31.0671513308951,-16.3744245592637));
#57640=CARTESIAN_POINT('Ctrl Pts',(-2.53378345502449,30.8353931303199,-17.0428092866419));
#57641=CARTESIAN_POINT('Ctrl Pts',(-2.68624145339725,30.4688168020419,-16.280019596665));
#57642=CARTESIAN_POINT('Ctrl Pts',(-2.05994523352376,30.9990432166992,-16.3833298319653));
#57643=CARTESIAN_POINT('Ctrl Pts',(-2.47058428125334,30.7532636055963,-17.057800327605));
#57644=CARTESIAN_POINT('Ctrl Pts',(-2.54757388740944,30.3015880840125,-16.3022942711121));
#57645=CARTESIAN_POINT('Ctrl Pts',(-1.9192454319902,30.8681341748231,-16.4004596153518));
#57646=CARTESIAN_POINT('Ctrl Pts',(-2.34070281481905,30.5925930259895,-17.0873081301815));
#57647=CARTESIAN_POINT('Ctrl Pts',(-2.476381206771,30.2198453486412,-16.3132771209141));
#57648=CARTESIAN_POINT('Ctrl Pts',(-1.84771884517628,30.8054525230851,-16.4086687974615));
#57649=CARTESIAN_POINT('Ctrl Pts',(-2.27402096482143,30.5140515215888,-17.1018250250437));
#57650=CARTESIAN_POINT('Ctrl Pts',(-2.32998205788182,30.0603897553416,-16.334829595528));
#57651=CARTESIAN_POINT('Ctrl Pts',(-1.70258673578777,30.6857855527938,-16.4242870257666));
#57652=CARTESIAN_POINT('Ctrl Pts',(-2.13689779545945,30.3608345647763,-17.1302692409457));
#57653=CARTESIAN_POINT('Ctrl Pts',(-2.25477627281575,29.982676223402,-16.345399374049));
#57654=CARTESIAN_POINT('Ctrl Pts',(-1.62894510471729,30.6289401059803,-16.4316764817347));
#57655=CARTESIAN_POINT('Ctrl Pts',(-2.06645711480206,30.2861584632619,-17.1441967467396));
#57656=CARTESIAN_POINT('Ctrl Pts',(-2.09997874346892,29.831641210054,-16.3660070272072));
#57657=CARTESIAN_POINT('Ctrl Pts',(-1.47982485477628,30.5213540438189,-16.4455349971866));
#57658=CARTESIAN_POINT('Ctrl Pts',(-1.92146769383922,30.1410235804603,-17.1713290042148));
#57659=CARTESIAN_POINT('Ctrl Pts',(-2.02038800914664,29.7583187312675,-16.3760451220302));
#57660=CARTESIAN_POINT('Ctrl Pts',(-1.40432964804446,30.4707756283822,-16.4519799689631));
#57661=CARTESIAN_POINT('Ctrl Pts',(-1.84691989810708,30.0705638387238,-17.1845340213945));
#57662=CARTESIAN_POINT('Ctrl Pts',(-1.89735688368434,29.6519763755937,-16.3905992032782));
#57663=CARTESIAN_POINT('Ctrl Pts',(-1.29061421420031,30.4002010119293,-16.4608187862555));
#57664=CARTESIAN_POINT('Ctrl Pts',(-1.73168413361204,29.9683736297906,-17.2036812816511));
#57665=CARTESIAN_POINT('Ctrl Pts',(-1.855738117802,29.6171366953533,-16.3953665421613));
#57666=CARTESIAN_POINT('Ctrl Pts',(-1.25230151783671,30.3773864795662,-16.4636476099762));
#57667=CARTESIAN_POINT('Ctrl Pts',(-1.69270236914862,29.9348943080071,-17.2099534441512));
#57668=CARTESIAN_POINT('Ctrl Pts',(-1.79234339952953,29.5658416895116,-16.4023765699238));
#57669=CARTESIAN_POINT('Ctrl Pts',(-1.19475183342288,30.3445305772294,-16.4676726412067));
#57670=CARTESIAN_POINT('Ctrl Pts',(-1.63332439632481,29.8856025996842,-17.2191791942467));
#57671=CARTESIAN_POINT('Ctrl Pts',(-1.77105066057652,29.5489041771658,-16.4046897342604));
#57672=CARTESIAN_POINT('Ctrl Pts',(-1.17547199819176,30.333762872091,-16.4689831252204));
#57673=CARTESIAN_POINT('Ctrl Pts',(-1.6133807839376,29.8693266444902,-17.2222240118077));
#57674=CARTESIAN_POINT('Ctrl Pts',(-1.72813291087157,29.5153605402291,-16.409266356606));
#57675=CARTESIAN_POINT('Ctrl Pts',(-1.13683610528857,30.3126589001511,-16.4715332981359));
#57676=CARTESIAN_POINT('Ctrl Pts',(-1.57318234083472,29.8370933859026,-17.2282496978405));
#57677=CARTESIAN_POINT('Ctrl Pts',(-1.70649633572161,29.4987461608599,-16.4115309334004));
#57678=CARTESIAN_POINT('Ctrl Pts',(-1.11747086839056,30.3023210014394,-16.4727730500227));
#57679=CARTESIAN_POINT('Ctrl Pts',(-1.5529166780537,29.8211281512158,-17.231232043014));
#57680=CARTESIAN_POINT('Ctrl Pts',(-1.59782880094616,29.416805054283,-16.4226849288261));
#57681=CARTESIAN_POINT('Ctrl Pts',(-1.01994827144306,30.2514460679374,-16.4788242146341));
#57682=CARTESIAN_POINT('Ctrl Pts',(-1.45113441423997,29.7423892766781,-17.2459262700218));
#57683=CARTESIAN_POINT('Ctrl Pts',(-1.50908967345445,29.3546606084382,-16.4310964828382));
#57684=CARTESIAN_POINT('Ctrl Pts',(-0.94294827805055,30.2151476418465,-16.4829741135679));
#57685=CARTESIAN_POINT('Ctrl Pts',(-1.36801787580905,29.6826756493925,-17.2570235387147));
#57686=CARTESIAN_POINT('Ctrl Pts',(-1.32773854032885,29.2376739642212,-16.446744165317));
#57687=CARTESIAN_POINT('Ctrl Pts',(-0.789958819385205,30.1499851126795,
-16.4900488930594));
#57688=CARTESIAN_POINT('Ctrl Pts',(-1.19815731065464,29.570273767709,-17.2777301553418));
#57689=CARTESIAN_POINT('Ctrl Pts',(-1.23512712642901,29.1828306555037,-16.4539805128856));
#57690=CARTESIAN_POINT('Ctrl Pts',(-0.714148771847181,30.1213547087018,
-16.4929390217047));
#57691=CARTESIAN_POINT('Ctrl Pts',(-1.11141383725493,29.5175844450748,-17.2873397728772));
#57692=CARTESIAN_POINT('Ctrl Pts',(-1.04569979909049,29.0810615938186,-16.4671043497951));
#57693=CARTESIAN_POINT('Ctrl Pts',(-0.564018986317464,30.0710934810012,
-16.4975516672181));
#57694=CARTESIAN_POINT('Ctrl Pts',(-0.933988792708237,29.4198266340564,
-17.3048725518148));
#57695=CARTESIAN_POINT('Ctrl Pts',(-0.948884762668731,29.0341341932451,
-16.4729921490482));
#57696=CARTESIAN_POINT('Ctrl Pts',(-0.489933276919771,30.0496744036365,
-16.4992439979384));
#57697=CARTESIAN_POINT('Ctrl Pts',(-0.843308041987629,29.3747565609294,
-17.3127960973893));
#57698=CARTESIAN_POINT('Ctrl Pts',(-0.800191680576077,28.9702716007703,
-16.4806600727396));
#57699=CARTESIAN_POINT('Ctrl Pts',(-0.380586307990408,30.0223765474346,
-16.5009885630312));
#57700=CARTESIAN_POINT('Ctrl Pts',(-0.704036284927813,29.3134377089103,
-17.3232401222866));
#57701=CARTESIAN_POINT('Ctrl Pts',(-0.750048107089607,28.9500736446709,
-16.483021826383));
#57702=CARTESIAN_POINT('Ctrl Pts',(-0.344229360090164,30.014052241189,-16.5014375482369));
#57703=CARTESIAN_POINT('Ctrl Pts',(-0.657069852279363,29.2940472367443,
-17.3264809285521));
#57704=CARTESIAN_POINT('Ctrl Pts',(-0.673915805988587,28.9215008203245,
-16.486251322221));
#57705=CARTESIAN_POINT('Ctrl Pts',(-0.290130099099646,30.0026923249378,
-16.501926978582));
#57706=CARTESIAN_POINT('Ctrl Pts',(-0.585761361026588,29.2666219330869,
-17.3309558082814));
#57707=CARTESIAN_POINT('Ctrl Pts',(-0.648385485598382,28.91226401611,-16.4872756105357));
#57708=CARTESIAN_POINT('Ctrl Pts',(-0.272119298069543,29.9990851554066,
-16.5020595144662));
#57709=CARTESIAN_POINT('Ctrl Pts',(-0.561848664151634,29.2577570144913,
-17.3323830214636));
#57710=CARTESIAN_POINT('Ctrl Pts',(-0.597010216853532,28.8943818767733,
-16.4892158575437));
#57711=CARTESIAN_POINT('Ctrl Pts',(-0.2362023844278,29.9922245088925,-16.5022661141874));
#57712=CARTESIAN_POINT('Ctrl Pts',(-0.513728577814346,29.2405968337917,
-17.3351040222603));
#57713=CARTESIAN_POINT('Ctrl Pts',(-0.571233147511417,28.8857606891544,
-16.4901291611817));
#57714=CARTESIAN_POINT('Ctrl Pts',(-0.218349366931985,29.9889826962993,
-16.5023396092702));
#57715=CARTESIAN_POINT('Ctrl Pts',(-0.4895847662591,29.2323247467198,-17.3363941024547));
#57716=CARTESIAN_POINT('Ctrl Pts',(-0.442166073327688,28.8443554178395,
-16.4943979018314));
#57717=CARTESIAN_POINT('Ctrl Pts',(-0.129239837306087,29.9735906916381,
-16.5025703106399));
#57718=CARTESIAN_POINT('Ctrl Pts',(-0.368695495698975,29.1926016196164,
-17.342474342916));
#57719=CARTESIAN_POINT('Ctrl Pts',(-0.338061778022354,28.8165747708187,
-16.4968705077674));
#57720=CARTESIAN_POINT('Ctrl Pts',(-0.0605317814243137,29.9642648979254,
-16.5023091130787));
#57721=CARTESIAN_POINT('Ctrl Pts',(-0.271187340267436,29.1659679325416,
-17.3461688365462));
#57722=CARTESIAN_POINT('Ctrl Pts',(-0.128108295013126,28.7719728676628,
-16.499836683451));
#57723=CARTESIAN_POINT('Ctrl Pts',(0.074456716006171,29.94974338385,-16.5011651314723));
#57724=CARTESIAN_POINT('Ctrl Pts',(-0.0745366950826016,29.1232544765027,
-17.3511133431508));
#57725=CARTESIAN_POINT('Ctrl Pts',(-0.0222591829595038,28.755151135902,
-16.5003303276454));
#57726=CARTESIAN_POINT('Ctrl Pts',(0.140356992327616,29.9446203245694,-16.5002807332538));
#57727=CARTESIAN_POINT('Ctrl Pts',(0.0246057239760995,29.1071742509764,
-17.3523634528138));
#57728=CARTESIAN_POINT('Ctrl Pts',(0.191245793985154,28.7328543901453,-16.499236995659));
#57729=CARTESIAN_POINT('Ctrl Pts',(0.27161304708856,29.937520037568,-16.4980385051));
#57730=CARTESIAN_POINT('Ctrl Pts',(0.224582837315142,29.0859421960738,-17.3523016800784));
#57731=CARTESIAN_POINT('Ctrl Pts',(0.298901540034271,28.7273786281084,-16.4976501104633));
#57732=CARTESIAN_POINT('Ctrl Pts',(0.336593949719366,29.9355704487499,-16.496686377349));
#57733=CARTESIAN_POINT('Ctrl Pts',(0.325417420428351,29.080789649795,-17.3509899235518));
#57734=CARTESIAN_POINT('Ctrl Pts',(0.434652344247154,28.7279511908531,-16.4942964360642));
#57735=CARTESIAN_POINT('Ctrl Pts',(0.41904432966663,29.9349828888683,-16.4946901599378));
#57736=CARTESIAN_POINT('Ctrl Pts',(0.452566934002955,29.0814932456998,-17.3476656555962));
#57737=CARTESIAN_POINT('Ctrl Pts',(0.461791435185215,28.7284371115372,-16.4935588164354));
#57738=CARTESIAN_POINT('Ctrl Pts',(0.435530517342106,29.9349612139799,-16.4942766579394));
#57739=CARTESIAN_POINT('Ctrl Pts',(0.477986468216754,29.0819916232635,-17.3469181407489));
#57740=CARTESIAN_POINT('Ctrl Pts',(0.515943690984539,28.7301437164452,-16.4919536704588));
#57741=CARTESIAN_POINT('Ctrl Pts',(0.468495969700064,29.9351121018813,-16.4934206136822));
#57742=CARTESIAN_POINT('Ctrl Pts',(0.528707589352712,29.0836958274767,-17.3452619533545));
#57743=CARTESIAN_POINT('Ctrl Pts',(0.542973446398712,28.7313644483332,-16.4910857384778));
#57744=CARTESIAN_POINT('Ctrl Pts',(0.484979151558676,29.9352844403668,-16.4929780058774));
#57745=CARTESIAN_POINT('Ctrl Pts',(0.554024715635541,29.084901718379,-17.344352879355));
#57746=CARTESIAN_POINT('Ctrl Pts',(0.623924958202809,28.7361181266015,-16.4882877715005));
#57747=CARTESIAN_POINT('Ctrl Pts',(0.534479466208411,29.9361010848821,-16.4916034160629));
#57748=CARTESIAN_POINT('Ctrl Pts',(0.629847068288364,29.0895703548083,-17.3413850837553));
#57749=CARTESIAN_POINT('Ctrl Pts',(0.677708990090665,28.7407423067484,-16.4861635783227));
#57750=CARTESIAN_POINT('Ctrl Pts',(0.567561890649228,29.9370419497641,-16.490624834322));
#57751=CARTESIAN_POINT('Ctrl Pts',(0.680223296507896,29.0940838248501,-17.339085810858));
#57752=CARTESIAN_POINT('Ctrl Pts',(0.838519927256103,28.7589030127749,-16.4790291084593));
#57753=CARTESIAN_POINT('Ctrl Pts',(0.667392543733618,29.9411882626693,-16.4874678461666));
#57754=CARTESIAN_POINT('Ctrl Pts',(0.830845110920096,29.1117531657169,-17.3312437799614));
#57755=CARTESIAN_POINT('Ctrl Pts',(0.945006106505387,28.7767241011346,-16.4732571040723));
#57756=CARTESIAN_POINT('Ctrl Pts',(0.734797573094118,29.9456748746285,-16.4850736283494));
#57757=CARTESIAN_POINT('Ctrl Pts',(0.930584232001352,29.1290345185376,-17.3247571305769));
#57758=CARTESIAN_POINT('Ctrl Pts',(1.07723807457993,28.8059438373021,-16.4648188690481));
#57759=CARTESIAN_POINT('Ctrl Pts',(0.821934628374837,29.9543140629695,-16.481507158621));
#57760=CARTESIAN_POINT('Ctrl Pts',(1.05443786599453,29.1573212640841,-17.315130200981));
#57761=CARTESIAN_POINT('Ctrl Pts',(1.10366391397319,28.8121410610613,-16.4630684410996));
#57762=CARTESIAN_POINT('Ctrl Pts',(0.839404777360703,29.9561838764168,-16.4807692180936));
#57763=CARTESIAN_POINT('Ctrl Pts',(1.07918934093606,29.1633187716124,-17.3131270133982));
#57764=CARTESIAN_POINT('Ctrl Pts',(1.15632374754114,28.8252003709767,-16.4594535730141));
#57765=CARTESIAN_POINT('Ctrl Pts',(0.874521011859752,29.9602382847319,-16.4792360955938));
#57766=CARTESIAN_POINT('Ctrl Pts',(1.12851260097818,29.1759537682257,-17.3089782907615));
#57767=CARTESIAN_POINT('Ctrl Pts',(1.18250126727682,28.8320477321608,-16.4575931395356));
#57768=CARTESIAN_POINT('Ctrl Pts',(0.892123466946685,29.9624166282505,-16.4784430213444));
#57769=CARTESIAN_POINT('Ctrl Pts',(1.15303149003764,29.1825770131165,-17.3068373640129));
#57770=CARTESIAN_POINT('Ctrl Pts',(1.26059001577615,28.8535152040682,-16.4518581803553));
#57771=CARTESIAN_POINT('Ctrl Pts',(0.945006269189896,29.9694228223987,-16.4759818429639));
#57772=CARTESIAN_POINT('Ctrl Pts',(1.22617246651459,29.2033372707004,-17.3002214041692));
#57773=CARTESIAN_POINT('Ctrl Pts',(1.31205768956044,28.8690601669617,-16.4478300726312));
#57774=CARTESIAN_POINT('Ctrl Pts',(0.980523921137524,29.974736003371,-16.4742254675058));
#57775=CARTESIAN_POINT('Ctrl Pts',(1.27437910322739,29.2183642879055,-17.2955532864967));
#57776=CARTESIAN_POINT('Ctrl Pts',(1.4647831287284,28.9191944472757,-16.43517107612));
#57777=CARTESIAN_POINT('Ctrl Pts',(1.08747216242771,29.9927517710206,-16.4685881506749));
#57778=CARTESIAN_POINT('Ctrl Pts',(1.41742772376219,29.2668125837537,-17.2808247001297));
#57779=CARTESIAN_POINT('Ctrl Pts',(1.56436648530266,28.957276499474,-16.4259664459877));
#57780=CARTESIAN_POINT('Ctrl Pts',(1.15996351383399,30.0075731994565,-16.4643154615969));
#57781=CARTESIAN_POINT('Ctrl Pts',(1.51070139131698,29.3035947033487,-17.2700412085024));
#57782=CARTESIAN_POINT('Ctrl Pts',(1.75949339397493,29.0418768304825,-16.4062122131103));
#57783=CARTESIAN_POINT('Ctrl Pts',(1.30740732628336,30.0440019520787,-16.4545229469892));
#57784=CARTESIAN_POINT('Ctrl Pts',(1.69346488679426,29.385274695068,-17.246768023877));
#57785=CARTESIAN_POINT('Ctrl Pts',(1.85503603822308,29.0883970101933,-16.3956623294501));
#57786=CARTESIAN_POINT('Ctrl Pts',(1.38208746912005,30.0654311191767,-16.449040555324));
#57787=CARTESIAN_POINT('Ctrl Pts',(1.78295386512358,29.4301743920079,-17.2342779633839));
#57788=CARTESIAN_POINT('Ctrl Pts',(2.04241537792939,29.1891877116256,-16.3733759911771));
#57789=CARTESIAN_POINT('Ctrl Pts',(1.53349668675425,30.1157894070632,-16.4367176133733));
#57790=CARTESIAN_POINT('Ctrl Pts',(1.95846068444071,29.5274274114621,-17.2077786001255));
#57791=CARTESIAN_POINT('Ctrl Pts',(2.13425146341608,29.2434595083696,-16.3616393385331));
#57792=CARTESIAN_POINT('Ctrl Pts',(1.61000429268926,30.1445060379138,-16.4299192937042));
#57793=CARTESIAN_POINT('Ctrl Pts',(2.04447795482465,29.5797819581103,-17.1937690407036));
#57794=CARTESIAN_POINT('Ctrl Pts',(2.3144828178405,29.3592119103105,-16.3371184864176));
#57795=CARTESIAN_POINT('Ctrl Pts',(1.76445361782877,30.2098541291851,-16.4149279831066));
#57796=CARTESIAN_POINT('Ctrl Pts',(2.21328969153138,29.6914212472574,-17.1643920201756));
#57797=CARTESIAN_POINT('Ctrl Pts',(2.40287766710257,29.4206933906018,-16.3243341414413));
#57798=CARTESIAN_POINT('Ctrl Pts',(1.84222493333582,30.2462536617642,-16.4067789597616));
#57799=CARTESIAN_POINT('Ctrl Pts',(2.29608376542315,29.7507068302044,-17.1490243729861));
#57800=CARTESIAN_POINT('Ctrl Pts',(2.51135285252538,29.5017829309144,-16.3077769328132));
#57801=CARTESIAN_POINT('Ctrl Pts',(1.94077379223057,30.2972459914495,-16.3956391132683));
#57802=CARTESIAN_POINT('Ctrl Pts',(2.39768586735591,29.8288858890433,-17.1290549495678));
#57803=CARTESIAN_POINT('Ctrl Pts',(2.53290170127805,29.5181794566019,-16.3044434790811));
#57804=CARTESIAN_POINT('Ctrl Pts',(1.96028897303141,30.3075771594425,-16.3933941774779));
#57805=CARTESIAN_POINT('Ctrl Pts',(2.41786936214229,29.8446932300906,-17.1250312972996));
#57806=CARTESIAN_POINT('Ctrl Pts',(2.57565545767622,29.5512731693992,-16.2977442351459));
#57807=CARTESIAN_POINT('Ctrl Pts',(1.99921568638862,30.3286552806381,-16.3888383057235));
#57808=CARTESIAN_POINT('Ctrl Pts',(2.45791420271846,29.8765964221614,-17.1169385254278));
#57809=CARTESIAN_POINT('Ctrl Pts',(2.59687024481893,29.5679777347785,-16.2943769383145));
#57810=CARTESIAN_POINT('Ctrl Pts',(2.01863572271277,30.3394038774272,-16.3865268648834));
#57811=CARTESIAN_POINT('Ctrl Pts',(2.47778480237176,29.8926993859692,-17.1128675875488));
#57812=CARTESIAN_POINT('Ctrl Pts',(2.66004324798223,29.6185503436459,-16.2842251711301));
#57813=CARTESIAN_POINT('Ctrl Pts',(2.07658934638655,30.3721820016165,-16.3795138210175));
#57814=CARTESIAN_POINT('Ctrl Pts',(2.53695510817887,29.9414486673533,-17.100584863834));
#57815=CARTESIAN_POINT('Ctrl Pts',(2.70153038913429,29.6528770266069,-16.2773908679428));
#57816=CARTESIAN_POINT('Ctrl Pts',(2.11515348080612,30.3949183678539,-16.3746953336256));
#57817=CARTESIAN_POINT('Ctrl Pts',(2.57581358773611,29.9745351098867,-17.0923032197876));
#57818=CARTESIAN_POINT('Ctrl Pts',(2.82421530443451,29.7575890425693,-16.2567120771395));
#57819=CARTESIAN_POINT('Ctrl Pts',(2.22956819594977,30.4651684504852,-16.3599495397914));
#57820=CARTESIAN_POINT('Ctrl Pts',(2.69072507829928,30.0754559176024,-17.0672065911949));
#57821=CARTESIAN_POINT('Ctrl Pts',(2.90364008546083,29.8297029496513,-16.2426922301433));
#57822=CARTESIAN_POINT('Ctrl Pts',(2.30547175408465,30.5154143020214,-16.3495803497904));
#57823=CARTESIAN_POINT('Ctrl Pts',(2.7651174356246,30.1449484959329,-17.0501405710026));
#57824=CARTESIAN_POINT('Ctrl Pts',(3.05823671500216,29.9780894969754,-16.2142950763844));
#57825=CARTESIAN_POINT('Ctrl Pts',(2.45531918886263,30.6220505261989,-16.3279618812435));
#57826=CARTESIAN_POINT('Ctrl Pts',(2.90991868602117,30.2879200951006,-17.0154679498268));
#57827=CARTESIAN_POINT('Ctrl Pts',(3.13340755103014,30.0543631118974,-16.1999176059517));
#57828=CARTESIAN_POINT('Ctrl Pts',(2.52928950864992,30.6782919897607,-16.316734700869));
#57829=CARTESIAN_POINT('Ctrl Pts',(2.98032663199793,30.3614000520084,-16.9978611399441));
#57830=CARTESIAN_POINT('Ctrl Pts',(3.27987015132021,30.210715992756,-16.1709005658607));
#57831=CARTESIAN_POINT('Ctrl Pts',(2.67504196758113,30.7964541736505,-16.2935360824409));
#57832=CARTESIAN_POINT('Ctrl Pts',(3.11750923246245,30.5120049089877,-16.9622167722053));
#57833=CARTESIAN_POINT('Ctrl Pts',(3.35116123035258,30.2907959175364,-16.156260881267));
#57834=CARTESIAN_POINT('Ctrl Pts',(2.74686657696321,30.8582478680463,-16.2815815826731));
#57835=CARTESIAN_POINT('Ctrl Pts',(3.18428324621236,30.5891304417996,-16.9441790683909));
#57836=CARTESIAN_POINT('Ctrl Pts',(3.55966298596679,30.5363244595009,-16.1120758578107));
#57837=CARTESIAN_POINT('Ctrl Pts',(2.95660210195659,31.049475646984,-16.2451814165979));
#57838=CARTESIAN_POINT('Ctrl Pts',(3.37957414633138,30.8255678671554,-16.8895639888451));
#57839=CARTESIAN_POINT('Ctrl Pts',(3.69152422416695,30.7070404100115,-16.0822670185369));
#57840=CARTESIAN_POINT('Ctrl Pts',(3.0935680110286,31.188233012752,-16.2194870411642));
#57841=CARTESIAN_POINT('Ctrl Pts',(3.50308054074258,30.9899200073615,-16.8524880403649));
#57842=CARTESIAN_POINT('Ctrl Pts',(3.84850625888578,30.9282217390845,-16.0449381752436));
#57843=CARTESIAN_POINT('Ctrl Pts',(3.2607646882954,31.3759330382798,-16.1859089389379));
#57844=CARTESIAN_POINT('Ctrl Pts',(3.6501160551046,31.2027958226833,-16.8057225066586));
#57845=CARTESIAN_POINT('Ctrl Pts',(3.87953256866694,30.9728856431268,-16.0374628392411));
#57846=CARTESIAN_POINT('Ctrl Pts',(3.29342662187892,31.4134934654484,-16.1792418772485));
#57847=CARTESIAN_POINT('Ctrl Pts',(3.67917651069663,31.2457796337213,-16.7963405521398));
#57848=CARTESIAN_POINT('Ctrl Pts',(3.94058434545197,31.0626285007038,-16.022571026142));
#57849=CARTESIAN_POINT('Ctrl Pts',(3.35787539127852,31.4893981914476,-16.1658790869078));
#57850=CARTESIAN_POINT('Ctrl Pts',(3.73635999288582,31.3321406834297,-16.7776156643026));
#57851=CARTESIAN_POINT('Ctrl Pts',(3.97063463723664,31.1077409109996,-16.0151487999533));
#57852=CARTESIAN_POINT('Ctrl Pts',(3.38969847622929,31.5277649299416,-16.1591781972395));
#57853=CARTESIAN_POINT('Ctrl Pts',(3.76450627188365,31.3755501268062,-16.7682655550614));
#57854=CARTESIAN_POINT('Ctrl Pts',(4.05941717087094,31.2437732562028,-15.9929626480247));
#57855=CARTESIAN_POINT('Ctrl Pts',(3.48351050644036,31.6435098716445,-16.1391308660064));
#57856=CARTESIAN_POINT('Ctrl Pts',(3.84766346564603,31.5064382047407,-16.7402628285028));
#57857=CARTESIAN_POINT('Ctrl Pts',(4.1167828254897,31.3353874419429,-15.978279338896));
#57858=CARTESIAN_POINT('Ctrl Pts',(3.54479499845881,31.7226089412723,-16.1256471238317));
#57859=CARTESIAN_POINT('Ctrl Pts',(3.90139438215665,31.5945757570875,-16.7216579368768));
#57860=CARTESIAN_POINT('Ctrl Pts',(4.28380788594745,31.6128203257638,-15.9346238064299));
#57861=CARTESIAN_POINT('Ctrl Pts',(3.72231473431664,31.9620905398297,-16.0855354656462));
#57862=CARTESIAN_POINT('Ctrl Pts',(4.05783658707824,31.8614425296594,-16.6661133987202));
#57863=CARTESIAN_POINT('Ctrl Pts',(4.3884148581878,31.8012197189447,-15.9060466319014));
#57864=CARTESIAN_POINT('Ctrl Pts',(3.83587999076983,32.1288604724229,-16.0584933410282));
#57865=CARTESIAN_POINT('Ctrl Pts',(4.15581556986088,32.0426166386068,-16.6294449643945));
#57866=CARTESIAN_POINT('Ctrl Pts',(4.58567200756637,32.1841943988468,-15.8503033618542));
#57867=CARTESIAN_POINT('Ctrl Pts',(4.05086579113235,32.4720636118671,-16.0050120263636));
#57868=CARTESIAN_POINT('Ctrl Pts',(4.34057433194744,32.4107939451974,-16.5572151315481));
#57869=CARTESIAN_POINT('Ctrl Pts',(4.67831544203237,32.3787729501169,-15.8231365471297));
#57870=CARTESIAN_POINT('Ctrl Pts',(4.152839616667,32.6484592325927,-15.9785118187779));
#57871=CARTESIAN_POINT('Ctrl Pts',(4.4273477970609,32.5978002916929,-16.5216528747722));
#57872=CARTESIAN_POINT('Ctrl Pts',(4.8526074647995,32.7736749069825,-15.7705575791359));
#57873=CARTESIAN_POINT('Ctrl Pts',(4.34531777018242,33.0096063680591,-15.9266467671527));
#57874=CARTESIAN_POINT('Ctrl Pts',(4.59059652338769,32.9772145356856,-16.4519928922655));
#57875=CARTESIAN_POINT('Ctrl Pts',(4.93425250225085,32.9740000075212,-15.7451448786754));
#57876=CARTESIAN_POINT('Ctrl Pts',(4.43629332140126,33.1943793675723,-15.9012113154715));
#57877=CARTESIAN_POINT('Ctrl Pts',(4.66706845943702,33.1696240761953,-16.4178945495574));
#57878=CARTESIAN_POINT('Ctrl Pts',(5.08711281849313,33.3801631316144,-15.6964237384943));
#57879=CARTESIAN_POINT('Ctrl Pts',(4.60722078767624,33.5714101157215,-15.8519572579756));
#57880=CARTESIAN_POINT('Ctrl Pts',(4.81024341123228,33.5596069464454,-16.3515167576984));
#57881=CARTESIAN_POINT('Ctrl Pts',(5.15832642133817,33.5860019204558,-15.6731147994769));
#57882=CARTESIAN_POINT('Ctrl Pts',(4.68757869339825,33.7637237962017,-15.8280627301349));
#57883=CARTESIAN_POINT('Ctrl Pts',(4.87694485739314,33.7571810298932,-16.3192367814774));
#57884=CARTESIAN_POINT('Ctrl Pts',(5.24097629968965,33.8467036990582,-15.6455255940079));
#57885=CARTESIAN_POINT('Ctrl Pts',(4.78213072770676,34.0107071083605,-15.7992314731343));
#57886=CARTESIAN_POINT('Ctrl Pts',(4.95435796666611,34.0073247840893,-16.2802535152582));
#57887=CARTESIAN_POINT('Ctrl Pts',(5.25719362818707,33.8990359684241,-15.6400829974654));
#57888=CARTESIAN_POINT('Ctrl Pts',(4.80054957120818,34.0598870173825,-15.793578275618));
#57889=CARTESIAN_POINT('Ctrl Pts',(4.96954775094229,34.0575332013725,-16.2725221393888));
#57890=CARTESIAN_POINT('Ctrl Pts',(5.28896226944923,34.0039467757404,-15.6293684812982));
#57891=CARTESIAN_POINT('Ctrl Pts',(4.83669604861666,34.1585897884646,-15.7824156043202));
#57892=CARTESIAN_POINT('Ctrl Pts',(4.99930350304212,34.1581771173989,-16.2572160497018));
#57893=CARTESIAN_POINT('Ctrl Pts',(5.30449626492683,34.0564670383293,-15.624102431784));
#57894=CARTESIAN_POINT('Ctrl Pts',(4.85440974566674,34.2080603224636,-15.7769108872987));
#57895=CARTESIAN_POINT('Ctrl Pts',(5.0138532509136,34.208556714705,-16.2496497575703));
#57896=CARTESIAN_POINT('Ctrl Pts',(5.3500593030389,34.2142207349753,-15.6085840212356));
#57897=CARTESIAN_POINT('Ctrl Pts',(4.90631386646526,34.3563731632076,-15.7606865923713));
#57898=CARTESIAN_POINT('Ctrl Pts',(5.05652937471128,34.3598665463188,-16.2272172272366));
#57899=CARTESIAN_POINT('Ctrl Pts',(5.37905002720047,34.3196469683343,-15.598611350614));
#57900=CARTESIAN_POINT('Ctrl Pts',(4.9396069834735,34.4560073796611,-15.7501529654412));
#57901=CARTESIAN_POINT('Ctrl Pts',(5.08368322108408,34.460967717809,-16.2126172924642));
#57902=CARTESIAN_POINT('Ctrl Pts',(5.46194078461707,34.6366877503115,-15.569862681342));
#57903=CARTESIAN_POINT('Ctrl Pts',(5.03466043352864,34.7544911380799,-15.7197631997284));
#57904=CARTESIAN_POINT('Ctrl Pts',(5.16132194699471,34.7649439115857,-16.1699328633975));
#57905=CARTESIAN_POINT('Ctrl Pts',(5.51176846617966,34.8490627904254,-15.5522551143952));
#57906=CARTESIAN_POINT('Ctrl Pts',(5.09291260313501,34.9564096240105,-15.7007118502892));
#57907=CARTESIAN_POINT('Ctrl Pts',(5.2079925027011,34.968490137579,-16.1429629194519));
#57908=CARTESIAN_POINT('Ctrl Pts',(5.60071361456991,35.275833071767,-15.5204457982229));
#57909=CARTESIAN_POINT('Ctrl Pts',(5.19800485837501,35.3631027727456,-15.6657772117967));
#57910=CARTESIAN_POINT('Ctrl Pts',(5.29130200819381,35.3773514622423,-16.0922807281473));
#57911=CARTESIAN_POINT('Ctrl Pts',(5.63983069135891,35.4902283652519,-15.5062438204224));
#57912=CARTESIAN_POINT('Ctrl Pts',(5.24514293116004,35.5680932299173,-15.649807466499));
#57913=CARTESIAN_POINT('Ctrl Pts',(5.32794059231136,35.5826666215459,-16.0685682530086));
#57914=CARTESIAN_POINT('Ctrl Pts',(5.70722219029865,35.9210809846202,-15.4815665394735));
#57915=CARTESIAN_POINT('Ctrl Pts',(5.32796042195972,35.9807456339375,-15.6213886714218));
#57916=CARTESIAN_POINT('Ctrl Pts',(5.39106210676183,35.9950907162295,-16.0247146511509));
#57917=CARTESIAN_POINT('Ctrl Pts',(5.73549725525296,36.1375381840345,-15.4710909455289));
#57918=CARTESIAN_POINT('Ctrl Pts',(5.36389926796403,36.1886130621991,-15.6088583771076));
#57919=CARTESIAN_POINT('Ctrl Pts',(5.41754563828522,36.2021995446388,-16.004573243818));
#57920=CARTESIAN_POINT('Ctrl Pts',(5.78078346060784,36.5726077638088,-15.4542268131215));
#57921=CARTESIAN_POINT('Ctrl Pts',(5.42398393004534,36.606935192749,-15.5876972584938));
#57922=CARTESIAN_POINT('Ctrl Pts',(5.45996247023453,36.6182830146743,-15.9682119674733));
#57923=CARTESIAN_POINT('Ctrl Pts',(5.7977963957715,36.7912198164816,-15.4478378834369));
#57924=CARTESIAN_POINT('Ctrl Pts',(5.44836047329696,36.8175859984048,-15.5789899469686));
#57925=CARTESIAN_POINT('Ctrl Pts',(5.47589745022953,36.8272573619824,-15.9519917284049));
#57926=CARTESIAN_POINT('Ctrl Pts',(5.81430843554853,37.1208676336436,-15.4416272457358));
#57927=CARTESIAN_POINT('Ctrl Pts',(5.47569053932407,37.1367087944884,-15.5691295274642));
#57928=CARTESIAN_POINT('Ctrl Pts',(5.49136327314324,37.1422120437367,-15.9308997542));
#57929=CARTESIAN_POINT('Ctrl Pts',(5.81830852011158,37.2310390122662,-15.4401195822918));
#57930=CARTESIAN_POINT('Ctrl Pts',(5.48324669152352,37.243039155561,-15.5663815273683));
#57931=CARTESIAN_POINT('Ctrl Pts',(5.49510990843326,37.2474462392647,-15.924409220868));
#57932=CARTESIAN_POINT('Ctrl Pts',(5.8219552680468,37.3967483415922,-15.4387447204924));
#57933=CARTESIAN_POINT('Ctrl Pts',(5.49218973652234,37.4033363287178,-15.5630995045285));
#57934=CARTESIAN_POINT('Ctrl Pts',(5.49852559552139,37.4056877138083,-15.9155248418178));
#57935=CARTESIAN_POINT('Ctrl Pts',(5.82277787197035,37.4520779924035,-15.4384344431652));
#57936=CARTESIAN_POINT('Ctrl Pts',(5.49476863526362,37.4567795900761,-15.5621468243714));
#57937=CARTESIAN_POINT('Ctrl Pts',(5.49929607838327,37.4585169113888,-15.9127047089119));
#57938=CARTESIAN_POINT('Ctrl Pts',(5.82361937406439,37.5625395576871,-15.438117035061));
#57939=CARTESIAN_POINT('Ctrl Pts',(5.49909810504416,37.5635003468084,-15.5605340956755));
#57940=CARTESIAN_POINT('Ctrl Pts',(5.50008426225533,37.5639723612738,-15.9073715669842));
#57941=CARTESIAN_POINT('Ctrl Pts',(5.82363950904436,37.6177133458351,-15.438109438589));
#57942=CARTESIAN_POINT('Ctrl Pts',(5.5008542982352,37.6168225419558,-15.5598720284282));
#57943=CARTESIAN_POINT('Ctrl Pts',(5.50010312136638,37.6166386057181,-15.9048561966123));
#57944=CARTESIAN_POINT('Ctrl Pts',(5.8217154307924,37.893294229626,-15.4388351940587));
#57945=CARTESIAN_POINT('Ctrl Pts',(5.50752491944064,37.881853217054,-15.5573104201885));
#57946=CARTESIAN_POINT('Ctrl Pts',(5.49830095467151,37.8796590971548,-15.8930435523112));
#57947=CARTESIAN_POINT('Ctrl Pts',(5.8137104043734,38.1128388502149,-15.4418594419708));
#57948=CARTESIAN_POINT('Ctrl Pts',(5.50636898532151,38.0944392377558,-15.5575651542258));
#57949=CARTESIAN_POINT('Ctrl Pts',(5.49080313325399,38.0890827853353,-15.886038511744));
#57950=CARTESIAN_POINT('Ctrl Pts',(5.7840049154644,38.5499825598019,-15.4530106720142));
#57951=CARTESIAN_POINT('Ctrl Pts',(5.48999166329811,38.5177567680441,-15.5630532663817));
#57952=CARTESIAN_POINT('Ctrl Pts',(5.46297981094671,38.5058340924418,-15.8771352552735));
#57953=CARTESIAN_POINT('Ctrl Pts',(5.76230703860224,38.7675819658764,-15.4611377904124));
#57954=CARTESIAN_POINT('Ctrl Pts',(5.47493356768806,38.7287614510696,-15.568229955048));
#57955=CARTESIAN_POINT('Ctrl Pts',(5.44265672992744,38.7131620074787,-15.8752371590965));
#57956=CARTESIAN_POINT('Ctrl Pts',(5.70407395336722,39.2006823460781,-15.4827163158072));
#57957=CARTESIAN_POINT('Ctrl Pts',(5.42972855746396,39.1486876692357,-15.5837780636752));
#57958=CARTESIAN_POINT('Ctrl Pts',(5.38811334519547,39.1255654423464,-15.8767726336669));
#57959=CARTESIAN_POINT('Ctrl Pts',(5.66754335828454,39.4161838894492,-15.4961678890182));
#57960=CARTESIAN_POINT('Ctrl Pts',(5.39972357971351,39.3578660216,-15.5941025574047));
#57961=CARTESIAN_POINT('Ctrl Pts',(5.35389735978674,39.3306414973316,-15.88020634219));
#57962=CARTESIAN_POINT('Ctrl Pts',(5.60039918974671,39.7377021629651,-15.5205056507883));
#57963=CARTESIAN_POINT('Ctrl Pts',(5.34213771584874,39.6706104721975,-15.6136918367253));
#57964=CARTESIAN_POINT('Ctrl Pts',(5.29100750584286,39.6364055190875,-15.8895273598811));
#57965=CARTESIAN_POINT('Ctrl Pts',(5.57595554966988,39.8445853883982,-15.5293116329089));
#57966=CARTESIAN_POINT('Ctrl Pts',(5.32093394283459,39.7743589127886,-15.6208743387635));
#57967=CARTESIAN_POINT('Ctrl Pts',(5.26811263571756,39.7380180145649,-15.8933294601772));
#57968=CARTESIAN_POINT('Ctrl Pts',(5.53599851525571,40.004450203368,-15.5435813267104));
#57969=CARTESIAN_POINT('Ctrl Pts',(5.28579906825781,39.929705256497,-15.632690927334));
#57970=CARTESIAN_POINT('Ctrl Pts',(5.23068731473301,39.8899479695032,-15.9000967087543));
#57971=CARTESIAN_POINT('Ctrl Pts',(5.5221305599358,40.0576617611033,-15.5485146750299));
#57972=CARTESIAN_POINT('Ctrl Pts',(5.27355459719845,39.9813594979742,-15.6367961486595));
#57973=CARTESIAN_POINT('Ctrl Pts',(5.2176980449392,39.9405097816184,-15.9025298069678));
#57974=CARTESIAN_POINT('Ctrl Pts',(5.50047699149048,40.1373603819414,-15.556182420383));
#57975=CARTESIAN_POINT('Ctrl Pts',(5.25432923497206,40.0587687077115,-15.6432168973992));
#57976=CARTESIAN_POINT('Ctrl Pts',(5.19741646594872,40.0162266424403,-15.9064481481372));
#57977=CARTESIAN_POINT('Ctrl Pts',(5.49311741536451,40.1639050501549,-15.5587828592327));
#57978=CARTESIAN_POINT('Ctrl Pts',(5.24778336468827,40.0845377385951,-15.6453990618431));
#57979=CARTESIAN_POINT('Ctrl Pts',(5.19052319892915,40.041442951149,-15.907799028716));
#57980=CARTESIAN_POINT('Ctrl Pts',(5.47814593729634,40.2168282263209,-15.5640605270417));
#57981=CARTESIAN_POINT('Ctrl Pts',(5.23443708951077,40.1359150171577,-15.649839332167));
#57982=CARTESIAN_POINT('Ctrl Pts',(5.17650032697911,40.0917133649177,-15.9105838634));
#57983=CARTESIAN_POINT('Ctrl Pts',(5.470529823742,40.2432224288697,-15.5667392494243));
#57984=CARTESIAN_POINT('Ctrl Pts',(5.22763310795184,40.1615391166161,-15.6520986436733));
#57985=CARTESIAN_POINT('Ctrl Pts',(5.16936677702167,40.1167823811518,-15.9120185729299));
#57986=CARTESIAN_POINT('Ctrl Pts',(5.40080286686056,40.4801601691466,-15.5912040190124));
#57987=CARTESIAN_POINT('Ctrl Pts',(5.1654386504834,40.3907259377088,-15.672707312104));
#57988=CARTESIAN_POINT('Ctrl Pts',(5.10405778192814,40.3418044912576,-15.9253090687417));
#57989=CARTESIAN_POINT('Ctrl Pts',(5.33043670111554,40.6864411445816,-15.6154875831029));
#57990=CARTESIAN_POINT('Ctrl Pts',(5.10156582395526,40.5911762940015,-15.6935809949587));
#57991=CARTESIAN_POINT('Ctrl Pts',(5.03815007775546,40.5375718116029,-15.9398148438705));
#57992=CARTESIAN_POINT('Ctrl Pts',(5.17171535959732,41.0898251595944,-15.6687704725657));
#57993=CARTESIAN_POINT('Ctrl Pts',(4.9558472522213,40.9828549133869,-15.739985220476));
#57994=CARTESIAN_POINT('Ctrl Pts',(4.88948546120424,40.9201248480408,-15.9738813871344));
#57995=CARTESIAN_POINT('Ctrl Pts',(5.08336558250042,41.2869305832741,-15.6977708167442));
#57996=CARTESIAN_POINT('Ctrl Pts',(4.87405064261176,41.1743746865059,-15.7655101753502));
#57997=CARTESIAN_POINT('Ctrl Pts',(4.80673360287453,41.1069127909073,-15.9934430495542));
#57998=CARTESIAN_POINT('Ctrl Pts',(4.88694399553687,41.671218731313,-15.7600251473423));
#57999=CARTESIAN_POINT('Ctrl Pts',(4.69092137437619,41.5474552367694,-15.8207627043341));
#58000=CARTESIAN_POINT('Ctrl Pts',(4.62275746195378,41.4708178044506,-16.0372007396695));
#58001=CARTESIAN_POINT('Ctrl Pts',(4.77888228918939,41.858405974228,-15.7932806671364));
#58002=CARTESIAN_POINT('Ctrl Pts',(4.58961749308463,41.7292760041513,-15.8504958068979));
#58003=CARTESIAN_POINT('Ctrl Pts',(4.5215426392795,41.6479391144314,-16.0613980705431));
#58004=CARTESIAN_POINT('Ctrl Pts',(4.64482519461143,42.0628061930575,-15.8327458139082));
#58005=CARTESIAN_POINT('Ctrl Pts',(4.46310917160174,41.9280541129356,-15.8860546410961));
#58006=CARTESIAN_POINT('Ctrl Pts',(4.39597952121523,41.8412001847982,-16.0909199817576));
#58007=CARTESIAN_POINT('Ctrl Pts',(4.62976965412125,42.0854096858801,-15.8371551458627));
#58008=CARTESIAN_POINT('Ctrl Pts',(4.44892446825342,41.9499886943975,-15.8900217942609));
#58009=CARTESIAN_POINT('Ctrl Pts',(4.38187791293436,41.8625697484028,-16.0942290007409));
#58010=CARTESIAN_POINT('Ctrl Pts',(4.59939878543121,42.1303067904093,-15.8460020502624));
#58011=CARTESIAN_POINT('Ctrl Pts',(4.42029652797858,41.9935550766478,-15.8979866657635));
#58012=CARTESIAN_POINT('Ctrl Pts',(4.35343136929109,41.9050117576583,-16.1008888977657));
#58013=CARTESIAN_POINT('Ctrl Pts',(4.58407427222009,42.1526144588579,-15.8504423301015));
#58014=CARTESIAN_POINT('Ctrl Pts',(4.40584455629757,42.0152010592343,-15.9019868666117));
#58015=CARTESIAN_POINT('Ctrl Pts',(4.3390778307107,41.9260974941438,-16.1042417996911));
#58016=CARTESIAN_POINT('Ctrl Pts',(4.53768208250935,42.2191142602777,-15.8638103017682));
#58017=CARTESIAN_POINT('Ctrl Pts',(4.36208642108868,42.0797067591165,-15.914033937939));
#58018=CARTESIAN_POINT('Ctrl Pts',(4.2956250910933,41.9889485291262,-16.1143660947964));
#58019=CARTESIAN_POINT('Ctrl Pts',(4.50619581303838,42.2628832431857,-15.8727851349316));
#58020=CARTESIAN_POINT('Ctrl Pts',(4.33235251838812,42.1221742523451,-15.9221344733298));
#58021=CARTESIAN_POINT('Ctrl Pts',(4.26613381932855,42.0303077037197,-16.121203084525));
#58022=CARTESIAN_POINT('Ctrl Pts',(4.41004926624052,42.3924912295783,-15.8998710702299));
#58023=CARTESIAN_POINT('Ctrl Pts',(4.24153152750805,42.2478448168248,-15.9465961576241));
#58024=CARTESIAN_POINT('Ctrl Pts',(4.1760792026318,42.1527559308387,-16.1419500461017));
#58025=CARTESIAN_POINT('Ctrl Pts',(4.34370225939985,42.4766322174293,-15.9181437877767));
#58026=CARTESIAN_POINT('Ctrl Pts',(4.17872361398144,42.3294747743511,-15.9631463234755));
#58027=CARTESIAN_POINT('Ctrl Pts',(4.11393600041315,42.2322165809747,-16.1560961451583));
#58028=CARTESIAN_POINT('Ctrl Pts',(4.13777251537753,42.7221794291726,-15.9733854419649));
#58029=CARTESIAN_POINT('Ctrl Pts',(3.98370692807761,42.5673833142134,-16.0132260504743));
#58030=CARTESIAN_POINT('Ctrl Pts',(3.92105414688791,42.4640154815466,-16.1992634768941));
#58031=CARTESIAN_POINT('Ctrl Pts',(3.99132195149594,42.8767293832158,-16.0107821043782));
#58032=CARTESIAN_POINT('Ctrl Pts',(3.84451111612512,42.7173047864165,-16.0473039779341));
#58033=CARTESIAN_POINT('Ctrl Pts',(3.78388281919657,42.6097890780496,-16.2290170151344));
#58034=CARTESIAN_POINT('Ctrl Pts',(3.75700972962784,43.0941951466418,-16.0667771043254));
#58035=CARTESIAN_POINT('Ctrl Pts',(3.62129524685035,42.9281698633173,-16.0984923203175));
#58036=CARTESIAN_POINT('Ctrl Pts',(3.56441682684187,42.8147476794126,-16.2742016702415));
#58037=CARTESIAN_POINT('Ctrl Pts',(3.67646144559015,43.1642860455141,-16.0854244903344));
#58038=CARTESIAN_POINT('Ctrl Pts',(3.54454660494019,42.9960786893441,-16.115553648241));
#58039=CARTESIAN_POINT('Ctrl Pts',(3.48897215266966,42.8807793342241,-16.2893548851606));
#58040=CARTESIAN_POINT('Ctrl Pts',(3.55180835016696,43.2656968454944,-16.1132389634261));
#58041=CARTESIAN_POINT('Ctrl Pts',(3.42566053370466,43.0943214418982,-16.1410401047175));
#58042=CARTESIAN_POINT('Ctrl Pts',(3.37221718759655,42.9762779466704,-16.3121000330166));
#58043=CARTESIAN_POINT('Ctrl Pts',(3.50961052575669,43.2988851470272,-16.122485966165));
#58044=CARTESIAN_POINT('Ctrl Pts',(3.38541262458361,43.1264600581356,-16.1495163495703));
#58045=CARTESIAN_POINT('Ctrl Pts',(3.33269305445803,43.0075246336688,-16.3196856337079));
#58046=CARTESIAN_POINT('Ctrl Pts',(3.4239361870611,43.3639679820918,-16.1408977680494));
#58047=CARTESIAN_POINT('Ctrl Pts',(3.30367271591507,43.189473362121,-16.1664034224739));
#58048=CARTESIAN_POINT('Ctrl Pts',(3.25244711732724,43.0687868973452,-16.3348347973778));
#58049=CARTESIAN_POINT('Ctrl Pts',(3.38069422093024,43.3956846955611,-16.1500121560905));
#58050=CARTESIAN_POINT('Ctrl Pts',(3.26240299114715,43.2201782549395,-16.1747684968875));
#58051=CARTESIAN_POINT('Ctrl Pts',(3.21194500033968,43.0986350973994,-16.3423568657999));
#58052=CARTESIAN_POINT('Ctrl Pts',(3.16247293665689,43.5501883769039,-16.1950777040967));
#58053=CARTESIAN_POINT('Ctrl Pts',(3.05423596689228,43.3696142664887,-16.2161210510762));
#58054=CARTESIAN_POINT('Ctrl Pts',(3.00755040891255,43.2440053764108,-16.3796546335878));
#58055=CARTESIAN_POINT('Ctrl Pts',(2.98147832252801,43.660776482398,-16.2295084233055));
#58056=CARTESIAN_POINT('Ctrl Pts',(2.88121816202138,43.4766418873115,-16.2478293654573));
#58057=CARTESIAN_POINT('Ctrl Pts',(2.83802377309921,43.3479542916528,-16.4084895185999));
#58058=CARTESIAN_POINT('Ctrl Pts',(2.70037397572554,43.8074863821001,-16.277807578224));
#58059=CARTESIAN_POINT('Ctrl Pts',(2.61232205384454,43.6184982166501,-16.2923899551782));
#58060=CARTESIAN_POINT('Ctrl Pts',(2.57473044561691,43.4857336160062,-16.4493217081974));
#58061=CARTESIAN_POINT('Ctrl Pts',(2.60506670587299,43.8531862697985,-16.2933497575293));
#58062=CARTESIAN_POINT('Ctrl Pts',(2.52114721824606,43.6626594710407,-16.3067415552332));
#58063=CARTESIAN_POINT('Ctrl Pts',(2.48546192830491,43.528628365131,-16.4625297245561));
#58064=CARTESIAN_POINT('Ctrl Pts',(2.41119452256951,43.9381353686842,-16.3231663545269));
#58065=CARTESIAN_POINT('Ctrl Pts',(2.3356478240054,43.7447042632128,-16.3342999073));
#58066=CARTESIAN_POINT('Ctrl Pts',(2.3038736575641,43.6083197721399,-16.4879921624111));
#58067=CARTESIAN_POINT('Ctrl Pts',(2.31262977609044,43.9773848957545,-16.3374408791774));
#58068=CARTESIAN_POINT('Ctrl Pts',(2.24131140491693,43.7825970865653,-16.3475093049691));
#58069=CARTESIAN_POINT('Ctrl Pts',(2.21155406016932,43.6451167254636,-16.5002466751902));
#58070=CARTESIAN_POINT('Ctrl Pts',(2.16227751834144,44.0313312810579,-16.3577844977291));
#58071=CARTESIAN_POINT('Ctrl Pts',(2.09738048924219,43.8346499499766,-16.3663562334774));
#58072=CARTESIAN_POINT('Ctrl Pts',(2.07072825413426,43.6956582712672,-16.5178019271295));
#58073=CARTESIAN_POINT('Ctrl Pts',(2.11174227376284,44.0484914663749,-16.3643876348749));
#58074=CARTESIAN_POINT('Ctrl Pts',(2.04900260649854,43.8512017716587,-16.3724769498617));
#58075=CARTESIAN_POINT('Ctrl Pts',(2.02339496711712,43.7117292100671,-16.523515913095));
#58076=CARTESIAN_POINT('Ctrl Pts',(2.03530194931424,44.072981459843,-16.3740100616474));
#58077=CARTESIAN_POINT('Ctrl Pts',(1.97581878875163,43.8748161029352,-16.3814021297576));
#58078=CARTESIAN_POINT('Ctrl Pts',(1.95179796907649,43.7346553851609,-16.5318661099767));
#58079=CARTESIAN_POINT('Ctrl Pts',(2.00971557668972,44.0809363660402,-16.3771704866985));
#58080=CARTESIAN_POINT('Ctrl Pts',(1.95132227885587,43.8824850165059,-16.3843344340238));
#58081=CARTESIAN_POINT('Ctrl Pts',(1.92783277153264,43.742100695679,-16.5346127099434));
#58082=CARTESIAN_POINT('Ctrl Pts',(1.95832824291746,44.0964258747234,-16.3833946525917));
#58083=CARTESIAN_POINT('Ctrl Pts',(1.90212235254287,43.8974148464812,-16.3901112587382));
#58084=CARTESIAN_POINT('Ctrl Pts',(1.87970138457326,43.7565946460749,-16.5400299284974));
#58085=CARTESIAN_POINT('Ctrl Pts',(1.93251110054407,44.1039650287676,-16.3864602701835));
#58086=CARTESIAN_POINT('Ctrl Pts',(1.87740326220016,43.9046802305651,-16.392957550475));
#58087=CARTESIAN_POINT('Ctrl Pts',(1.85552003909345,43.7636475423924,-16.5427021859492));
#58088=CARTESIAN_POINT('Ctrl Pts',(1.8030633147258,44.1405497707181,-16.4015192016935));
#58089=CARTESIAN_POINT('Ctrl Pts',(1.75346736507588,43.9399264952154,-16.4069429652539));
#58090=CARTESIAN_POINT('Ctrl Pts',(1.73427417901659,43.7978641021233,-16.5558492664266));
#58091=CARTESIAN_POINT('Ctrl Pts',(1.69906639420128,44.1660683153088,-16.4126226120353));
#58092=CARTESIAN_POINT('Ctrl Pts',(1.65387335486775,43.9644920355918,-16.417272571238));
#58093=CARTESIAN_POINT('Ctrl Pts',(1.63686659515066,43.8217027186776,-16.5656092158287));
#58094=CARTESIAN_POINT('Ctrl Pts',(1.49021426166529,44.2098252495483,-16.4329020282884));
#58095=CARTESIAN_POINT('Ctrl Pts',(1.45386135654879,44.0065631227143,-16.4361701532582));
#58096=CARTESIAN_POINT('Ctrl Pts',(1.44124751778221,43.862520976467,-16.5835644832772));
#58097=CARTESIAN_POINT('Ctrl Pts',(1.38535902634819,44.2280633796216,-16.4420780728859));
#58098=CARTESIAN_POINT('Ctrl Pts',(1.35343204203413,44.0240714574058,-16.4447394017829));
#58099=CARTESIAN_POINT('Ctrl Pts',(1.34303600264843,43.8795003686096,-16.5917598520244));
#58100=CARTESIAN_POINT('Ctrl Pts',(1.17479908853176,44.2573750378148,-16.4584628106134));
#58101=CARTESIAN_POINT('Ctrl Pts',(1.15176493152459,44.0521448192979,-16.4600782830589));
#58102=CARTESIAN_POINT('Ctrl Pts',(1.14581732809311,43.906712349358,-16.6065414193849));
#58103=CARTESIAN_POINT('Ctrl Pts',(1.06909438111656,44.2684484921629,-16.4656715398477));
#58104=CARTESIAN_POINT('Ctrl Pts',(1.05051664045048,44.0627110998794,-16.4668487116589));
#58105=CARTESIAN_POINT('Ctrl Pts',(1.04681016412825,43.9169448659429,-16.6131276573267));
#58106=CARTESIAN_POINT('Ctrl Pts',(0.856834555596582,44.2834493850702,-16.4780804888865));
#58107=CARTESIAN_POINT('Ctrl Pts',(0.847217272305147,44.0769219395685,-16.4785516187993));
#58108=CARTESIAN_POINT('Ctrl Pts',(0.847999308275245,43.9306827648361,-16.6246496409757));
#58109=CARTESIAN_POINT('Ctrl Pts',(0.750279450442107,44.2873769285557,-16.4832807449414));
#58110=CARTESIAN_POINT('Ctrl Pts',(0.745156101872444,44.0805664549735,-16.483484482518));
#58111=CARTESIAN_POINT('Ctrl Pts',(0.748195628510673,43.9341882452755,-16.62958541764));
#58112=CARTESIAN_POINT('Ctrl Pts',(0.58980086051462,44.2878495874714,-16.4895421642784));
#58113=CARTESIAN_POINT('Ctrl Pts',(0.591467911154747,44.0807865596362,-16.4894752008505));
#58114=CARTESIAN_POINT('Ctrl Pts',(0.597885103513613,43.9343461853688,-16.6357218580272));
#58115=CARTESIAN_POINT('Ctrl Pts',(0.536200263354332,44.2871032596941,-16.4913727887242));
#58116=CARTESIAN_POINT('Ctrl Pts',(0.540132926138202,44.0799845128224,-16.4912375073698));
#58117=CARTESIAN_POINT('Ctrl Pts',(0.547680687440361,43.9335480497144,-16.6375561481366));
#58118=CARTESIAN_POINT('Ctrl Pts',(0.455636014550893,44.284613337201,-16.4937296454446));
#58119=CARTESIAN_POINT('Ctrl Pts',(0.462979747202555,44.0774546459417,-16.4935249270376));
#58120=CARTESIAN_POINT('Ctrl Pts',(0.47222106046037,43.9310609294277,-16.6399872269088));
#58121=CARTESIAN_POINT('Ctrl Pts',(0.428754034222533,44.2835549068502,-16.4944504159164));
#58122=CARTESIAN_POINT('Ctrl Pts',(0.437235366462993,44.0763900837954,-16.4942280935165));
#58123=CARTESIAN_POINT('Ctrl Pts',(0.447042346105144,43.9300168543709,-16.6407441942414));
#58124=CARTESIAN_POINT('Ctrl Pts',(0.388389950057066,44.2816222765731,-16.4954337434013));
#58125=CARTESIAN_POINT('Ctrl Pts',(0.398580882778724,44.0744592385522,-16.4951933304063));
#58126=CARTESIAN_POINT('Ctrl Pts',(0.409235765892974,43.9281260198428,-16.6417991152495));
#58127=CARTESIAN_POINT('Ctrl Pts',(0.374928402732455,44.2809205658472,-16.4957452143992));
#58128=CARTESIAN_POINT('Ctrl Pts',(0.385689351820399,44.0737599283669,-16.4955001651808));
#58129=CARTESIAN_POINT('Ctrl Pts',(0.396627154075427,43.9274416182168,-16.6421373338812));
#58130=CARTESIAN_POINT('Ctrl Pts',(0.347991554057913,44.2794017185444,-16.4963354525741));
#58131=CARTESIAN_POINT('Ctrl Pts',(0.359893363301771,44.072249540534,-16.4960839175124));
#58132=CARTESIAN_POINT('Ctrl Pts',(0.371397047876984,43.9259641674669,-16.6427868545954));
#58133=CARTESIAN_POINT('Ctrl Pts',(0.334532328343637,44.2785856289167,-16.4966139069159));
#58134=CARTESIAN_POINT('Ctrl Pts',(0.347004279162573,44.0714394948401,-16.496360523009));
#58135=CARTESIAN_POINT('Ctrl Pts',(0.358790610672238,43.925172130238,-16.6430978003365));
#58136=CARTESIAN_POINT('Ctrl Pts',(0.321034048597817,44.2777095070773,-16.496876587392));
#58137=CARTESIAN_POINT('Ctrl Pts',(0.334078182671872,44.0705712895835,-16.4966227447236));
#58138=CARTESIAN_POINT('Ctrl Pts',(0.346147593727982,43.9243235322772,-16.6433959637249));
#58139=CARTESIAN_POINT('Ctrl Pts',(-0.962949743629567,23.7058553936807,
-16.4718768751861));
#58140=CARTESIAN_POINT('Ctrl Pts',(-0.492765517354465,23.7311233306727,
-16.4993627999076));
#58141=CARTESIAN_POINT('Ctrl Pts',(-0.492844382849881,23.7325958701808,
-16.9710247304714));
#58142=CARTESIAN_POINT('Ctrl Pts',(-0.953542544970481,23.5248859568717,
-16.4724268222023));
#58143=CARTESIAN_POINT('Ctrl Pts',(-0.483855216134323,23.5656632201722,
-16.4996141685673));
#58144=CARTESIAN_POINT('Ctrl Pts',(-0.484033232848877,23.5680782136333,
-16.9715913419337));
#58145=CARTESIAN_POINT('Ctrl Pts',(-0.935468634918637,23.344260801378,-16.4734824711073));
#58146=CARTESIAN_POINT('Ctrl Pts',(-0.466721831624295,23.4005201515163,
-16.5000965390465));
#58147=CARTESIAN_POINT('Ctrl Pts',(-0.467104505517941,23.4038735842938,
-16.9726789786417));
#58148=CARTESIAN_POINT('Ctrl Pts',(-0.89510523809019,23.0738487819855,-16.4757084274388));
#58149=CARTESIAN_POINT('Ctrl Pts',(-0.428567886035457,23.1537264435047,
-16.5010528910333));
#58150=CARTESIAN_POINT('Ctrl Pts',(-0.429298576219848,23.1580445293623,
-16.9749723845983));
#58151=CARTESIAN_POINT('Ctrl Pts',(-0.87943798870027,22.9837992435457,-16.4765564083283));
#58152=CARTESIAN_POINT('Ctrl Pts',(-0.413753117119786,23.0715250912475,
-16.5014098047918));
#58153=CARTESIAN_POINT('Ctrl Pts',(-0.414624019763036,23.0761813304592,
-16.9758460607511));
#58154=CARTESIAN_POINT('Ctrl Pts',(-0.857029346731565,22.871349346421,-16.4777280242054));
#58155=CARTESIAN_POINT('Ctrl Pts',(-0.392594063617177,22.9689868879305,
-16.501882689752));
#58156=CARTESIAN_POINT('Ctrl Pts',(-0.393635213114529,22.9739541736211,
-16.9770531781636));
#58157=CARTESIAN_POINT('Ctrl Pts',(-0.852405448376484,22.8488621194965,
-16.477967944935));
#58158=CARTESIAN_POINT('Ctrl Pts',(-0.388226665517808,22.9484751168198,
-16.5019786523467));
#58159=CARTESIAN_POINT('Ctrl Pts',(-0.389304289803603,22.953511244517,-16.9773003688871));
#58160=CARTESIAN_POINT('Ctrl Pts',(-0.842901150174904,22.8040262491542,
-16.4784568541402));
#58161=CARTESIAN_POINT('Ctrl Pts',(-0.379251273164189,22.9075837307647,
-16.5021720691143));
#58162=CARTESIAN_POINT('Ctrl Pts',(-0.380402193782386,22.9127513713192,
-16.9778040926919));
#58163=CARTESIAN_POINT('Ctrl Pts',(-0.838017665072762,22.7816617177292,
-16.4787060049652));
#58164=CARTESIAN_POINT('Ctrl Pts',(-0.374640213962693,22.8871893178798,
-16.5022695915681));
#58165=CARTESIAN_POINT('Ctrl Pts',(-0.37582813152086,22.892419983537,-16.9780607931916));
#58166=CARTESIAN_POINT('Ctrl Pts',(-0.822975496592716,22.7147273874846,
-16.4794663794692));
#58167=CARTESIAN_POINT('Ctrl Pts',(-0.360437617319141,22.8261502697624,
-16.5025636559244));
#58168=CARTESIAN_POINT('Ctrl Pts',(-0.361739050443223,22.8315706057323,
-16.9788442080374));
#58169=CARTESIAN_POINT('Ctrl Pts',(-0.812425165219932,22.6703168263289,
-16.4799905377545));
#58170=CARTESIAN_POINT('Ctrl Pts',(-0.350480426682779,22.7856681155344,
-16.5027616215283));
#58171=CARTESIAN_POINT('Ctrl Pts',(-0.351857199315679,22.7911973771194,
-16.9793842491552));
#58172=CARTESIAN_POINT('Ctrl Pts',(-0.757088938658021,22.4493146639893,
-16.4826812356247));
#58173=CARTESIAN_POINT('Ctrl Pts',(-0.298223330345641,22.5840652733162,
-16.5037483172792));
#58174=CARTESIAN_POINT('Ctrl Pts',(-0.300027133564499,22.5902863641164,
-16.9821564785501));
#58175=CARTESIAN_POINT('Ctrl Pts',(-0.704568880777145,22.2758671068484,
-16.485061716078));
#58176=CARTESIAN_POINT('Ctrl Pts',(-0.248694534639063,22.4261536301923,
-16.5045273833023));
#58177=CARTESIAN_POINT('Ctrl Pts',(-0.250834802041656,22.4326068013007,
-16.9846090911103));
#58178=CARTESIAN_POINT('Ctrl Pts',(-0.583383247271744,21.9355291968338,
-16.4897950586838));
#58179=CARTESIAN_POINT('Ctrl Pts',(-0.134788012211473,22.1169078656145,
-16.5056480962526));
#58180=CARTESIAN_POINT('Ctrl Pts',(-0.137327617879236,22.1232087702482,
-16.9894858582894));
#58181=CARTESIAN_POINT('Ctrl Pts',(-0.514717124843465,21.7686390767122,
-16.4921487116152));
#58182=CARTESIAN_POINT('Ctrl Pts',(-0.0703104071456902,21.965477603616,
-16.5059887383307));
#58183=CARTESIAN_POINT('Ctrl Pts',(-0.0730122532846286,21.9714905132742,
-16.9919108295178));
#58184=CARTESIAN_POINT('Ctrl Pts',(-0.399512762791793,21.5232549343589,
-16.4952073422415));
#58185=CARTESIAN_POINT('Ctrl Pts',(0.0373481064066343,21.7435521241675,
-16.5057799897692));
#58186=CARTESIAN_POINT('Ctrl Pts',(0.0348926376623413,21.7484140712811,
-16.9950621368967));
#58187=CARTESIAN_POINT('Ctrl Pts',(-0.359073410724847,21.4422868841008,
-16.4961472443844));
#58188=CARTESIAN_POINT('Ctrl Pts',(0.0751411787183878,21.6703115153897,
-16.5055887897801));
#58189=CARTESIAN_POINT('Ctrl Pts',(0.072769709688035,21.6748067697522,-16.996030518433));
#58190=CARTESIAN_POINT('Ctrl Pts',(-0.295310930681003,21.3220928627162,
-16.4973708014316));
#58191=CARTESIAN_POINT('Ctrl Pts',(0.134596754045265,21.5617672788568,-16.5050629722566));
#58192=CARTESIAN_POINT('Ctrl Pts',(0.132492130847063,21.5655395026313,-16.9972911481565));
#58193=CARTESIAN_POINT('Ctrl Pts',(-0.273539280243306,21.2822379645823,
-16.4977475258198));
#58194=CARTESIAN_POINT('Ctrl Pts',(0.154896674034376,21.5257721875215,-16.5048475037642));
#58195=CARTESIAN_POINT('Ctrl Pts',(0.152884306494302,21.5293077854622,-16.9976792871469));
#58196=CARTESIAN_POINT('Ctrl Pts',(-0.240097413338021,21.2227734744632,
-16.4982568025543));
#58197=CARTESIAN_POINT('Ctrl Pts',(0.18604366839339,21.472111121502,-16.504456559693));
#58198=CARTESIAN_POINT('Ctrl Pts',(0.184207260913047,21.4752491704785,-16.9982039940394));
#58199=CARTESIAN_POINT('Ctrl Pts',(-0.228819376074745,21.2030049605629,
-16.4984172542104));
#58200=CARTESIAN_POINT('Ctrl Pts',(0.196547253522777,21.4542711189745,-16.5043148697831));
#58201=CARTESIAN_POINT('Ctrl Pts',(0.19477070980231,21.4572777983998,-16.9983693072139));
#58202=CARTESIAN_POINT('Ctrl Pts',(-0.206000240323432,21.1635745131237,
-16.4987179532799));
#58203=CARTESIAN_POINT('Ctrl Pts',(0.217791152556636,21.4186966483038,-16.5040074771837));
#58204=CARTESIAN_POINT('Ctrl Pts',(0.216144000673567,21.4214319452995,-16.9986791167097));
#58205=CARTESIAN_POINT('Ctrl Pts',(-0.194452744209423,21.1439021274209,
-16.4988582584087));
#58206=CARTESIAN_POINT('Ctrl Pts',(0.228537608365471,21.4009527421141,-16.5038416501483));
#58207=CARTESIAN_POINT('Ctrl Pts',(0.226959835108923,21.4035479624256,-16.9988236728386));
#58208=CARTESIAN_POINT('Ctrl Pts',(-0.089617584523493,20.9678046097149,
-16.5000198041065));
#58209=CARTESIAN_POINT('Ctrl Pts',(0.326274277831968,21.2418141732983,-16.5022358569792));
#58210=CARTESIAN_POINT('Ctrl Pts',(0.325152528104813,21.2434593463896,-17.0000204094314));
#58211=CARTESIAN_POINT('Ctrl Pts',(0.0103895000608808,20.8173601426308,
-16.5003410554286));
#58212=CARTESIAN_POINT('Ctrl Pts',(0.419074339645924,21.1064783083436,-16.5000224206461));
#58213=CARTESIAN_POINT('Ctrl Pts',(0.418823056213946,21.1066916807028,-17.0003513900864));
#58214=CARTESIAN_POINT('Ctrl Pts',(0.223577828128103,20.5282445580889,-16.4988295294443));
#58215=CARTESIAN_POINT('Ctrl Pts',(0.616138593215655,20.8468543167526,-16.4934517294574));
#58216=CARTESIAN_POINT('Ctrl Pts',(0.618503542756773,20.8438593932758,-16.9987940467289));
#58217=CARTESIAN_POINT('Ctrl Pts',(0.336760364078229,20.3895745669501,-16.4969979144061));
#58218=CARTESIAN_POINT('Ctrl Pts',(0.720448287574235,20.7226376096344,-16.4890852353886));
#58219=CARTESIAN_POINT('Ctrl Pts',(0.724514711017868,20.7177957950236,-16.9969069228523));
#58220=CARTESIAN_POINT('Ctrl Pts',(0.576232686432668,20.1239652559013,-16.4903700268213));
#58221=CARTESIAN_POINT('Ctrl Pts',(0.940326943553951,20.4850026896863,-16.4775707284051));
#58222=CARTESIAN_POINT('Ctrl Pts',(0.948813807316047,20.4763328427083,-16.9900781771338));
#58223=CARTESIAN_POINT('Ctrl Pts',(0.702521851144169,19.9970253470419,-16.4855754457147));
#58224=CARTESIAN_POINT('Ctrl Pts',(1.0558985496554,20.3716874051054,-16.4704138841867));
#58225=CARTESIAN_POINT('Ctrl Pts',(1.06710115351391,20.3609329538988,-16.9851383009696));
#58226=CARTESIAN_POINT('Ctrl Pts',(0.868773037863646,19.8458702850025,-16.4771460462422));
#58227=CARTESIAN_POINT('Ctrl Pts',(1.20728915622331,20.2370055044214,-16.4592899829426));
#58228=CARTESIAN_POINT('Ctrl Pts',(1.22281848263862,20.2235192945973,-16.9764534578773));
#58229=CARTESIAN_POINT('Ctrl Pts',(0.902443746971063,19.816016149053,-16.4753379800747));
#58230=CARTESIAN_POINT('Ctrl Pts',(1.23797338983554,20.2103694135477,-16.4569512657965));
#58231=CARTESIAN_POINT('Ctrl Pts',(1.25435577897425,20.1963791777396,-16.974590600823));
#58232=CARTESIAN_POINT('Ctrl Pts',(0.953587295856246,19.7718065477056,-16.4724303864898));
#58233=CARTESIAN_POINT('Ctrl Pts',(1.28453203163021,20.1709385549961,-16.4532690756911));
#58234=CARTESIAN_POINT('Ctrl Pts',(1.30225881653627,20.1561886407066,-16.971594896244));
#58235=CARTESIAN_POINT('Ctrl Pts',(0.970754191649368,19.7571546013071,-16.4714278213924));
#58236=CARTESIAN_POINT('Ctrl Pts',(1.30015758473307,20.157868088241,-16.452011212648));
#58237=CARTESIAN_POINT('Ctrl Pts',(1.31833799903477,20.1428686926593,-16.9705619498875));
#58238=CARTESIAN_POINT('Ctrl Pts',(1.00522776483883,19.7281045215425,-16.4693598939589));
#58239=CARTESIAN_POINT('Ctrl Pts',(1.33152367544567,20.1319543908634,-16.4494410173175));
#58240=CARTESIAN_POINT('Ctrl Pts',(1.35062728897796,20.1164595357428,-16.9684313566742));
#58241=CARTESIAN_POINT('Ctrl Pts',(1.02253286102999,19.7137073645744,-16.4682946770178));
#58242=CARTESIAN_POINT('Ctrl Pts',(1.34726260060578,20.1191123389068,-16.4481288375936));
#58243=CARTESIAN_POINT('Ctrl Pts',(1.36683591525823,20.1033712143075,-16.9673338599297));
#58244=CARTESIAN_POINT('Ctrl Pts',(1.10939730941571,19.6423569831041,-16.4628091753718));
#58245=CARTESIAN_POINT('Ctrl Pts',(1.42629119516503,20.0554244701247,-16.441425558252));
#58246=CARTESIAN_POINT('Ctrl Pts',(1.4481965373725,20.0385072470155,-16.9616821277774));
#58247=CARTESIAN_POINT('Ctrl Pts',(1.17997289092976,19.5873087525872,-16.4579107068088));
#58248=CARTESIAN_POINT('Ctrl Pts',(1.4903494741532,20.0063372584577,-16.4356263390571));
#58249=CARTESIAN_POINT('Ctrl Pts',(1.51430037239319,19.9884634129435,-16.9566352189892));
#58250=CARTESIAN_POINT('Ctrl Pts',(1.39486926268553,19.4281362425253,-16.4415626740924));
#58251=CARTESIAN_POINT('Ctrl Pts',(1.68530301764386,19.8642142740128,-16.4168034493466));
#58252=CARTESIAN_POINT('Ctrl Pts',(1.71558067464331,19.8437611662803,-16.9397917847999));
#58253=CARTESIAN_POINT('Ctrl Pts',(1.54235226719088,19.3299705812408,-16.4284621948059));
#58254=CARTESIAN_POINT('Ctrl Pts',(1.81854043497645,19.7766504246625,-16.4023921233297));
#58255=CARTESIAN_POINT('Ctrl Pts',(1.85371899319303,19.7545196774371,-16.9262943189646));
#58256=CARTESIAN_POINT('Ctrl Pts',(1.8455081137815,19.1492250077106,-16.3971741591057));
#58257=CARTESIAN_POINT('Ctrl Pts',(2.09201064403488,19.6148487582272,-16.3692914888457));
#58258=CARTESIAN_POINT('Ctrl Pts',(2.13766655088791,19.5902055590468,-16.8940581558081));
#58259=CARTESIAN_POINT('Ctrl Pts',(2.00118134550501,19.0666455566031,-16.3789878356581));
#58260=CARTESIAN_POINT('Ctrl Pts',(2.23204313940034,19.5407583231452,-16.3506228147975));
#58261=CARTESIAN_POINT('Ctrl Pts',(2.28347615445228,19.5151333486988,-16.8753207313665));
#58262=CARTESIAN_POINT('Ctrl Pts',(2.24082421386082,18.9545554863542,-16.3473300317566));
#58263=CARTESIAN_POINT('Ctrl Pts',(2.44755457756016,19.4395071081516,-16.3189516367199));
#58264=CARTESIAN_POINT('Ctrl Pts',(2.50793498547555,19.4132333079427,-16.8427035993773));
#58265=CARTESIAN_POINT('Ctrl Pts',(2.32172912386916,18.9191586223815,-16.3360470573507));
#58266=CARTESIAN_POINT('Ctrl Pts',(2.52026069725735,19.4074307794645,-16.3077882731722));
#58267=CARTESIAN_POINT('Ctrl Pts',(2.58371367100673,19.3810543481895,-16.8310787173966));
#58268=CARTESIAN_POINT('Ctrl Pts',(2.42415296888238,18.8774057450501,-16.3209653852811));
#58269=CARTESIAN_POINT('Ctrl Pts',(2.61232353439924,19.3694170191855,-16.2930124644539));
#58270=CARTESIAN_POINT('Ctrl Pts',(2.67964782784832,19.3430971951672,-16.8155400254028));
#58271=CARTESIAN_POINT('Ctrl Pts',(2.44470241052432,18.8691798998893,-16.3179001338654));
#58272=CARTESIAN_POINT('Ctrl Pts',(2.63079004346867,19.3619205223288,-16.2900170229615));
#58273=CARTESIAN_POINT('Ctrl Pts',(2.69889523418508,19.3356191558291,-16.8123818878633));
#58274=CARTESIAN_POINT('Ctrl Pts',(2.48593111009814,18.8529788338351,-16.3116700914));
#58275=CARTESIAN_POINT('Ctrl Pts',(2.6678392301345,19.3471377665628,-16.2839429469447));
#58276=CARTESIAN_POINT('Ctrl Pts',(2.7375116377121,19.3208909170966,-16.8059630564883));
#58277=CARTESIAN_POINT('Ctrl Pts',(2.50661987329755,18.8450002475771,-16.3085037647573));
#58278=CARTESIAN_POINT('Ctrl Pts',(2.68642985951431,19.3398486136801,-16.2808629383133));
#58279=CARTESIAN_POINT('Ctrl Pts',(2.75688953799591,19.3136376584055,-16.8027007808385));
#58280=CARTESIAN_POINT('Ctrl Pts',(2.5686809342295,18.821516920274,-16.2988843543115));
#58281=CARTESIAN_POINT('Ctrl Pts',(2.74219268886266,19.3183677676536,-16.2715271448004));
#58282=CARTESIAN_POINT('Ctrl Pts',(2.81501834153598,19.2922891838504,-16.7927898737225));
#58283=CARTESIAN_POINT('Ctrl Pts',(2.61012992508159,18.8064320620533,-16.2922985348497));
#58284=CARTESIAN_POINT('Ctrl Pts',(2.77943541677509,19.3045303867492,-16.2651626675075));
#58285=CARTESIAN_POINT('Ctrl Pts',(2.85384107841252,19.2785756790292,-16.7860044845856));
#58286=CARTESIAN_POINT('Ctrl Pts',(2.81773937785444,18.7338190214716,-16.2584950468795));
#58287=CARTESIAN_POINT('Ctrl Pts',(2.96587020075137,19.2377636805501,-16.2326478240223));
#58288=CARTESIAN_POINT('Ctrl Pts',(3.04829616661998,19.2125638384852,-16.751176651373));
#58289=CARTESIAN_POINT('Ctrl Pts',(2.9849895752519,18.6847044470942,-16.2286549196291));
#58290=CARTESIAN_POINT('Ctrl Pts',(3.11604918687771,19.1919225453077,-16.2043747173323));
#58291=CARTESIAN_POINT('Ctrl Pts',(3.20494920623192,19.1679142333196,-16.7204322819396));
#58292=CARTESIAN_POINT('Ctrl Pts',(3.32161623394242,18.6036838578296,-16.1631144542047));
#58293=CARTESIAN_POINT('Ctrl Pts',(3.41910319125249,19.1146585110534,-16.1428992719901));
#58294=CARTESIAN_POINT('Ctrl Pts',(3.52024682897757,19.0942591651346,-16.6529057512598));
#58295=CARTESIAN_POINT('Ctrl Pts',(3.49099316674984,18.5717797729774,-16.1274145820174));
#58296=CARTESIAN_POINT('Ctrl Pts',(3.5716609663928,19.083259988654,-16.1097791546225));
#58297=CARTESIAN_POINT('Ctrl Pts',(3.67889185273297,19.0652554551678,-16.6161240713731));
#58298=CARTESIAN_POINT('Ctrl Pts',(3.74656986701161,18.5366323538023,-16.069251626303));
#58299=CARTESIAN_POINT('Ctrl Pts',(3.80309044573612,19.0468400841815,-16.0560272802084));
#58300=CARTESIAN_POINT('Ctrl Pts',(3.91827493418733,19.033303258113,-16.5561986123435));
#58301=CARTESIAN_POINT('Ctrl Pts',(3.83201461596044,18.5270381829345,-16.049094870664));
#58302=CARTESIAN_POINT('Ctrl Pts',(3.88043400857609,19.0365067070544,-16.0374888868254));
#58303=CARTESIAN_POINT('Ctrl Pts',(3.99830581044114,19.0245812847932,-16.5354310500837));
#58304=CARTESIAN_POINT('Ctrl Pts',(3.9605555485118,18.5158358162941,-16.017676026607));
#58305=CARTESIAN_POINT('Ctrl Pts',(3.99711396115319,19.0237071198211,-16.0086240190836));
#58306=CARTESIAN_POINT('Ctrl Pts',(4.11870224954153,19.0143973144301,-16.503060126001));
#58307=CARTESIAN_POINT('Ctrl Pts',(4.00346486557186,18.5126333940285,-16.0070057718171));
#58308=CARTESIAN_POINT('Ctrl Pts',(4.03605994925758,19.019895083143,-15.9988412256294));
#58309=CARTESIAN_POINT('Ctrl Pts',(4.15889278554975,19.011486021175,-16.4920665324453));
#58310=CARTESIAN_POINT('Ctrl Pts',(4.08940780911621,18.5072956852501,-15.9852653553081));
#58311=CARTESIAN_POINT('Ctrl Pts',(4.11414010512615,19.0131810195212,-15.9789257486132));
#58312=CARTESIAN_POINT('Ctrl Pts',(4.23939029066013,19.0066335576006,-16.4696673198694));
#58313=CARTESIAN_POINT('Ctrl Pts',(4.13245806836038,18.5051597914318,-15.9741908394575));
#58314=CARTESIAN_POINT('Ctrl Pts',(4.15328411493104,19.0102768074715,-15.9687909906719));
#58315=CARTESIAN_POINT('Ctrl Pts',(4.27971283869093,19.0046918351941,-16.4582572149842));
#58316=CARTESIAN_POINT('Ctrl Pts',(4.34784672550312,18.4971683714463,-15.9178500886953));
#58317=CARTESIAN_POINT('Ctrl Pts',(4.3487542282718,18.9980972539458,-15.9174161894257));
#58318=CARTESIAN_POINT('Ctrl Pts',(4.4814542353807,18.9974269049179,-16.4002091813211));
#58319=CARTESIAN_POINT('Ctrl Pts',(4.51834575570717,18.4994317728118,-15.8702720675625));
#58320=CARTESIAN_POINT('Ctrl Pts',(4.50442609142234,18.9957318186494,-15.8740794573458));
#58321=CARTESIAN_POINT('Ctrl Pts',(4.64115026261982,18.9994845360441,-16.3511894124623));
#58322=CARTESIAN_POINT('Ctrl Pts',(4.85588770099964,18.5202816685198,-15.7702675469788));
#58323=CARTESIAN_POINT('Ctrl Pts',(4.81424862806617,19.0054597207642,-15.7829152581971));
#58324=CARTESIAN_POINT('Ctrl Pts',(4.95730518812699,19.0184389728909,-16.2481544747099));
#58325=CARTESIAN_POINT('Ctrl Pts',(5.02293020096387,18.5388709869828,-15.717840780607));
#58326=CARTESIAN_POINT('Ctrl Pts',(4.96817008474715,19.0174140221494,-15.7352002323915));
#58327=CARTESIAN_POINT('Ctrl Pts',(5.11376369695387,19.0353383433437,-16.1941390305004));
#58328=CARTESIAN_POINT('Ctrl Pts',(5.35366345256434,18.5918857067752,-15.6082873578935));
#58329=CARTESIAN_POINT('Ctrl Pts',(5.27463071593156,19.05568949738,-15.6352352679861));
#58330=CARTESIAN_POINT('Ctrl Pts',(5.42354133961961,19.0835335214419,-16.0812658326074));
#58331=CARTESIAN_POINT('Ctrl Pts',(5.51735404460432,18.626311704008,-15.5511604175382));
#58332=CARTESIAN_POINT('Ctrl Pts',(5.42697409841425,19.0818325558241,-15.5831012458257));
#58333=CARTESIAN_POINT('Ctrl Pts',(5.57686032344895,19.1148298694965,-16.0224077860923));
#58334=CARTESIAN_POINT('Ctrl Pts',(5.71990424855873,18.67921397641,-15.4769039866353));
#58335=CARTESIAN_POINT('Ctrl Pts',(5.61739054976128,19.1238638166436,-15.514780928748));
#58336=CARTESIAN_POINT('Ctrl Pts',(5.76657673742069,19.1629228269299,-15.9459011766186));
#58337=CARTESIAN_POINT('Ctrl Pts',(5.7603110112591,18.6902890021976,-15.4619103121913));
#58338=CARTESIAN_POINT('Ctrl Pts',(5.65525437053189,19.1326840835,-15.5010398404495));
#58339=CARTESIAN_POINT('Ctrl Pts',(5.80442328554253,19.1729910285574,-15.9304531518085));
#58340=CARTESIAN_POINT('Ctrl Pts',(5.82076645659554,18.7076461532893,-15.4392079207446));
#58341=CARTESIAN_POINT('Ctrl Pts',(5.7120216468109,19.1466132281685,-15.4802028149947));
#58342=CARTESIAN_POINT('Ctrl Pts',(5.86104821118419,19.1887702511317,-15.9070628142843));
#58343=CARTESIAN_POINT('Ctrl Pts',(5.84090083204721,18.7135586164393,-15.431601930293));
#58344=CARTESIAN_POINT('Ctrl Pts',(5.73092530850596,19.1513689910166,-15.4732248266298));
#58345=CARTESIAN_POINT('Ctrl Pts',(5.87990685170539,19.1941452156697,-15.8992263409633));
#58346=CARTESIAN_POINT('Ctrl Pts',(5.88102767187931,18.7256047794529,-15.4163541146221));
#58347=CARTESIAN_POINT('Ctrl Pts',(5.76862341141302,19.1610883165219,-15.4592309087857));
#58348=CARTESIAN_POINT('Ctrl Pts',(5.91749121334782,19.2050962692109,-15.8835164738311));
#58349=CARTESIAN_POINT('Ctrl Pts',(5.90102969963314,18.7317411147533,-15.408708735978));
#58350=CARTESIAN_POINT('Ctrl Pts',(5.78742667675602,19.1660535865446,-15.4522118926581));
#58351=CARTESIAN_POINT('Ctrl Pts',(5.93622589191204,19.2106747537697,-15.8756394187103));
#58352=CARTESIAN_POINT('Ctrl Pts',(6.00073572818559,18.7629847662334,-15.3703764930614));
#58353=CARTESIAN_POINT('Ctrl Pts',(5.88100137903186,19.1913491554074,-15.4170877663835));
#58354=CARTESIAN_POINT('Ctrl Pts',(6.0296144427393,19.2390780635469,-15.8361456018249));
#58355=CARTESIAN_POINT('Ctrl Pts',(6.07952793866853,18.7897768131789,-15.3393735694147));
#58356=CARTESIAN_POINT('Ctrl Pts',(5.95530612330359,19.2133034465851,-15.3885782624779));
#58357=CARTESIAN_POINT('Ctrl Pts',(6.10341429757601,19.2634344611989,-15.8042032023619));
#58358=CARTESIAN_POINT('Ctrl Pts',(6.3130827298411,18.875408878203,-15.2454305378321));
#58359=CARTESIAN_POINT('Ctrl Pts',(6.17541857033644,19.2839556861349,-15.3023083477907));
#58360=CARTESIAN_POINT('Ctrl Pts',(6.32217081560629,19.3412817673883,-15.7074134345399));
#58361=CARTESIAN_POINT('Ctrl Pts',(6.46502925485296,18.939491446264,-15.1815553755486));
#58362=CARTESIAN_POINT('Ctrl Pts',(6.31979410155795,19.3377274535367,-15.2433154114145));
#58363=CARTESIAN_POINT('Ctrl Pts',(6.46448985405949,19.3995386285318,-15.6416026748871));
#58364=CARTESIAN_POINT('Ctrl Pts',(6.76176840236203,19.0812662510744,-15.0517346163669));
#58365=CARTESIAN_POINT('Ctrl Pts',(6.60303555768087,19.4585649747456,-15.1229332761854));
#58366=CARTESIAN_POINT('Ctrl Pts',(6.74242730949661,19.5284247765807,-15.5078479818444));
#58367=CARTESIAN_POINT('Ctrl Pts',(6.90656044807258,19.1589588891342,-14.985788123841));
#58368=CARTESIAN_POINT('Ctrl Pts',(6.74191080864818,19.5254379131911,-15.0615983721264));
#58369=CARTESIAN_POINT('Ctrl Pts',(6.87804518597047,19.5990544270626,-15.439903124207));
#58370=CARTESIAN_POINT('Ctrl Pts',(7.11851697824708,19.2857408919594,-14.8856582575188));
#58371=CARTESIAN_POINT('Ctrl Pts',(6.94669094873197,19.6362246024488,-14.967804995196));
#58372=CARTESIAN_POINT('Ctrl Pts',(7.07657194161257,19.7143107625128,-15.3367390395514));
#58373=CARTESIAN_POINT('Ctrl Pts',(7.18829589041354,19.3297120059879,-14.8520803094002));
#58374=CARTESIAN_POINT('Ctrl Pts',(7.01403806331814,19.6746887916144,-14.936401435585));
#58375=CARTESIAN_POINT('Ctrl Pts',(7.14192959263245,19.7542844918657,-15.3021435844138));
#58376=CARTESIAN_POINT('Ctrl Pts',(7.29165902215419,19.3982694262532,-14.8014587300021));
#58377=CARTESIAN_POINT('Ctrl Pts',(7.11415554816123,19.7350433954885,-14.8888967056587));
#58378=CARTESIAN_POINT('Ctrl Pts',(7.23874353497939,19.8166094030417,-15.249988027825));
#58379=CARTESIAN_POINT('Ctrl Pts',(7.3258957750402,19.4215555778275,-14.784542462985));
#58380=CARTESIAN_POINT('Ctrl Pts',(7.14729834641863,19.7555520830343,-14.8730341341912));
#58381=CARTESIAN_POINT('Ctrl Pts',(7.27081101338128,19.8377786262931,-15.2325591498893));
#58382=CARTESIAN_POINT('Ctrl Pts',(7.39393376089708,19.4690038300525,-14.7506334876184));
#58383=CARTESIAN_POINT('Ctrl Pts',(7.21322647966689,19.797430733529,-14.8412096765173));
#58384=CARTESIAN_POINT('Ctrl Pts',(7.33453804573537,19.8809133897312,-15.1976226366084));
#58385=CARTESIAN_POINT('Ctrl Pts',(7.42775939794765,19.4931849686784,-14.7336281269098));
#58386=CARTESIAN_POINT('Ctrl Pts',(7.24603686392702,19.818815013828,-14.8252361070978));
#58387=CARTESIAN_POINT('Ctrl Pts',(7.36622045719149,19.9028962373553,-15.180101965099));
#58388=CARTESIAN_POINT('Ctrl Pts',(7.59506589867206,19.6157601057687,-14.6488051829882));
#58389=CARTESIAN_POINT('Ctrl Pts',(7.40770361714788,19.9269175872,-14.745870258467));
#58390=CARTESIAN_POINT('Ctrl Pts',(7.52292625224057,20.0143281505988,-15.0927086470378));
#58391=CARTESIAN_POINT('Ctrl Pts',(7.72362179982455,19.7195008596405,-14.5813365909781));
#58392=CARTESIAN_POINT('Ctrl Pts',(7.53309970113241,20.0194651615337,-14.6822094135442));
#58393=CARTESIAN_POINT('Ctrl Pts',(7.64333672678021,20.1086379031159,-15.0231955640876));
#58394=CARTESIAN_POINT('Ctrl Pts',(7.97062286550307,19.9382205720063,-14.4477985043873));
#58395=CARTESIAN_POINT('Ctrl Pts',(7.77465365444886,20.2159950446239,-14.5558500950358));
#58396=CARTESIAN_POINT('Ctrl Pts',(7.87468756705251,20.3074739578748,-14.8856108938969));
#58397=CARTESIAN_POINT('Ctrl Pts',(8.08906736132104,20.0531994360158,-14.3817276587201));
#58398=CARTESIAN_POINT('Ctrl Pts',(7.89097239699678,20.3198807121421,-14.493112481288));
#58399=CARTESIAN_POINT('Ctrl Pts',(7.98562730607927,20.4120001735958,-14.8175379122407));
#58400=CARTESIAN_POINT('Ctrl Pts',(8.31600323145087,20.294652390103,-14.2517083706198));
#58401=CARTESIAN_POINT('Ctrl Pts',(8.11429680827963,20.5393096561358,-14.3693578331021));
#58402=CARTESIAN_POINT('Ctrl Pts',(8.19818430429942,20.6315028094719,-14.6835786686257));
#58403=CARTESIAN_POINT('Ctrl Pts',(8.42449547871763,20.4211244360891,-14.1877579569348));
#58404=CARTESIAN_POINT('Ctrl Pts',(8.22147030516298,20.6547792674814,-14.3082854478819));
#58405=CARTESIAN_POINT('Ctrl Pts',(8.29980237977681,20.7464773718416,-14.6176903733931));
#58406=CARTESIAN_POINT('Ctrl Pts',(8.57965570414123,20.6199525825303,-14.0940823744386));
#58407=CARTESIAN_POINT('Ctrl Pts',(8.37539273565275,20.8376518525986,-14.2184166621781));
#58408=CARTESIAN_POINT('Ctrl Pts',(8.44513150955405,20.9272301946537,-14.5211761516265));
#58409=CARTESIAN_POINT('Ctrl Pts',(8.63011026247902,20.6877520189069,-14.0632335704244));
#58410=CARTESIAN_POINT('Ctrl Pts',(8.42538599398931,20.8999711961408,-14.1888588770955));
#58411=CARTESIAN_POINT('Ctrl Pts',(8.49238921931927,20.9888660332051,-14.4893925398783));
#58412=CARTESIAN_POINT('Ctrl Pts',(8.70385476035904,20.7918332707026,-14.0176227553152));
#58413=CARTESIAN_POINT('Ctrl Pts',(8.49861509669621,20.9959548800499,-14.1450582060422));
#58414=CARTESIAN_POINT('Ctrl Pts',(8.56146119773943,21.0834853334181,-14.442399585989));
#58415=CARTESIAN_POINT('Ctrl Pts',(8.72811318594382,20.8269242967422,-14.0025296682918));
#58416=CARTESIAN_POINT('Ctrl Pts',(8.52268865375042,21.0283052437927,-14.130573551022));
#58417=CARTESIAN_POINT('Ctrl Pts',(8.58418258654386,21.1153862597525,-14.4268491348457));
#58418=CARTESIAN_POINT('Ctrl Pts',(8.77597501193154,20.897920431518,-13.9725824201542));
#58419=CARTESIAN_POINT('Ctrl Pts',(8.5702088349925,21.0938179609117,-14.1018188553834));
#58420=CARTESIAN_POINT('Ctrl Pts',(8.62901184306147,21.179928186994,-14.3959943990639));
#58421=CARTESIAN_POINT('Ctrl Pts',(8.7994896585319,20.9336941025988,-13.9577838001673));
#58422=CARTESIAN_POINT('Ctrl Pts',(8.59357050615549,21.1268592854661,-14.0876006312119));
#58423=CARTESIAN_POINT('Ctrl Pts',(8.65103657958592,21.2124496995907,-14.3807473380954));
#58424=CARTESIAN_POINT('Ctrl Pts',(8.91495935746604,21.1138958131933,-13.8847199993329));
#58425=CARTESIAN_POINT('Ctrl Pts',(8.70792670494221,21.2928426773794,-14.0176222210528));
#58426=CARTESIAN_POINT('Ctrl Pts',(8.75919001035479,21.3762694014718,-14.305469494962));
#58427=CARTESIAN_POINT('Ctrl Pts',(9.00065683266863,21.2623657685385,-13.8292130781874));
#58428=CARTESIAN_POINT('Ctrl Pts',(8.79340445777157,21.4305988476776,-13.9640890064058));
#58429=CARTESIAN_POINT('Ctrl Pts',(8.83945761419094,21.5112420614924,-14.2482805529682));
#58430=CARTESIAN_POINT('Ctrl Pts',(9.15871068236081,21.5682334421585,-13.7250492319199));
#58431=CARTESIAN_POINT('Ctrl Pts',(8.95109569231193,21.7151215946974,-13.8635721361939));
#58432=CARTESIAN_POINT('Ctrl Pts',(8.98749702761635,21.789303528528,-14.140960241944));
#58433=CARTESIAN_POINT('Ctrl Pts',(9.23106853128776,21.7256297738407,-13.6763903437594));
#58434=CARTESIAN_POINT('Ctrl Pts',(9.02351685850879,21.8619866213685,-13.8164716865597));
#58435=CARTESIAN_POINT('Ctrl Pts',(9.05527021632604,21.9323910758609,-14.0908268477781));
#58436=CARTESIAN_POINT('Ctrl Pts',(9.36200027235301,22.0499603000645,-13.5870979228432));
#58437=CARTESIAN_POINT('Ctrl Pts',(9.15454270838474,22.1651688960518,-13.7300319644641));
#58438=CARTESIAN_POINT('Ctrl Pts',(9.17790600436843,22.2272369528839,-13.9988286084952));
#58439=CARTESIAN_POINT('Ctrl Pts',(9.42057845052407,22.2168912940591,-13.546461187714));
#58440=CARTESIAN_POINT('Ctrl Pts',(9.21333491179549,22.3216229093717,-13.6905787947584));
#58441=CARTESIAN_POINT('Ctrl Pts',(9.23277261467539,22.378992374506,-13.9569604616345));
#58442=CARTESIAN_POINT('Ctrl Pts',(9.4781725544487,22.4106027511509,-13.5060840404267));
#58443=CARTESIAN_POINT('Ctrl Pts',(9.27124287178487,22.5038190489669,-13.6513005654783));
#58444=CARTESIAN_POINT('Ctrl Pts',(9.28671750556737,22.5550936679072,-13.9153597695754));
#58445=CARTESIAN_POINT('Ctrl Pts',(9.48444711786266,22.4321789243944,-13.5016783842282));
#58446=CARTESIAN_POINT('Ctrl Pts',(9.27753750017006,22.5240683387227,-13.6470243760949));
#58447=CARTESIAN_POINT('Ctrl Pts',(9.29259450685464,22.5747083672934,-13.9108206091289));
#58448=CARTESIAN_POINT('Ctrl Pts',(9.49672536685248,22.4753618131691,-13.4930450095317));
#58449=CARTESIAN_POINT('Ctrl Pts',(9.28985611838946,22.564602870967,-13.6386438680677));
#58450=CARTESIAN_POINT('Ctrl Pts',(9.30409479488525,22.6139655317586,-13.901925618187));
#58451=CARTESIAN_POINT('Ctrl Pts',(9.50273249627371,22.4969800713172,-13.4888148772171));
#58452=CARTESIAN_POINT('Ctrl Pts',(9.29588389997394,22.5848994479116,-13.6345369851084));
#58453=CARTESIAN_POINT('Ctrl Pts',(9.30972130716465,22.6336184901156,-13.8975673005029));
#58454=CARTESIAN_POINT('Ctrl Pts',(9.52035918168828,22.5619152496179,-13.476385561487));
#58455=CARTESIAN_POINT('Ctrl Pts',(9.31356710910104,22.6458558854866,-13.6224724720524));
#58456=CARTESIAN_POINT('Ctrl Pts',(9.32623114985529,22.6926504596105,-13.8847613405295));
#58457=CARTESIAN_POINT('Ctrl Pts',(9.53158409879775,22.6053125634296,-13.468447447099));
#58458=CARTESIAN_POINT('Ctrl Pts',(9.32483548260588,22.6866238631496,-13.6147621214551));
#58459=CARTESIAN_POINT('Ctrl Pts',(9.3367448460817,22.732102555901,-13.8765826780708));
#58460=CARTESIAN_POINT('Ctrl Pts',(9.56368814998023,22.7358261581148,-13.4456891694235));
#58461=CARTESIAN_POINT('Ctrl Pts',(9.35704811788232,22.8091939866226,-13.5926671654132));
#58462=CARTESIAN_POINT('Ctrl Pts',(9.36681475560692,22.8507512566856,-13.8531347586999));
#58463=CARTESIAN_POINT('Ctrl Pts',(9.5829975742177,22.823263935959,-13.4319248824045));
#58464=CARTESIAN_POINT('Ctrl Pts',(9.37645126647122,22.8914279771673,-13.5792841202355));
#58465=CARTESIAN_POINT('Ctrl Pts',(9.38490071726704,22.9302401313564,-13.8389533735087));
#58466=CARTESIAN_POINT('Ctrl Pts',(9.63467303059377,23.086869673514,-13.3949568797211));
#58467=CARTESIAN_POINT('Ctrl Pts',(9.4283215850424,23.1391952104619,-13.5433774600759));
#58468=CARTESIAN_POINT('Ctrl Pts',(9.43330197030269,23.1698816673068,-13.8008651332953));
#58469=CARTESIAN_POINT('Ctrl Pts',(9.66080205100456,23.264327543883,-13.3760749408244));
#58470=CARTESIAN_POINT('Ctrl Pts',(9.45464141905301,23.3064610473423,-13.5249723329533));
#58471=CARTESIAN_POINT('Ctrl Pts',(9.45777543217764,23.3312069757732,-13.7814110162615));
#58472=CARTESIAN_POINT('Ctrl Pts',(9.69618216865947,23.6227778055913,-13.3504504958979));
#58473=CARTESIAN_POINT('Ctrl Pts',(9.49022252619599,23.6442122621145,-13.5000339915227));
#58474=CARTESIAN_POINT('Ctrl Pts',(9.49091383452651,23.6570707923046,-13.7550100763112));
#58475=CARTESIAN_POINT('Ctrl Pts',(9.70543536945587,23.8037698369644,-13.3437073024875));
#58476=CARTESIAN_POINT('Ctrl Pts',(9.49954967786973,23.8149979384621,-13.4934560518724));
#58477=CARTESIAN_POINT('Ctrl Pts',(9.4995807433815,23.8216089741294,-13.7480625443467));
#58478=CARTESIAN_POINT('Ctrl Pts',(9.70597513873851,24.0323294734863,-13.3433146790455));
#58479=CARTESIAN_POINT('Ctrl Pts',(9.50009270586957,24.0304786994239,-13.4930737933728));
#58480=CARTESIAN_POINT('Ctrl Pts',(9.50008631309344,24.0293904252603,-13.7476580232753));
#58481=CARTESIAN_POINT('Ctrl Pts',(9.70553034474903,24.0781576052184,-13.3436382698279));
#58482=CARTESIAN_POINT('Ctrl Pts',(9.49964517461909,24.0736863887931,-13.4933888785566));
#58483=CARTESIAN_POINT('Ctrl Pts',(9.49966970135809,24.0710523558596,-13.7479914198069));
#58484=CARTESIAN_POINT('Ctrl Pts',(9.70402058186149,24.1470768987552,-13.3447362257199));
#58485=CARTESIAN_POINT('Ctrl Pts',(9.49812638956954,24.1386573118864,-13.4944577823999));
#58486=CARTESIAN_POINT('Ctrl Pts',(9.49825559862898,24.1337062480285,-13.7491226469482));
#58487=CARTESIAN_POINT('Ctrl Pts',(9.70337612425004,24.1700954524399,-13.3452048589811));
#58488=CARTESIAN_POINT('Ctrl Pts',(9.49747804813204,24.160357728836,-13.4949140382431));
#58489=CARTESIAN_POINT('Ctrl Pts',(9.49765197443261,24.1546322022357,-13.7496054811704));
#58490=CARTESIAN_POINT('Ctrl Pts',(9.70181039353469,24.2160242659793,-13.3463431704996));
#58491=CARTESIAN_POINT('Ctrl Pts',(9.49590295559263,24.2036548244372,-13.4960222310312));
#58492=CARTESIAN_POINT('Ctrl Pts',(9.49618544965948,24.1963856617205,-13.7507782868312));
#58493=CARTESIAN_POINT('Ctrl Pts',(9.70088893502563,24.2389518587485,-13.3470129835802));
#58494=CARTESIAN_POINT('Ctrl Pts',(9.49497597105382,24.225268486177,-13.4966743322698));
#58495=CARTESIAN_POINT('Ctrl Pts',(9.49532237574291,24.2172289242047,-13.7514683972106));
#58496=CARTESIAN_POINT('Ctrl Pts',(9.69559422432726,24.3534073082494,-13.3508606484318));
#58497=CARTESIAN_POINT('Ctrl Pts',(9.48964887351038,24.3331782299118,-13.5004206915048));
#58498=CARTESIAN_POINT('Ctrl Pts',(9.49036314227762,24.3212793145206,-13.7554326574748));
#58499=CARTESIAN_POINT('Ctrl Pts',(9.68916022224817,24.4443879326826,-13.3555339196467));
#58500=CARTESIAN_POINT('Ctrl Pts',(9.48317387006694,24.4189497885899,-13.504972050757));
#58501=CARTESIAN_POINT('Ctrl Pts',(9.48433680488061,24.4039889585799,-13.7602475425037));
#58502=CARTESIAN_POINT('Ctrl Pts',(9.6634393151647,24.715630632223,-13.3741687205965));
#58503=CARTESIAN_POINT('Ctrl Pts',(9.45729426491734,24.674657571566,-13.52311676352));
#58504=CARTESIAN_POINT('Ctrl Pts',(9.4602455967653,24.650573187534,-13.7794470320152));
#58505=CARTESIAN_POINT('Ctrl Pts',(9.63775002362843,24.8941969109951,-13.3927413312077));
#58506=CARTESIAN_POINT('Ctrl Pts',(9.43141637017533,24.8429770623408,-13.541221148463));
#58507=CARTESIAN_POINT('Ctrl Pts',(9.43618400243639,24.8129061398801,-13.798582447208));
#58508=CARTESIAN_POINT('Ctrl Pts',(9.56979665799707,25.2469945208445,-13.441381543842));
#58509=CARTESIAN_POINT('Ctrl Pts',(9.36314059164007,25.174907732864,-13.5885109273976));
#58510=CARTESIAN_POINT('Ctrl Pts',(9.37253622263319,25.1336311822155,-13.8486965992851));
#58511=CARTESIAN_POINT('Ctrl Pts',(9.52753173217289,25.4212256474459,-13.4714495820274));
#58512=CARTESIAN_POINT('Ctrl Pts',(9.320621388888,25.3387948465226,-13.6177780168233));
#58513=CARTESIAN_POINT('Ctrl Pts',(9.33294924072412,25.2920230872501,-13.8796757870884));
#58514=CARTESIAN_POINT('Ctrl Pts',(9.47065193933464,25.6148436317644,-13.5113586085727));
#58515=CARTESIAN_POINT('Ctrl Pts',(9.26369917506079,25.5200585720568,-13.6564194462368));
#58516=CARTESIAN_POINT('Ctrl Pts',(9.27967340329896,25.4680394032114,-13.9207941723777));
#58517=CARTESIAN_POINT('Ctrl Pts',(9.46420202333222,25.6363234509834,-13.5158774981925));
#58518=CARTESIAN_POINT('Ctrl Pts',(9.25722980273212,25.5402115827205,-13.6608046879957));
#58519=CARTESIAN_POINT('Ctrl Pts',(9.27363215982219,25.4875665080051,-13.9254499975484));
#58520=CARTESIAN_POINT('Ctrl Pts',(9.45104171472625,25.6792165551332,-13.5250831787126));
#58521=CARTESIAN_POINT('Ctrl Pts',(9.24403189021062,25.580446362938,-13.6697366125152));
#58522=CARTESIAN_POINT('Ctrl Pts',(9.26130570026585,25.5265602319081,-13.9349346368283));
#58523=CARTESIAN_POINT('Ctrl Pts',(9.44433889025821,25.7006047210845,-13.5297646668679));
#58524=CARTESIAN_POINT('Ctrl Pts',(9.23731060205227,25.6005049962199,-13.6742783692687));
#58525=CARTESIAN_POINT('Ctrl Pts',(9.25502757293848,25.546004015586,-13.9397579877384));
#58526=CARTESIAN_POINT('Ctrl Pts',(9.42389557569635,25.7645001936973,-13.5440196484565));
#58527=CARTESIAN_POINT('Ctrl Pts',(9.21680681254345,25.6604369459517,-13.6881105608007));
#58528=CARTESIAN_POINT('Ctrl Pts',(9.23587956495122,25.6040907981566,-13.9544449365423));
#58529=CARTESIAN_POINT('Ctrl Pts',(9.40980812022507,25.806778431026,-13.5538121533282));
#58530=CARTESIAN_POINT('Ctrl Pts',(9.20268515890637,25.7000622918785,-13.6976073638699));
#58531=CARTESIAN_POINT('Ctrl Pts',(9.22268470384003,25.6425255523807,-13.9645341828734));
#58532=CARTESIAN_POINT('Ctrl Pts',(9.36619491727129,25.932680699603,-13.5840216342671));
#58533=CARTESIAN_POINT('Ctrl Pts',(9.1589493065576,25.8180973351854,-13.7269154264562));
#58534=CARTESIAN_POINT('Ctrl Pts',(9.18183487229295,25.756982139071,-13.9956590985482));
#58535=CARTESIAN_POINT('Ctrl Pts',(9.33531944381127,26.0153730275513,-13.6052699759399));
#58536=CARTESIAN_POINT('Ctrl Pts',(9.12801654872368,25.8954988194392,-13.7475086852288));
#58537=CARTESIAN_POINT('Ctrl Pts',(9.15291569757583,25.8321569688563,-14.0175513269118));
#58538=CARTESIAN_POINT('Ctrl Pts',(9.23744936372985,26.2598841203837,-13.6720799513866));
#58539=CARTESIAN_POINT('Ctrl Pts',(9.02989846070897,26.124492810673,-13.8123018789954));
#58540=CARTESIAN_POINT('Ctrl Pts',(9.06124675341241,26.054439739586,-14.0863858380353));
#58541=CARTESIAN_POINT('Ctrl Pts',(9.16522614835605,26.418146799207,-13.720699066088));
#58542=CARTESIAN_POINT('Ctrl Pts',(8.95760403593686,26.272189807985,-13.8593692962326));
#58543=CARTESIAN_POINT('Ctrl Pts',(8.99359966771377,26.1983148751026,-14.1364782535083));
#58544=CARTESIAN_POINT('Ctrl Pts',(9.04675320711485,26.6488731358305,-13.7988584568673));
#58545=CARTESIAN_POINT('Ctrl Pts',(8.8396384118494,26.4864000763885,-13.9346421962668));
#58546=CARTESIAN_POINT('Ctrl Pts',(8.88263328090294,26.4080660479035,-14.2170060986102));
#58547=CARTESIAN_POINT('Ctrl Pts',(9.00556864379736,26.724668077879,-13.8257853617022));
#58548=CARTESIAN_POINT('Ctrl Pts',(8.79856477912204,26.5568225974011,-13.9606137985784));
#58549=CARTESIAN_POINT('Ctrl Pts',(8.84405820972172,26.4769705271959,-14.2447489668247));
#58550=CARTESIAN_POINT('Ctrl Pts',(8.94125888839501,26.8367243925892,-13.8673912960299));
#58551=CARTESIAN_POINT('Ctrl Pts',(8.73458393580632,26.6606514330639,-14.0006470656152));
#58552=CARTESIAN_POINT('Ctrl Pts',(8.78382317974531,26.5788398835889,-14.287615680565));
#58553=CARTESIAN_POINT('Ctrl Pts',(8.91939992829263,26.8738036722238,-13.8814626371617));
#58554=CARTESIAN_POINT('Ctrl Pts',(8.71282066028938,26.6950205492259,-14.0141961613619));
#58555=CARTESIAN_POINT('Ctrl Pts',(8.76334922367439,26.6125483128922,-14.3021134241213));
#58556=CARTESIAN_POINT('Ctrl Pts',(8.87483584131177,26.947420683523,-13.9099960035042));
#58557=CARTESIAN_POINT('Ctrl Pts',(8.66847764979718,26.7631998723909,-14.0416544795966));
#58558=CARTESIAN_POINT('Ctrl Pts',(8.72160875835307,26.6794728551709,-14.3315114335205));
#58559=CARTESIAN_POINT('Ctrl Pts',(8.85211849071852,26.9839775314368,-13.9244657683607));
#58560=CARTESIAN_POINT('Ctrl Pts',(8.64588225815288,26.7970289078062,-14.0555729736903));
#58561=CARTESIAN_POINT('Ctrl Pts',(8.70033080036421,26.7127063466435,-14.34641967414));
#58562=CARTESIAN_POINT('Ctrl Pts',(8.73653994314236,27.1652095745738,-13.9976729904853));
#58563=CARTESIAN_POINT('Ctrl Pts',(8.5305769785088,26.9651990737812,-14.126204210908));
#58564=CARTESIAN_POINT('Ctrl Pts',(8.59207541474747,26.8774627173519,-14.4218452863613));
#58565=CARTESIAN_POINT('Ctrl Pts',(8.63857581146634,27.3039232901101,-14.0584339961704));
#58566=CARTESIAN_POINT('Ctrl Pts',(8.43329573465729,27.0929766694405,-14.184537001276));
#58567=CARTESIAN_POINT('Ctrl Pts',(8.50031838267292,27.0035660693995,-14.4844475260831));
#58568=CARTESIAN_POINT('Ctrl Pts',(8.43205452679184,27.5697679631042,-14.1832653127355));
#58569=CARTESIAN_POINT('Ctrl Pts',(8.22893898206923,27.336891173593,-14.303993073037));
#58570=CARTESIAN_POINT('Ctrl Pts',(8.30688247951664,27.245242992928,-14.6130615891751));
#58571=CARTESIAN_POINT('Ctrl Pts',(8.32349524991498,27.696895500351,-14.2473383251373));
#58572=CARTESIAN_POINT('Ctrl Pts',(8.12167890826586,27.4529918698611,-14.3651939112398));
#58573=CARTESIAN_POINT('Ctrl Pts',(8.20520162130922,27.3608134562285,-14.6790761982849));
#58574=CARTESIAN_POINT('Ctrl Pts',(8.0958209230527,27.940066659269,-14.3779312179124));
#58575=CARTESIAN_POINT('Ctrl Pts',(7.89760049643352,27.6740297912245,-14.4895090431896));
#58576=CARTESIAN_POINT('Ctrl Pts',(7.99195295573568,27.5818780963411,-14.8136264284226));
#58577=CARTESIAN_POINT('Ctrl Pts',(7.97670562766047,28.0561091060765,-14.4444528576548));
#58578=CARTESIAN_POINT('Ctrl Pts',(7.78060080854458,27.7789047025113,-14.5526858646747));
#58579=CARTESIAN_POINT('Ctrl Pts',(7.88038491947146,27.6873712051867,-14.8821638645775));
#58580=CARTESIAN_POINT('Ctrl Pts',(7.82103135401305,28.1943068383712,-14.5286861673289));
#58581=CARTESIAN_POINT('Ctrl Pts',(7.62904494836334,27.9025325222122,-14.63203155862));
#58582=CARTESIAN_POINT('Ctrl Pts',(7.73457431964004,27.8130054758372,-14.9689496818345));
#58583=CARTESIAN_POINT('Ctrl Pts',(7.78955667512429,28.2216027048998,-14.5455871841282));
#58584=CARTESIAN_POINT('Ctrl Pts',(7.598286999393,27.9270226975393,-14.6480127292069));
#58585=CARTESIAN_POINT('Ctrl Pts',(7.70509390682786,27.8378198938992,-14.9863628477604));
#58586=CARTESIAN_POINT('Ctrl Pts',(7.72591977577152,28.2755052515132,-14.579487760013));
#58587=CARTESIAN_POINT('Ctrl Pts',(7.53615718432266,27.9753071204984,-14.6800419075361));
#58588=CARTESIAN_POINT('Ctrl Pts',(7.6454891029661,27.8868221972088,-15.0212907073461));
#58589=CARTESIAN_POINT('Ctrl Pts',(7.69383664689685,28.3020444414061,-14.5964450623165));
#58590=CARTESIAN_POINT('Ctrl Pts',(7.50486038355863,27.9990389548318,-14.6960503341127));
#58591=CARTESIAN_POINT('Ctrl Pts',(7.61543879232438,27.9109487275864,-15.0387618643017));
#58592=CARTESIAN_POINT('Ctrl Pts',(7.5969094767131,28.3803480091191,-14.647262188812));
#58593=CARTESIAN_POINT('Ctrl Pts',(7.41024929743659,28.0690530186176,-14.7440600614543));
#58594=CARTESIAN_POINT('Ctrl Pts',(7.52465302114093,27.982133771713,-15.091118894199));
#58595=CARTESIAN_POINT('Ctrl Pts',(7.53133940020973,28.4308406046357,-14.681092957269));
#58596=CARTESIAN_POINT('Ctrl Pts',(7.34645413992588,28.1139578323579,-14.7759196021834));
#58597=CARTESIAN_POINT('Ctrl Pts',(7.46323752886183,28.0280361199399,-15.125974831266));
#58598=CARTESIAN_POINT('Ctrl Pts',(7.33178100387479,28.5773010543634,-14.782328694575));
#58599=CARTESIAN_POINT('Ctrl Pts',(7.1520743196714,28.2441717263217,-14.871402064795));
#58600=CARTESIAN_POINT('Ctrl Pts',(7.27632334582098,28.1611819502916,-15.2302782990676));
#58601=CARTESIAN_POINT('Ctrl Pts',(7.19495063365634,28.6682647836609,-14.849474803097));
#58602=CARTESIAN_POINT('Ctrl Pts',(7.01967189155258,28.3240420533312,-14.9343096208533));
#58603=CARTESIAN_POINT('Ctrl Pts',(7.1481626829883,28.2438762276959,-15.2994591252776));
#58604=CARTESIAN_POINT('Ctrl Pts',(6.9135955853759,28.8370962326483,-14.9825369223229));
#58605=CARTESIAN_POINT('Ctrl Pts',(6.74867575496167,28.4711445942248,-15.058566331689));
#58606=CARTESIAN_POINT('Ctrl Pts',(6.88463457001264,28.3973593211239,-15.4365534020641));
#58607=CARTESIAN_POINT('Ctrl Pts',(6.76907115430593,28.914963455736,-15.0484540472046));
#58608=CARTESIAN_POINT('Ctrl Pts',(6.61002452272855,28.5381997925323,-15.1198862928276));
#58609=CARTESIAN_POINT('Ctrl Pts',(6.74926735169343,28.4681476850395,-15.5044680022405));
#58610=CARTESIAN_POINT('Ctrl Pts',(6.47201687898309,29.0574380438273,-15.1785800066827));
#58611=CARTESIAN_POINT('Ctrl Pts',(6.32644002885306,28.6596820173027,-15.2405646922931));
#58612=CARTESIAN_POINT('Ctrl Pts',(6.4710347352573,28.5976699998072,-15.6385371439425));
#58613=CARTESIAN_POINT('Ctrl Pts',(6.3194882860113,29.1220469515791,-15.2427897294257));
#58614=CARTESIAN_POINT('Ctrl Pts',(6.18147732116283,28.7139248359103,-15.2998772546999));
#58615=CARTESIAN_POINT('Ctrl Pts',(6.32817050912569,28.656405351216,-15.70469260229));
#58616=CARTESIAN_POINT('Ctrl Pts',(6.12349203741434,29.1941487275923,-15.3217045706728));
#58617=CARTESIAN_POINT('Ctrl Pts',(5.99703656673586,28.7733421722218,-15.3722356540574));
#58618=CARTESIAN_POINT('Ctrl Pts',(6.14459278632615,28.721952398637,-15.7859987832458));
#58619=CARTESIAN_POINT('Ctrl Pts',(6.08402359052547,29.2081344154966,-15.3374205374095));
#58620=CARTESIAN_POINT('Ctrl Pts',(5.95976665824897,28.7848674248604,-15.3867016540606));
#58621=CARTESIAN_POINT('Ctrl Pts',(6.10762510082632,28.7346666559994,-15.8021909879922));
#58622=CARTESIAN_POINT('Ctrl Pts',(6.00481108118076,29.235136099283,-15.3686061720222));
#58623=CARTESIAN_POINT('Ctrl Pts',(5.88506002432616,28.8070167605749,-15.4153866452692));
#58624=CARTESIAN_POINT('Ctrl Pts',(6.03343157769096,28.7592136330259,-15.8343216346973));
#58625=CARTESIAN_POINT('Ctrl Pts',(5.96503423890355,29.2481644638745,-15.3840891406583));
#58626=CARTESIAN_POINT('Ctrl Pts',(5.84759340501311,28.8176478244873,-15.4296164975149));
#58627=CARTESIAN_POINT('Ctrl Pts',(5.99617503723461,28.7710575967267,-15.8502737807819));
#58628=CARTESIAN_POINT('Ctrl Pts',(5.84518801096566,29.285827922622,-15.4302010924098));
#58629=CARTESIAN_POINT('Ctrl Pts',(5.73467502532393,28.8482698420827,-15.4720336723545));
#58630=CARTESIAN_POINT('Ctrl Pts',(5.88392238984605,28.8052970930209,-15.8977830539599));
#58631=CARTESIAN_POINT('Ctrl Pts',(5.76460316441166,29.309042283798,-15.4604931073141));
#58632=CARTESIAN_POINT('Ctrl Pts',(5.65906122614119,28.8668766739417,-15.4998090557935));
#58633=CARTESIAN_POINT('Ctrl Pts',(5.80844348291024,28.8264010499212,-15.9289930019522));
#58634=CARTESIAN_POINT('Ctrl Pts',(5.6426748606603,29.3409890436428,-15.5052279766528));
#58635=CARTESIAN_POINT('Ctrl Pts',(5.54510753066133,28.8921201145448,-15.540725306626));
#58636=CARTESIAN_POINT('Ctrl Pts',(5.69424068407321,28.8554435481393,-15.9750834627829));
#58637=CARTESIAN_POINT('Ctrl Pts',(5.60185686122977,29.3511586098101,-15.5200224119935));
#58638=CARTESIAN_POINT('Ctrl Pts',(5.50695179331065,28.9001039225748,-15.5542677227203));
#58639=CARTESIAN_POINT('Ctrl Pts',(5.65600895573945,28.8646886046383,-15.9903262110367));
#58640=CARTESIAN_POINT('Ctrl Pts',(5.51986632851016,29.3705308152709,-15.5493720669948));
#58641=CARTESIAN_POINT('Ctrl Pts',(5.43040476978069,28.9151886717053,-15.5811202430405));
#58642=CARTESIAN_POINT('Ctrl Pts',(5.57921342901242,28.8822996938417,-16.0205652426492));
#58643=CARTESIAN_POINT('Ctrl Pts',(5.47867048511738,29.3797375986075,-15.5639351530272));
#58644=CARTESIAN_POINT('Ctrl Pts',(5.39199408493733,28.9222895153009,-15.5944358228649));
#58645=CARTESIAN_POINT('Ctrl Pts',(5.54062779747857,28.8906694935097,-16.0355696310093));
#58646=CARTESIAN_POINT('Ctrl Pts',(5.35495705072016,29.4058100316881,-15.607115874279));
#58647=CARTESIAN_POINT('Ctrl Pts',(5.27662176045004,28.9422275091807,-15.6339576546548));
#58648=CARTESIAN_POINT('Ctrl Pts',(5.42475297585001,28.9143716957695,-16.0800588491233));
#58649=CARTESIAN_POINT('Ctrl Pts',(5.27219555306174,29.4211589388003,-15.6352680825888));
#58650=CARTESIAN_POINT('Ctrl Pts',(5.19975787711073,28.9536492950679,-15.6596539110981));
#58651=CARTESIAN_POINT('Ctrl Pts',(5.3472353340361,28.9283252417574,-16.1090641481402));
#58652=CARTESIAN_POINT('Ctrl Pts',(5.02305213210112,29.4611376714299,-15.7178103797378));
#58653=CARTESIAN_POINT('Ctrl Pts',(4.96827292910735,28.9825980821897,-15.7351752246276));
#58654=CARTESIAN_POINT('Ctrl Pts',(5.11387790237459,28.9646695277837,-16.1941077084662));
#58655=CARTESIAN_POINT('Ctrl Pts',(4.8558120579994,29.4797132570353,-15.7702865042745));
#58656=CARTESIAN_POINT('Ctrl Pts',(4.81418315067994,28.9945338902948,-15.7829316553988));
#58657=CARTESIAN_POINT('Ctrl Pts',(4.95723433795089,28.9815564141466,-16.2481740063996));
#58658=CARTESIAN_POINT('Ctrl Pts',(4.51901742036134,29.5005364682645,-15.8700765191147));
#58659=CARTESIAN_POINT('Ctrl Pts',(4.50504494020981,29.0042572601608,-15.8739002545569));
#58660=CARTESIAN_POINT('Ctrl Pts',(4.64177936989425,29.0004865920627,-16.3509879384084));
#58661=CARTESIAN_POINT('Ctrl Pts',(4.3494629500257,29.502785301074,-15.9173905277554));
#58662=CARTESIAN_POINT('Ctrl Pts',(4.3502429631541,29.0019042207245,-15.9169948174607));
#58663=CARTESIAN_POINT('Ctrl Pts',(4.48296805417846,29.0025309794379,-16.399735694321));
#58664=CARTESIAN_POINT('Ctrl Pts',(4.09335666867169,29.4934411267723,-15.9844367581263));
#58665=CARTESIAN_POINT('Ctrl Pts',(4.11757727073345,28.9875429702007,-15.9781904236519));
#58666=CARTESIAN_POINT('Ctrl Pts',(4.24308894583155,28.9940362716043,-16.4688136139354));
#58667=CARTESIAN_POINT('Ctrl Pts',(4.00769193386057,29.488203178257,-16.0061312589015));
#58668=CARTESIAN_POINT('Ctrl Pts',(4.03976686665927,28.9809127305293,-15.9980533071268));
#58669=CARTESIAN_POINT('Ctrl Pts',(4.16285202190648,28.9892744987069,-16.4911655193356));
#58670=CARTESIAN_POINT('Ctrl Pts',(3.87874392389429,29.4770663983519,-16.0376838633684));
#58671=CARTESIAN_POINT('Ctrl Pts',(3.92291316792116,28.9681807792558,-16.0269890641618));
#58672=CARTESIAN_POINT('Ctrl Pts',(4.04207429867147,28.9791501531594,-16.5236742568235));
#58673=CARTESIAN_POINT('Ctrl Pts',(3.83568608727203,29.4728072307827,-16.0480365319683));
#58674=CARTESIAN_POINT('Ctrl Pts',(3.88389492951693,28.9634647647606,-16.0365012625793));
#58675=CARTESIAN_POINT('Ctrl Pts',(4.001744653625,28.9752781822712,-16.5343406406146));
#58676=CARTESIAN_POINT('Ctrl Pts',(3.77098556634597,29.4655837062055,-16.0633171833005));
#58677=CARTESIAN_POINT('Ctrl Pts',(3.82533008776607,28.955682491492,-16.0505552670575));
#58678=CARTESIAN_POINT('Ctrl Pts',(3.94114362844063,28.9687113421149,-16.5500843389504));
#58679=CARTESIAN_POINT('Ctrl Pts',(3.74939141393193,29.4630354881802,-16.0683712143744));
#58680=CARTESIAN_POINT('Ctrl Pts',(3.80578374002981,28.9529673365255,-16.0552084803821));
#58681=CARTESIAN_POINT('Ctrl Pts',(3.92091770513547,28.9663947803014,-16.5552915214721));
#58682=CARTESIAN_POINT('Ctrl Pts',(3.70628810723345,29.4576742045361,-16.0783680118345));
#58683=CARTESIAN_POINT('Ctrl Pts',(3.76678170918465,28.9473145341322,-16.0644192570448));
#58684=CARTESIAN_POINT('Ctrl Pts',(3.88054547112458,28.9615208862491,-16.5655912503298));
#58685=CARTESIAN_POINT('Ctrl Pts',(3.68476473814926,29.4548596671818,-16.083314174015));
#58686=CARTESIAN_POINT('Ctrl Pts',(3.74731382458174,28.9443751898187,-16.0689797247386));
#58687=CARTESIAN_POINT('Ctrl Pts',(3.86038584624321,28.9589622161346,-16.5706872952021));
#58688=CARTESIAN_POINT('Ctrl Pts',(3.49130865587881,29.4283277337408,-16.127363937821));
#58689=CARTESIAN_POINT('Ctrl Pts',(3.57193400752812,28.9168380011473,-16.1097329329338));
#58690=CARTESIAN_POINT('Ctrl Pts',(3.67918735214675,28.9348422779537,-16.6160718926013));
#58691=CARTESIAN_POINT('Ctrl Pts',(3.32115082183791,29.3962214040903,-16.1632103665466));
#58692=CARTESIAN_POINT('Ctrl Pts',(3.41868379435837,28.885249246741,-16.1429885986858));
#58693=CARTESIAN_POINT('Ctrl Pts',(3.51981090582723,28.905654709583,-16.6530045699382));
#58694=CARTESIAN_POINT('Ctrl Pts',(2.98447140597061,29.3151535083114,-16.2287504929071));
#58695=CARTESIAN_POINT('Ctrl Pts',(3.11558321115816,28.8079438698407,-16.2044649622416));
#58696=CARTESIAN_POINT('Ctrl Pts',(3.20446386879709,28.8319566350224,-16.7205307514468));
#58697=CARTESIAN_POINT('Ctrl Pts',(2.81794971294387,29.2661918358164,-16.2584434074366));
#58698=CARTESIAN_POINT('Ctrl Pts',(2.96606141020008,28.7622515268809,-16.2326005398578));
#58699=CARTESIAN_POINT('Ctrl Pts',(3.04849317455918,28.7874460320186,-16.7511234470313));
#58700=CARTESIAN_POINT('Ctrl Pts',(2.48868900652383,29.1511550976376,-16.3120890644351));
#58701=CARTESIAN_POINT('Ctrl Pts',(2.67017594325405,28.6563940412766,-16.284231703085));
#58702=CARTESIAN_POINT('Ctrl Pts',(2.74009479036264,28.6828672014999,-16.8063947256689));
#58703=CARTESIAN_POINT('Ctrl Pts',(2.32594930549035,29.0850820592773,-16.3360411540186));
#58704=CARTESIAN_POINT('Ctrl Pts',(2.52411048001744,28.5963080017393,-16.3076661076437));
#58705=CARTESIAN_POINT('Ctrl Pts',(2.58766645743185,28.6228008156417,-16.831072634431));
#58706=CARTESIAN_POINT('Ctrl Pts',(2.1250599072148,28.9913388786302,-16.3626331297301));
#58707=CARTESIAN_POINT('Ctrl Pts',(2.34344451308294,28.5116156314395,-16.3342596418995));
#58708=CARTESIAN_POINT('Ctrl Pts',(2.39950563332105,28.537579762439,-16.8584704278843));
#58709=CARTESIAN_POINT('Ctrl Pts',(2.08500913587358,28.9720313848574,-16.3677840722747));
#58710=CARTESIAN_POINT('Ctrl Pts',(2.30741972529226,28.4942013857767,-16.3394412041397));
#58711=CARTESIAN_POINT('Ctrl Pts',(2.36199252324546,28.5200274991674,-16.8637774595515));
#58712=CARTESIAN_POINT('Ctrl Pts',(2.0051675717704,28.9322819172796,-16.3777569142544));
#58713=CARTESIAN_POINT('Ctrl Pts',(2.23557690953715,28.458397994944,-16.3495362389501));
#58714=CARTESIAN_POINT('Ctrl Pts',(2.28720980878386,28.4838916282115,-16.8740525092714));
#58715=CARTESIAN_POINT('Ctrl Pts',(1.96554728119832,28.9119246509324,-16.3825574991731));
#58716=CARTESIAN_POINT('Ctrl Pts',(2.19991626407161,28.4400872660864,-16.3544276110724));
#58717=CARTESIAN_POINT('Ctrl Pts',(2.25009990362284,28.4653850267029,-16.8789985664897));
#58718=CARTESIAN_POINT('Ctrl Pts',(1.84762852982704,28.8494438636152,-16.3964183323368));
#58719=CARTESIAN_POINT('Ctrl Pts',(2.09374858695216,28.3839559804985,-16.3686452334824));
#58720=CARTESIAN_POINT('Ctrl Pts',(2.13965261480346,28.408584324102,-16.8932794261332));
#58721=CARTESIAN_POINT('Ctrl Pts',(1.77025016417281,28.8059015325617,-16.4049406057559));
#58722=CARTESIAN_POINT('Ctrl Pts',(2.0240311102136,28.3449272621931,-16.3775190668833));
#58723=CARTESIAN_POINT('Ctrl Pts',(2.06717702770033,28.369000396413,-16.9020599505988));
#58724=CARTESIAN_POINT('Ctrl Pts',(1.54177444682283,28.6696922285513,-16.4285233433696));
#58725=CARTESIAN_POINT('Ctrl Pts',(1.81802054001897,28.2230482321264,-16.4024562776685));
#58726=CARTESIAN_POINT('Ctrl Pts',(1.85317778430319,28.245173785856,-16.9263573205953));
#58727=CARTESIAN_POINT('Ctrl Pts',(1.39432796702046,28.5714557232892,-16.4416026489042));
#58728=CARTESIAN_POINT('Ctrl Pts',(1.68481012920359,28.1354202701133,-16.416850048029));
#58729=CARTESIAN_POINT('Ctrl Pts',(1.71507367590203,28.1558678938527,-16.9398329709249));
#58730=CARTESIAN_POINT('Ctrl Pts',(1.1091581197396,28.3602462452578,-16.4632990742983));
#58731=CARTESIAN_POINT('Ctrl Pts',(1.42630999988166,27.9469834669516,-16.4418103773245));
#58732=CARTESIAN_POINT('Ctrl Pts',(1.44797250333451,27.9638593241193,-16.9621868725179));
#58733=CARTESIAN_POINT('Ctrl Pts',(0.97143433369676,28.2472737238628,-16.4719148498968));
#58734=CARTESIAN_POINT('Ctrl Pts',(1.30115362468154,27.8463289268546,-16.4523713139938));
#58735=CARTESIAN_POINT('Ctrl Pts',(1.31897504755037,27.8611570567861,-16.9710637360526));
#58736=CARTESIAN_POINT('Ctrl Pts',(0.772335964035815,28.0665436198457,-16.4820482049561));
#58737=CARTESIAN_POINT('Ctrl Pts',(1.11938409554033,27.6848732656992,-16.4657595070228));
#58738=CARTESIAN_POINT('Ctrl Pts',(1.13249176716596,27.6968570019834,-16.9815041710235));
#58739=CARTESIAN_POINT('Ctrl Pts',(0.707219927244881,28.0044184229425,-16.4849604530816));
#58740=CARTESIAN_POINT('Ctrl Pts',(1.05990308308362,27.6294199257431,-16.4698065678274));
#58741=CARTESIAN_POINT('Ctrl Pts',(1.07150155369664,27.640379563638,-16.9845046714466));
#58742=CARTESIAN_POINT('Ctrl Pts',(0.627425661641159,27.9243604283892,-16.4880742390367));
#58743=CARTESIAN_POINT('Ctrl Pts',(0.986825074194957,27.5578383302768,-16.4743952087767));
#58744=CARTESIAN_POINT('Ctrl Pts',(0.996763139213813,27.5675995862004,-16.9877128184167));
#58745=CARTESIAN_POINT('Ctrl Pts',(0.611540473924973,27.9082218095615,-16.4886708677361));
#58746=CARTESIAN_POINT('Ctrl Pts',(0.972283286896175,27.5434186810164,-16.4752888037803));
#58747=CARTESIAN_POINT('Ctrl Pts',(0.981884454263182,27.5529281180705,-16.9883275273789));
#58748=CARTESIAN_POINT('Ctrl Pts',(0.580018327330572,27.8757931855677,-16.4898098071427));
#58749=CARTESIAN_POINT('Ctrl Pts',(0.943414684059886,27.5144388040394,-16.4770249256736));
#58750=CARTESIAN_POINT('Ctrl Pts',(0.952359585218988,27.5234475578251,-16.9895009817092));
#58751=CARTESIAN_POINT('Ctrl Pts',(0.564371283292323,27.8594932366258,-16.4903525315996));
#58752=CARTESIAN_POINT('Ctrl Pts',(0.9290786686879,27.4998699251214,-16.4778680690466));
#58753=CARTESIAN_POINT('Ctrl Pts',(0.937703954811051,27.5086294260622,-16.9900601529576));
#58754=CARTESIAN_POINT('Ctrl Pts',(0.517770310560036,27.8103379398031,-16.4919034726953));
#58755=CARTESIAN_POINT('Ctrl Pts',(0.886376806082585,27.4559394538946,-16.4803243487277));
#58756=CARTESIAN_POINT('Ctrl Pts',(0.894055670458409,27.4639428032576,-16.9916580947053));
#58757=CARTESIAN_POINT('Ctrl Pts',(0.487156485366989,27.777227184081,-16.4928344795921));
#58758=CARTESIAN_POINT('Ctrl Pts',(0.858291786859998,27.4263293129875,-16.4818659359195));
#58759=CARTESIAN_POINT('Ctrl Pts',(0.865381570302197,27.4338421235899,-16.992617315159));
#58760=CARTESIAN_POINT('Ctrl Pts',(0.336332590426369,27.6099874673847,-16.4970133717404));
#58761=CARTESIAN_POINT('Ctrl Pts',(0.720060538634519,27.2769753235213,-16.4891085915155));
#58762=CARTESIAN_POINT('Ctrl Pts',(0.724114041754052,27.2818060543167,-16.9969228486531));
#58763=CARTESIAN_POINT('Ctrl Pts',(0.222841397833277,27.470813335503,-16.4988386846704));
#58764=CARTESIAN_POINT('Ctrl Pts',(0.615458588915073,27.152300128901,-16.4934777845921));
#58765=CARTESIAN_POINT('Ctrl Pts',(0.617813773293677,27.1552841466947,-16.9988034793985));
#58766=CARTESIAN_POINT('Ctrl Pts',(0.00990321376705526,27.1819234494132,
-16.5003405467281));
#58767=CARTESIAN_POINT('Ctrl Pts',(0.418623080759106,26.8928768176219,-16.500034082667));
#58768=CARTESIAN_POINT('Ctrl Pts',(0.418367581724231,26.8926570393483,-17.0003508660311));
#58769=CARTESIAN_POINT('Ctrl Pts',(-0.0895433703373462,27.0322073820898,
-16.5000155646105));
#58770=CARTESIAN_POINT('Ctrl Pts',(0.326337742518627,26.7581881683623,-16.5022304055355));
#58771=CARTESIAN_POINT('Ctrl Pts',(0.325222039785076,26.7565515553554,-17.0000160414432));
#58772=CARTESIAN_POINT('Ctrl Pts',(-0.22808532752021,26.7996588451688,-16.4984881124101));
#58773=CARTESIAN_POINT('Ctrl Pts',(0.197300595381823,26.5482355425314,-16.5043570320983));
#58774=CARTESIAN_POINT('Ctrl Pts',(0.195458248265802,26.545143842926,-16.9984423127055));
#58775=CARTESIAN_POINT('Ctrl Pts',(-0.272491460913673,26.7208111901634,
-16.4978048280384));
#58776=CARTESIAN_POINT('Ctrl Pts',(0.155921684887115,26.4770642935037,-16.5048709970138));
#58777=CARTESIAN_POINT('Ctrl Pts',(0.153865735050095,26.4734641729081,-16.9977383254034));
#58778=CARTESIAN_POINT('Ctrl Pts',(-0.336397061068505,26.600511460516,-16.4965842207539));
#58779=CARTESIAN_POINT('Ctrl Pts',(0.096263783369711,26.3682980360483,-16.5054035854578));
#58780=CARTESIAN_POINT('Ctrl Pts',(0.0940092613899049,26.364100807324,-16.9964807347913));
#58781=CARTESIAN_POINT('Ctrl Pts',(-0.357248112372307,26.5600733475937,
-16.4961447004054));
#58782=CARTESIAN_POINT('Ctrl Pts',(0.0767954341642,26.3317400093734,-16.5055413589327));
#58783=CARTESIAN_POINT('Ctrl Pts',(0.0744793550369163,26.3273388947892,
-16.9960278969377));
#58784=CARTESIAN_POINT('Ctrl Pts',(-0.387841216089795,26.498903476538,-16.4954443177129));
#58785=CARTESIAN_POINT('Ctrl Pts',(0.0482046831755837,26.2763955006129,
-16.5056949266238));
#58786=CARTESIAN_POINT('Ctrl Pts',(0.0458246627006021,26.2717299338042,
-16.9953062928579));
#58787=CARTESIAN_POINT('Ctrl Pts',(-0.397929989940197,26.4784177145172,
-16.4952038798439));
#58788=CARTESIAN_POINT('Ctrl Pts',(0.0387756143308138,26.2578613891262,
-16.5057372758339));
#58789=CARTESIAN_POINT('Ctrl Pts',(0.0363751242704468,26.2531065180243,
-16.995058569621));
#58790=CARTESIAN_POINT('Ctrl Pts',(-0.41785522716858,26.4373219520784,-16.4947111621768));
#58791=CARTESIAN_POINT('Ctrl Pts',(0.020147303064918,26.2206715650669,-16.5058052567056));
#58792=CARTESIAN_POINT('Ctrl Pts',(0.0177123713203404,26.215746742428,-16.9945509226647));
#58793=CARTESIAN_POINT('Ctrl Pts',(-0.427682464432081,26.4167313372239,
-16.4944591218899));
#58794=CARTESIAN_POINT('Ctrl Pts',(0.0109564801403263,26.2020333124516,
-16.5058308763942));
#58795=CARTESIAN_POINT('Ctrl Pts',(0.00850779813750384,26.1970280059491,
-16.9942912454038));
#58796=CARTESIAN_POINT('Ctrl Pts',(-0.514916549790388,26.2310334534057,
-16.4921459441983));
#58797=CARTESIAN_POINT('Ctrl Pts',(-0.0704930411183981,26.0342333549254,
-16.5059913084747));
#58798=CARTESIAN_POINT('Ctrl Pts',(-0.0731990422494235,26.0282117868214,
-16.991907978272));
#58799=CARTESIAN_POINT('Ctrl Pts',(-0.583868202739844,26.0632566591539,
-16.4897780154229));
#58800=CARTESIAN_POINT('Ctrl Pts',(-0.135243030695479,25.8819909514499,
-16.5056453064897));
#58801=CARTESIAN_POINT('Ctrl Pts',(-0.137781846254395,25.8756874627897,
-16.9894682985939));
#58802=CARTESIAN_POINT('Ctrl Pts',(-0.705119344738234,25.7224378966208,
-16.4850383010123));
#58803=CARTESIAN_POINT('Ctrl Pts',(-0.249212478633839,25.5723054059926,
-16.5045205921069));
#58804=CARTESIAN_POINT('Ctrl Pts',(-0.251350387828509,25.5658522930326,
-16.98458496655));
#58805=CARTESIAN_POINT('Ctrl Pts',(-0.757417463412148,25.5493955100128,
-16.4826653704805));
#58806=CARTESIAN_POINT('Ctrl Pts',(-0.298533978119679,25.4147565405257,
-16.5037425494566));
#58807=CARTESIAN_POINT('Ctrl Pts',(-0.300334842855957,25.4085410670984,
-16.9821401326672));
#58808=CARTESIAN_POINT('Ctrl Pts',(-0.845380072148487,25.1980454046336,
-16.4783880116582));
#58809=CARTESIAN_POINT('Ctrl Pts',(-0.381512922806825,25.0945912805061,
-16.5021755819352));
#58810=CARTESIAN_POINT('Ctrl Pts',(-0.382724048673311,25.0891319505675,
-16.9777331645216));
#58811=CARTESIAN_POINT('Ctrl Pts',(-0.88104566901821,25.0197380423049,-16.4764831102671));
#58812=CARTESIAN_POINT('Ctrl Pts',(-0.415254760524545,24.9318357068706,
-16.5013859883012));
#58813=CARTESIAN_POINT('Ctrl Pts',(-0.416129835547799,24.9270343835225,
-16.9757705414227));
#58814=CARTESIAN_POINT('Ctrl Pts',(-0.911543766590598,24.8160928395057,
-16.4748019557039));
#58815=CARTESIAN_POINT('Ctrl Pts',(-0.44411885392913,24.7457485251799,-16.5006631669498));
#58816=CARTESIAN_POINT('Ctrl Pts',(-0.444695542276101,24.7419024208988,
-16.9740384454876));
#58817=CARTESIAN_POINT('Ctrl Pts',(-0.914798413228078,24.7934231348861,
-16.4746215017785));
#58818=CARTESIAN_POINT('Ctrl Pts',(-0.447197123951018,24.7250475825129,
-16.5005851404517));
#58819=CARTESIAN_POINT('Ctrl Pts',(-0.447743970993952,24.7212936029764,
-16.9738525234988));
#58820=CARTESIAN_POINT('Ctrl Pts',(-0.921038106174053,24.7479983123345,
-16.4742738404667));
#58821=CARTESIAN_POINT('Ctrl Pts',(-0.453099183041882,24.6835643674665,
-16.5004340097327));
#58822=CARTESIAN_POINT('Ctrl Pts',(-0.453588310581765,24.6799983187254,
-16.9734943275512));
#58823=CARTESIAN_POINT('Ctrl Pts',(-0.924024713623736,24.7252305558544,
-16.4741065451602));
#58824=CARTESIAN_POINT('Ctrl Pts',(-0.455924553911642,24.6627702033824,
-16.5003608644188));
#58825=CARTESIAN_POINT('Ctrl Pts',(-0.456385683463281,24.6593003627783,
-16.9733219629078));
#58826=CARTESIAN_POINT('Ctrl Pts',(-0.932566535330723,24.6568879141791,
-16.4736259575042));
#58827=CARTESIAN_POINT('Ctrl Pts',(-0.464005080455623,24.6003531735753,
-16.5001497685869));
#58828=CARTESIAN_POINT('Ctrl Pts',(-0.464386286247165,24.5971707019928,
-16.9728268127538));
#58829=CARTESIAN_POINT('Ctrl Pts',(-0.93769515390498,24.6113486125014,-16.4733344755913));
#58830=CARTESIAN_POINT('Ctrl Pts',(-0.468858612305496,24.558750101885,-16.5000203424063));
#58831=CARTESIAN_POINT('Ctrl Pts',(-0.46918995040038,24.5557713458215,-16.9725264984295));
#58832=CARTESIAN_POINT('Ctrl Pts',(-0.951402889619917,24.4747973150587,
-16.4725503892664));
#58833=CARTESIAN_POINT('Ctrl Pts',(-0.481829948120828,24.4340092880389,
-16.4996699330201));
#58834=CARTESIAN_POINT('Ctrl Pts',(-0.482029149367011,24.4316338295858,
-16.9717186531439));
#58835=CARTESIAN_POINT('Ctrl Pts',(-0.958304970217346,24.3838519341024,
-16.4721484267205));
#58836=CARTESIAN_POINT('Ctrl Pts',(-0.488366769549358,24.3508831821315,
-16.4994869083559));
#58837=CARTESIAN_POINT('Ctrl Pts',(-0.488493906800559,24.3489562298645,
-16.9713045105041));
#58838=CARTESIAN_POINT('Ctrl Pts',(-0.963009452978601,24.2929936995252,
-16.4718733844551));
#58839=CARTESIAN_POINT('Ctrl Pts',(-0.492822054870804,24.2678247304756,
-16.4993612048297));
#58840=CARTESIAN_POINT('Ctrl Pts',(-0.492900308952224,24.2663578511416,
-16.9710211339658));
#58841=CARTESIAN_POINT('Origin',(-0.976753528407678,24.4999999958215,-16.9714356779612));
#58842=CARTESIAN_POINT('Ctrl Pts',(6.78574855947051,19.4906334205529,-15.2493774847029));
#58843=CARTESIAN_POINT('Ctrl Pts',(7.09365200449485,19.6230994530404,-15.0579941028986));
#58844=CARTESIAN_POINT('Ctrl Pts',(7.39169961590562,19.7784989217241,-14.8605142516318));
#58845=CARTESIAN_POINT('Ctrl Pts',(7.96341514878726,20.1269516722891,-14.4823196206633));
#58846=CARTESIAN_POINT('Ctrl Pts',(8.24170752937464,20.3223222055852,-14.2982311601103));
#58847=CARTESIAN_POINT('Ctrl Pts',(8.51515294794751,20.5398470862767,-14.1330198635429));
#58848=CARTESIAN_POINT('Ctrl Pts',(8.51772116533781,20.5418925937812,-14.1314696945114));
#58849=CARTESIAN_POINT('Ctrl Pts',(8.52036854006083,20.5440034843838,-14.1298733170473));
#58850=CARTESIAN_POINT('Origin',(-0.976758640922575,23.4999998309184,-16.9714360885196));
#58851=CARTESIAN_POINT('Origin',(-27.5,23.5,-23.));
#58852=CARTESIAN_POINT('',(-27.5,23.5,-23.));
#58853=CARTESIAN_POINT('',(-27.5,24.5,-23.));
#58854=CARTESIAN_POINT('Origin',(1.59198825996909E-15,23.5,4.71469806142367E-15));
#58855=CARTESIAN_POINT('Origin',(-36.5,3.36766747301154E-16,-24.));
#58856=CARTESIAN_POINT('',(-36.5,49.3978607591793,-24.5));
#58857=CARTESIAN_POINT('',(-36.5,54.4282032302755,-24.5));
#58858=CARTESIAN_POINT('Origin',(-36.5000000000003,50.0331217848142,-24.0000000000004));
#58859=CARTESIAN_POINT('Origin',(-37.5,41.9220413888134,-36.7681064455182));
#58860=CARTESIAN_POINT('',(-37.5,49.6110803960012,-23.7318935544818));
#58861=CARTESIAN_POINT('Origin',(-37.5,50.0331217848147,-24.));
#58862=CARTESIAN_POINT('',(-37.5,41.5,-36.5));
#58863=CARTESIAN_POINT('Ctrl Pts',(-37.4999999984477,49.6111157620785,-23.7318378827565));
#58864=CARTESIAN_POINT('Ctrl Pts',(-36.999945703858,49.6111031628287,-23.7318577159421));
#58865=CARTESIAN_POINT('Ctrl Pts',(-37.0000000019487,50.0331903787841,-23.9999932725221));
#58866=CARTESIAN_POINT('Ctrl Pts',(-37.5000026475399,49.5809381372911,-23.7793421740157));
#58867=CARTESIAN_POINT('Ctrl Pts',(-37.0125257432584,49.5919210538653,-23.7620533492161));
#58868=CARTESIAN_POINT('Ctrl Pts',(-37.0000003236668,50.0030123006108,-24.0237451732358));
#58869=CARTESIAN_POINT('Ctrl Pts',(-37.4966146037487,49.5507607813308,-23.8268460420991));
#58870=CARTESIAN_POINT('Ctrl Pts',(-37.0226617091426,49.5716751064898,-23.7939236301844));
#58871=CARTESIAN_POINT('Ctrl Pts',(-36.9983053346281,49.9728345473706,-24.0474967093262));
#58872=CARTESIAN_POINT('Ctrl Pts',(-37.4831283980406,49.491028778915,-23.9208735363186));
#58873=CARTESIAN_POINT('Ctrl Pts',(-37.0369947679708,49.5303132082949,-23.8590337133256));
#58874=CARTESIAN_POINT('Ctrl Pts',(-36.9915604437569,49.9131017946599,-24.0945094462342));
#58875=CARTESIAN_POINT('Ctrl Pts',(-37.4730329455306,49.4614743777896,-23.967396776267));
#58876=CARTESIAN_POINT('Ctrl Pts',(-37.0413371805881,49.5091937801452,-23.8922789893572));
#58877=CARTESIAN_POINT('Ctrl Pts',(-36.9865118906715,49.8835470446703,-24.1177704508956));
#58878=CARTESIAN_POINT('Ctrl Pts',(-37.446338975696,49.4035751035746,-24.0585392702631));
#58879=CARTESIAN_POINT('Ctrl Pts',(-37.0439552690129,49.4668675528739,-23.9589070769676));
#58880=CARTESIAN_POINT('Ctrl Pts',(-36.9731634448554,49.8256471127136,-24.1633403049858));
#58881=CARTESIAN_POINT('Ctrl Pts',(-37.429740631672,49.3752306064593,-24.1031579324689));
#58882=CARTESIAN_POINT('Ctrl Pts',(-37.0423583210133,49.4456316816316,-23.9923356526007));
#58883=CARTESIAN_POINT('Ctrl Pts',(-36.9648636339063,49.7973023126176,-24.1856488539623));
#58884=CARTESIAN_POINT('Ctrl Pts',(-37.390377073182,49.3203254093101,-24.1895872818758));
#58885=CARTESIAN_POINT('Ctrl Pts',(-37.0332157434799,49.4038164073336,-24.0581594204861));
#58886=CARTESIAN_POINT('Ctrl Pts',(-36.9451808008242,49.7423965456869,-24.2288618610315));
#58887=CARTESIAN_POINT('Ctrl Pts',(-37.3676121138729,49.2937650652586,-24.231397408705));
#58888=CARTESIAN_POINT('Ctrl Pts',(-37.0257725875086,49.3831899562253,-24.0906286737161));
#58889=CARTESIAN_POINT('Ctrl Pts',(-36.9337979027379,49.7158359419089,-24.2497660334815));
#58890=CARTESIAN_POINT('Ctrl Pts',(-37.3163764581199,49.2429663043523,-24.311362586571));
#58891=CARTESIAN_POINT('Ctrl Pts',(-37.0052677332731,49.3432758528686,-24.1534597018221));
#58892=CARTESIAN_POINT('Ctrl Pts',(-36.9081794773421,49.6650366944085,-24.289746799377));
#58893=CARTESIAN_POINT('Ctrl Pts',(-37.287906093082,49.2187282161604,-24.3495171202411));
#58894=CARTESIAN_POINT('Ctrl Pts',(-36.9922786439071,49.3239297683643,-24.1839134581893));
#58895=CARTESIAN_POINT('Ctrl Pts',(-36.8939441137087,49.6407983870913,-24.308823128154));
#58896=CARTESIAN_POINT('Ctrl Pts',(-37.2258363558164,49.173065055751,-24.4213980614082));
#58897=CARTESIAN_POINT('Ctrl Pts',(-36.9611889277236,49.2871849199918,-24.2417555843231));
#58898=CARTESIAN_POINT('Ctrl Pts',(-36.8629091218297,49.5951348186603,-24.3447617436394));
#58899=CARTESIAN_POINT('Ctrl Pts',(-37.1922373840171,49.1516402781994,-24.455124005055));
#58900=CARTESIAN_POINT('Ctrl Pts',(-36.9431292563272,49.2697227239588,-24.2692438062169));
#58901=CARTESIAN_POINT('Ctrl Pts',(-36.8461096933389,49.5737098600968,-24.3616237923194));
#58902=CARTESIAN_POINT('Ctrl Pts',(-37.1205910755058,49.1120378371204,-24.517464428095));
#58903=CARTESIAN_POINT('Ctrl Pts',(-36.9025509928616,49.2372711703841,-24.3203276162804));
#58904=CARTESIAN_POINT('Ctrl Pts',(-36.8102868777744,49.534107085388,-24.3927922372483));
#58905=CARTESIAN_POINT('Ctrl Pts',(-37.0825441996165,49.0938604283893,-24.5460785063992));
#58906=CARTESIAN_POINT('Ctrl Pts',(-36.8800425170188,49.2222192372126,-24.3440217082585));
#58907=CARTESIAN_POINT('Ctrl Pts',(-36.791263722181,49.5159295315503,-24.4070984271328));
#58908=CARTESIAN_POINT('Ctrl Pts',(-37.0027728479139,49.061121037485,-24.5976154173431));
#58909=CARTESIAN_POINT('Ctrl Pts',(-36.8313364551817,49.1950237103828,-24.3868317119147));
#58910=CARTESIAN_POINT('Ctrl Pts',(-36.7513788065511,49.4831898778153,-24.4328653160013));
#58911=CARTESIAN_POINT('Ctrl Pts',(-36.9610488835586,49.0465592652919,-24.6205379194415));
#58912=CARTESIAN_POINT('Ctrl Pts',(-36.8051210511832,49.182823514119,-24.4060367249271));
#58913=CARTESIAN_POINT('Ctrl Pts',(-36.7305173047078,49.4686279945608,-24.4443258445491));
#58914=CARTESIAN_POINT('Ctrl Pts',(-36.8747686270439,49.0213462124955,-24.6602271995625));
#58915=CARTESIAN_POINT('Ctrl Pts',(-36.7498616197956,49.1616716404749,-24.4393330752317));
#58916=CARTESIAN_POINT('Ctrl Pts',(-36.6873782930618,49.443414746811,-24.4641692147401));
#58917=CARTESIAN_POINT('Ctrl Pts',(-36.8302128863916,49.0106950931136,-24.6769937237974));
#58918=CARTESIAN_POINT('Ctrl Pts',(-36.7207763816884,49.1526735677021,-24.4534974461114));
#58919=CARTESIAN_POINT('Ctrl Pts',(-36.6651010626569,49.4327635489392,-24.4725519253));
#58920=CARTESIAN_POINT('Ctrl Pts',(-36.7391717313683,48.9935191854961,-24.7040312830438));
#58921=CARTESIAN_POINT('Ctrl Pts',(-36.6607031513577,49.1381669860886,-24.4763330696242));
#58922=CARTESIAN_POINT('Ctrl Pts',(-36.6195818726028,49.4155875120346,-24.4860698090038));
#58923=CARTESIAN_POINT('Ctrl Pts',(-36.6926868974402,48.9869945068099,-24.7143021456072));
#58924=CARTESIAN_POINT('Ctrl Pts',(-36.6296563273817,49.1326255446801,-24.4850561632574));
#58925=CARTESIAN_POINT('Ctrl Pts',(-36.5963402077165,49.409062786363,-24.4912048929667));
#58926=CARTESIAN_POINT('Ctrl Pts',(-36.5987293041569,48.9782037218442,-24.7281402131275));
#58927=CARTESIAN_POINT('Ctrl Pts',(-36.5666266668979,49.1251717354285,-24.4967896223414));
#58928=CARTESIAN_POINT('Ctrl Pts',(-36.5493629685859,49.4002719362922,-24.4981234586691));
#58929=CARTESIAN_POINT('Ctrl Pts',(-36.5512571427956,48.9759376715364,-24.7317073299761));
#58930=CARTESIAN_POINT('Ctrl Pts',(-36.5345740079014,49.1232421108123,-24.499827152645));
#58931=CARTESIAN_POINT('Ctrl Pts',(-36.5256276984433,49.3980058698557,-24.4999068948091));
#58932=CARTESIAN_POINT('Ctrl Pts',(-36.4562866573806,48.9757101072324,-24.7320655517066));
#58933=CARTESIAN_POINT('Ctrl Pts',(-36.4705163089246,49.123048899448,-24.5001312974868));
#58934=CARTESIAN_POINT('Ctrl Pts',(-36.4781440730316,49.3977783038758,-24.500085993473));
#58935=CARTESIAN_POINT('Ctrl Pts',(-36.4087889373822,48.9777485946843,-24.7288566543092));
#58936=CARTESIAN_POINT('Ctrl Pts',(-36.43843759609,49.1247848624327,-24.4973986208165));
#58937=CARTESIAN_POINT('Ctrl Pts',(-36.4543960250934,49.3998168058322,-24.4984816548169));
#58938=CARTESIAN_POINT('Ctrl Pts',(-36.3147296267512,48.9860888614095,-24.7157277728121));
#58939=CARTESIAN_POINT('Ctrl Pts',(-36.3753047257849,49.1318576224222,-24.4862649927414));
#58940=CARTESIAN_POINT('Ctrl Pts',(-36.4073679332755,49.4081571342912,-24.4919176584518));
#58941=CARTESIAN_POINT('Ctrl Pts',(-36.2681686347218,48.992390587583,-24.7058078723002));
#58942=CARTESIAN_POINT('Ctrl Pts',(-36.3441803599222,49.1372108049169,-24.4778382480196));
#58943=CARTESIAN_POINT('Ctrl Pts',(-36.3840881938228,49.4144589058036,-24.4869580440036));
#58944=CARTESIAN_POINT('Ctrl Pts',(-36.1769261057559,49.0091297146586,-24.6794578737954));
#58945=CARTESIAN_POINT('Ctrl Pts',(-36.2839031722063,49.1513523853739,-24.4555771932943));
#58946=CARTESIAN_POINT('Ctrl Pts',(-36.338468328439,49.4311981587367,-24.473783919146));
#58947=CARTESIAN_POINT('Ctrl Pts',(-36.1322451504778,49.0195670088094,-24.6630279438459));
#58948=CARTESIAN_POINT('Ctrl Pts',(-36.2546907643748,49.1601729318861,-24.4416922764546));
#58949=CARTESIAN_POINT('Ctrl Pts',(-36.3161284979174,49.4416355296862,-24.4655694956441));
#58950=CARTESIAN_POINT('Ctrl Pts',(-36.0456679431823,49.0443658677742,-24.6239906694594));
#58951=CARTESIAN_POINT('Ctrl Pts',(-36.1991315589116,49.1809863110149,-24.4089287693469));
#58952=CARTESIAN_POINT('Ctrl Pts',(-36.2728410275264,49.4664345800778,-24.4460521102632));
#58953=CARTESIAN_POINT('Ctrl Pts',(-36.003772244485,49.0587272740393,-24.601383574603));
#58954=CARTESIAN_POINT('Ctrl Pts',(-36.1727424636104,49.1930248987828,-24.3899781533289));
#58955=CARTESIAN_POINT('Ctrl Pts',(-36.2518936680164,49.480796095646,-24.4347492773044));
#58956=CARTESIAN_POINT('Ctrl Pts',(-35.9236143812708,49.0910834492376,-24.5504499049892));
#58957=CARTESIAN_POINT('Ctrl Pts',(-36.1236482291063,49.2199185380588,-24.3476433677986));
#58958=CARTESIAN_POINT('Ctrl Pts',(-36.2118155173364,49.5131525300135,-24.4092839956601));
#58959=CARTESIAN_POINT('Ctrl Pts',(-35.8853531222871,49.1090777974647,-24.5221239924888));
#58960=CARTESIAN_POINT('Ctrl Pts',(-36.1009245697621,49.2348292308243,-24.3241716102623));
#58961=CARTESIAN_POINT('Ctrl Pts',(-36.1926854283368,49.5311467527012,-24.395122094762));
#58962=CARTESIAN_POINT('Ctrl Pts',(-35.8492954555149,49.1287069943377,-24.4912245730675));
#58963=CARTESIAN_POINT('Ctrl Pts',(-36.0805222911065,49.2508329082794,-24.2989793242432));
#58964=CARTESIAN_POINT('Ctrl Pts',(-36.1746565192972,49.5507763940651,-24.3796730443644));
#58965=CARTESIAN_POINT('',(-35.8596780097302,49.1231323091022,-24.4999999976734));
#58966=CARTESIAN_POINT('Ctrl Pts',(-35.8596780097302,49.1231323076242,-24.5));
#58967=CARTESIAN_POINT('Ctrl Pts',(-35.8897007194235,49.1231323141072,-24.5));
#58968=CARTESIAN_POINT('Ctrl Pts',(-35.9492795917087,49.12628580103,-24.5));
#58969=CARTESIAN_POINT('Ctrl Pts',(-36.0079619111141,49.1354984450364,-24.5));
#58970=CARTESIAN_POINT('Ctrl Pts',(-36.0516397569449,49.1446647887917,-24.5));
#58971=CARTESIAN_POINT('Ctrl Pts',(-36.0733950255041,49.1498133203893,-24.5));
#58972=CARTESIAN_POINT('Ctrl Pts',(-36.1022332978191,49.1578185056805,-24.5));
#58973=CARTESIAN_POINT('Ctrl Pts',(-36.116596336941,49.1622047284401,-24.5));
#58974=CARTESIAN_POINT('Ctrl Pts',(-36.1522448462494,49.1735909724898,-24.5));
#58975=CARTESIAN_POINT('Ctrl Pts',(-36.1800852563754,49.1840820076817,-24.5));
#58976=CARTESIAN_POINT('Ctrl Pts',(-36.2344635854011,49.2077175303379,-24.5));
#58977=CARTESIAN_POINT('Ctrl Pts',(-36.2610010813319,49.2208628794797,-24.5));
#58978=CARTESIAN_POINT('Ctrl Pts',(-36.3127941023519,49.2497652256379,-24.5));
#58979=CARTESIAN_POINT('Ctrl Pts',(-36.3380490893341,49.2655233188928,-24.5));
#58980=CARTESIAN_POINT('Ctrl Pts',(-36.3688173582917,49.2868516528285,-24.5));
#58981=CARTESIAN_POINT('Ctrl Pts',(-36.3749341691932,49.2912014358321,-24.5));
#58982=CARTESIAN_POINT('Ctrl Pts',(-36.3870418406883,49.3000299236013,-24.5));
#58983=CARTESIAN_POINT('Ctrl Pts',(-36.4050308157833,49.3134769801761,-24.5));
#58984=CARTESIAN_POINT('Ctrl Pts',(-36.4341648250175,49.3368925485922,-24.5));
#58985=CARTESIAN_POINT('Ctrl Pts',(-36.4622110995748,49.3615962902832,-24.5));
#58986=CARTESIAN_POINT('Ctrl Pts',(-36.4812975745014,49.3795354237726,-24.5));
#58987=CARTESIAN_POINT('Ctrl Pts',(-36.4907080161569,49.3886622568197,-24.5));
#58988=CARTESIAN_POINT('Ctrl Pts',(-36.4947130222966,49.3926069640088,-24.5));
#58989=CARTESIAN_POINT('Ctrl Pts',(-36.4973768431774,49.3952440914044,-24.5));
#58990=CARTESIAN_POINT('Ctrl Pts',(-36.4986848184451,49.3965508641444,-24.5));
#58991=CARTESIAN_POINT('Ctrl Pts',(-36.5,49.3978607591793,-24.5));
#58992=CARTESIAN_POINT('Origin',(-36.4999950467498,49.6110877386296,-23.7318819960386));
#58993=CARTESIAN_POINT('Origin',(-50.,38.1236688894923,-34.3551484358543));
#58994=CARTESIAN_POINT('',(-45.2221315177632,44.0220106908928,-25.0702378819582));
#58995=CARTESIAN_POINT('',(-10.,39.7323075626015,-31.8229001029736));
#58996=CARTESIAN_POINT('',(-10.,39.7323075626015,-31.8229001029736));
#58997=CARTESIAN_POINT('',(-10.,38.1236688894923,-34.3551484358543));
#58998=CARTESIAN_POINT('Origin',(6.61363325216158E-15,52.,24.));
#58999=CARTESIAN_POINT('',(-3.43565291283912,52.,26.90625));
#59000=CARTESIAN_POINT('',(-3.43565291283912,52.,26.90625));
#59001=CARTESIAN_POINT('',(-27.1034840901754,52.,1.07291666666665));
#59002=CARTESIAN_POINT('',(-11.,52.,24.));
#59003=CARTESIAN_POINT('',(-6.,52.,-16.7705098312484));
#59004=CARTESIAN_POINT('Origin',(-5.,52.,-16.7705098312484));
#59005=CARTESIAN_POINT('',(-6.,52.,-23.8747810831708));
#59006=CARTESIAN_POINT('',(-6.,52.,-12.1904119063322));
#59007=CARTESIAN_POINT('',(-27.1034840901754,52.,1.07291666666665));
#59008=CARTESIAN_POINT('',(15.2695685015073,52.,-12.9166666666667));
#59009=CARTESIAN_POINT('',(27.1034840901754,52.,1.07291666666666));
#59010=CARTESIAN_POINT('',(15.2695685015073,52.,12.9166666666666));
#59011=CARTESIAN_POINT('Origin',(6.61287431064084E-15,52.,0.));
#59012=CARTESIAN_POINT('',(3.43565291283914,52.,26.90625));
#59013=CARTESIAN_POINT('',(3.43565291283914,52.,26.90625));
#59014=CARTESIAN_POINT('Origin',(6.61363325216158E-15,52.,24.));
#59015=CARTESIAN_POINT('Origin',(-50.,41.5,-36.5));
#59016=CARTESIAN_POINT('Origin',(-50.,-2.17497943900684,-3.42375708761853));
#59017=CARTESIAN_POINT('Origin',(-6.,3.67381906146713E-16,1.84889274661174E-32));
#59018=CARTESIAN_POINT('',(-6.,40.2323075626015,-16.7705098312484));
#59019=CARTESIAN_POINT('',(-6.,3.67381906146713E-16,-16.7705098312484));
#59020=CARTESIAN_POINT('',(-6.,40.2323075626015,1.46930375624346E-14));
#59021=CARTESIAN_POINT('',(-6.,52.0032753870454,-24.));
#59022=CARTESIAN_POINT('',(-6.,3.67381906146713E-16,-24.));
#59023=CARTESIAN_POINT('Origin',(-6.00000000000972,54.3934990501575,-23.8748259395246));
#59024=CARTESIAN_POINT('Origin',(-50.,3.67381906146713E-16,1.84889274661174E-32));
#59025=CARTESIAN_POINT('Origin',(-50.,3.67381906146713E-16,1.84889274661174E-32));
#59026=CARTESIAN_POINT('',(-50.,40.4835859155314,-25.7842093518926));
#59027=CARTESIAN_POINT('Origin',(1.59198825996909E-15,24.5,4.71469806142367E-15));
#59028=CARTESIAN_POINT('Origin',(-50.,51.6880449296918,-20.4624272250886));
#59029=CARTESIAN_POINT('Origin',(-10.,39.7323075626015,-31.8229001029736));
#59030=CARTESIAN_POINT('',(-6.5,39.7323075626015,-16.2480768092719));
#59031=CARTESIAN_POINT('',(-6.5,39.7323075626015,-31.8229001029736));
#59032=CARTESIAN_POINT('',(-10.,39.7323075626015,-14.3614066163451));
#59033=CARTESIAN_POINT('Origin',(6.61363325216158E-15,39.7323075626015,
1.23256668029931E-15));
#59034=CARTESIAN_POINT('',(-10.,39.7323075626015,-31.8229001029736));
#59035=CARTESIAN_POINT('Origin',(-45.2221315177632,40.4835859155314,-25.7842093518926));
#59036=CARTESIAN_POINT('Origin',(-4.19913133791448,57.,-27.5520833333334));
#59037=CARTESIAN_POINT('',(-4.19913133791448,53.,-27.5520833333334));
#59038=CARTESIAN_POINT('',(-6.78091634720693,53.,-24.5));
#59039=CARTESIAN_POINT('',(-4.19913133791448,53.,-27.5520833333334));
#59040=CARTESIAN_POINT('',(-6.78091634720693,57.,-24.5));
#59041=CARTESIAN_POINT('Origin',(-10.,3.67381906146713E-16,0.));
#59042=CARTESIAN_POINT('',(-10.,39.5242048993244,-13.6106575888162));
#59043=CARTESIAN_POINT('Ctrl Pts',(-10.,39.7323075626015,-14.3614066163451));
#59044=CARTESIAN_POINT('Ctrl Pts',(-10.,39.7323075626015,-14.200398990526));
#59045=CARTESIAN_POINT('Ctrl Pts',(-10.,39.699502446739,-14.009995208009));
#59046=CARTESIAN_POINT('Ctrl Pts',(-10.,39.6147673433497,-13.7776180829596));
#59047=CARTESIAN_POINT('Ctrl Pts',(-10.,39.5738101323051,-13.6904818142623));
#59048=CARTESIAN_POINT('Ctrl Pts',(-10.,39.5242048993244,-13.6106575888162));
#59049=CARTESIAN_POINT('',(-10.,51.,-13.6106575888162));
#59050=CARTESIAN_POINT('',(-10.,3.67381906146713E-16,-13.6106575888162));
#59051=CARTESIAN_POINT('',(-10.,51.,0.));
#59052=CARTESIAN_POINT('Origin',(-10.,45.4641016151378,-17.5));
#59053=CARTESIAN_POINT('Ctrl Pts',(16.2770594071445,26.117084953911,2.70320865940617));
#59054=CARTESIAN_POINT('Ctrl Pts',(16.1847747722226,25.1844547539906,3.25888995310305));
#59055=CARTESIAN_POINT('Ctrl Pts',(17.2635478560624,25.2642374615925,3.38919957270747));
#59056=CARTESIAN_POINT('Ctrl Pts',(16.2967231208785,26.0401987677082,2.58480587333236));
#59057=CARTESIAN_POINT('Ctrl Pts',(16.2046985714116,25.1219174064774,3.16392715346833));
#59058=CARTESIAN_POINT('Ctrl Pts',(17.2844032861437,25.2001657110687,3.28455076234357));
#59059=CARTESIAN_POINT('Ctrl Pts',(16.3146546406934,25.9585491601778,2.46884251835106));
#59060=CARTESIAN_POINT('Ctrl Pts',(16.2234217236847,25.0559444309027,3.07071608610299));
#59061=CARTESIAN_POINT('Ctrl Pts',(17.303421588318,25.1321242999822,3.18205778145459));
#59062=CARTESIAN_POINT('Ctrl Pts',(16.3473809405565,25.7855724308805,2.24193572830452));
#59063=CARTESIAN_POINT('Ctrl Pts',(16.2586774276057,24.9166403886353,2.88760736217028));
#59064=CARTESIAN_POINT('Ctrl Pts',(17.3381313008865,24.9879770258997,2.98150885069049));
#59065=CARTESIAN_POINT('Ctrl Pts',(16.3621754499714,25.694246003057,2.13099201606505));
#59066=CARTESIAN_POINT('Ctrl Pts',(16.2751973635875,24.8433767087607,2.79778198770337));
#59067=CARTESIAN_POINT('Ctrl Pts',(17.353822446655,24.9118716689619,2.88345253963371));
#59068=CARTESIAN_POINT('Ctrl Pts',(16.3788998863479,25.5738507355765,1.99559089989728));
#59069=CARTESIAN_POINT('Ctrl Pts',(16.2945840207838,24.7468003055873,2.68754694707923));
#59070=CARTESIAN_POINT('Ctrl Pts',(17.3715604855917,24.8115422797102,2.76377983572222));
#59071=CARTESIAN_POINT('Ctrl Pts',(16.382158257244,25.5494440782525,1.9686582620157));
#59072=CARTESIAN_POINT('Ctrl Pts',(16.2983964036959,24.727243668477,2.66561253202148));
#59073=CARTESIAN_POINT('Ctrl Pts',(17.375016333334,24.7912033985914,2.73997573657795));
#59074=CARTESIAN_POINT('Ctrl Pts',(16.3884940923374,25.5000673076495,1.91519865899398));
#59075=CARTESIAN_POINT('Ctrl Pts',(16.3058846588611,24.6876852903887,2.62202284398017));
#59076=CARTESIAN_POINT('Ctrl Pts',(17.3817361586463,24.7500560896602,2.69272608754677));
#59077=CARTESIAN_POINT('Ctrl Pts',(16.3915654053909,25.4751465153454,1.88872442372019));
#59078=CARTESIAN_POINT('Ctrl Pts',(16.3095531288558,24.6677240764023,2.60041130993974));
#59079=CARTESIAN_POINT('Ctrl Pts',(17.3849936116739,24.7292887628288,2.66932714213006));
#59080=CARTESIAN_POINT('Ctrl Pts',(16.4005017546482,25.3996926651759,1.81006291261778));
#59081=CARTESIAN_POINT('Ctrl Pts',(16.3203356992417,24.6073073367928,2.53613976226817));
#59082=CARTESIAN_POINT('Ctrl Pts',(17.3944715581686,24.6664105542314,2.59980307942765));
#59083=CARTESIAN_POINT('Ctrl Pts',(16.4060893408832,25.3484683787228,1.75863656568711));
#59084=CARTESIAN_POINT('Ctrl Pts',(16.3272331794214,24.5662888812604,2.49400781955273));
#59085=CARTESIAN_POINT('Ctrl Pts',(17.4003977855862,24.6237236489918,2.55435049990395));
#59086=CARTESIAN_POINT('Ctrl Pts',(16.4218345582109,25.1920672215291,1.60736737169908));
#59087=CARTESIAN_POINT('Ctrl Pts',(16.3470874651384,24.4410877110629,2.36984780965278));
#59088=CARTESIAN_POINT('Ctrl Pts',(17.4170972591065,24.493389351162,2.42065298018113));
#59089=CARTESIAN_POINT('Ctrl Pts',(16.4309764402636,25.0841657011645,1.51053038267463));
#59090=CARTESIAN_POINT('Ctrl Pts',(16.3592331968953,24.3546376676092,2.28990440593928));
#59091=CARTESIAN_POINT('Ctrl Pts',(17.4267931938554,24.4034714176583,2.33506473211196));
#59092=CARTESIAN_POINT('Ctrl Pts',(16.446994092363,24.8611997872063,1.3247921132227));
#59093=CARTESIAN_POINT('Ctrl Pts',(16.3815748016209,24.1756367993131,2.13577662546436));
#59094=CARTESIAN_POINT('Ctrl Pts',(17.4437816134758,24.2176664893174,2.17090212032256));
#59095=CARTESIAN_POINT('Ctrl Pts',(16.4538694171321,24.7461353014014,1.23589090041249));
#59096=CARTESIAN_POINT('Ctrl Pts',(16.3917723398782,24.0831327303185,2.06160077217661));
#59097=CARTESIAN_POINT('Ctrl Pts',(17.4510736238994,24.1217794177785,2.09232781607564));
#59098=CARTESIAN_POINT('Ctrl Pts',(16.4657444941948,24.5088324285203,1.06606911860916));
#59099=CARTESIAN_POINT('Ctrl Pts',(16.41043203463,23.8918442069889,1.91919542169583));
#59100=CARTESIAN_POINT('Ctrl Pts',(17.4636684032655,23.924027023823,1.94223280679702));
#59101=CARTESIAN_POINT('Ctrl Pts',(16.4707439330845,24.3865942689554,0.985148265534012));
#59102=CARTESIAN_POINT('Ctrl Pts',(16.4188978329588,23.7930962833668,1.85095941313437));
#59103=CARTESIAN_POINT('Ctrl Pts',(17.4689708378186,23.8221618906762,1.87071185102215));
#59104=CARTESIAN_POINT('Ctrl Pts',(16.4770987515012,24.1977602110029,0.869883576612304));
#59105=CARTESIAN_POINT('Ctrl Pts',(16.430448838457,23.6399653599251,1.75322510898323));
#59106=CARTESIAN_POINT('Ctrl Pts',(17.4757107971974,23.6648001758957,1.76883649439488));
#59107=CARTESIAN_POINT('Ctrl Pts',(16.4790260107452,24.1339017821622,0.832482487139682));
#59108=CARTESIAN_POINT('Ctrl Pts',(16.4341038189509,23.588155056693,1.72145552621991));
#59109=CARTESIAN_POINT('Ctrl Pts',(17.4777548597382,23.611584818395,1.73577997612498));
#59110=CARTESIAN_POINT('Ctrl Pts',(16.481660834336,24.0367224738724,0.777937966978324));
#59111=CARTESIAN_POINT('Ctrl Pts',(16.439316110871,23.5091625905436,1.67499684370208));
#59112=CARTESIAN_POINT('Ctrl Pts',(17.4805493698219,23.5306020615971,1.68757143540179));
#59113=CARTESIAN_POINT('Ctrl Pts',(16.4824963319283,24.0040971394492,0.76001668658966));
#59114=CARTESIAN_POINT('Ctrl Pts',(16.4410074506687,23.4826353866685,1.65971950289981));
#59115=CARTESIAN_POINT('Ctrl Pts',(17.4814355034805,23.5034142828847,1.67173191994441));
#59116=CARTESIAN_POINT('Ctrl Pts',(16.4840825264792,23.9385710072358,0.724799252308877));
#59117=CARTESIAN_POINT('Ctrl Pts',(16.4442928704461,23.4293188181548,1.62966302113361));
#59118=CARTESIAN_POINT('Ctrl Pts',(17.483117831194,23.4488091726861,1.64060539978915));
#59119=CARTESIAN_POINT('Ctrl Pts',(16.4848338838812,23.9056467056935,0.707489718603382));
#59120=CARTESIAN_POINT('Ctrl Pts',(16.4458883265545,23.402510427123,1.61487200588415));
#59121=CARTESIAN_POINT('Ctrl Pts',(17.4839147252516,23.4213722547508,1.6253065694588));
#59122=CARTESIAN_POINT('Ctrl Pts',(16.4883963136533,23.7402209980604,0.622434816921749));
#59123=CARTESIAN_POINT('Ctrl Pts',(16.4536288557431,23.2678810456568,1.54219914855875));
#59124=CARTESIAN_POINT('Ctrl Pts',(17.4876930602432,23.2835174983592,1.5501317826884));
#59125=CARTESIAN_POINT('Ctrl Pts',(16.4906265194978,23.6053104048751,0.559161466617183));
#59126=CARTESIAN_POINT('Ctrl Pts',(16.4591061096903,23.1576407614143,1.48778409749428));
#59127=CARTESIAN_POINT('Ctrl Pts',(17.4900584295061,23.1710920040299,1.49420836702546));
#59128=CARTESIAN_POINT('Ctrl Pts',(16.4928461382771,23.43345704006,0.486045567387642));
#59129=CARTESIAN_POINT('Ctrl Pts',(16.4651843052487,23.0166721910829,1.4246163879437));
#59130=CARTESIAN_POINT('Ctrl Pts',(17.492412570966,23.0278808667248,1.42958572873525));
#59131=CARTESIAN_POINT('Ctrl Pts',(16.4932615496334,23.3989227879446,0.47172051602756));
#59132=CARTESIAN_POINT('Ctrl Pts',(16.4663600202752,22.988357063806,1.4122411370019));
#59133=CARTESIAN_POINT('Ctrl Pts',(17.4928531586321,22.9991023233164,1.41692469843949));
#59134=CARTESIAN_POINT('Ctrl Pts',(16.4940398122447,23.32954199818,0.443674950772383));
#59135=CARTESIAN_POINT('Ctrl Pts',(16.4686366864973,22.9314333971575,1.38799006257673));
#59136=CARTESIAN_POINT('Ctrl Pts',(17.4936785888143,22.9412849984541,1.39213695150995));
#59137=CARTESIAN_POINT('Ctrl Pts',(16.4944018726065,23.2947668025916,0.42998321641532));
#59138=CARTESIAN_POINT('Ctrl Pts',(16.4697353860784,22.9028829800878,1.37613850024778));
#59139=CARTESIAN_POINT('Ctrl Pts',(17.494062592092,22.912305668851,1.3800356710121));
#59140=CARTESIAN_POINT('Ctrl Pts',(16.4954144797531,23.19018912733,0.389892224755595));
#59141=CARTESIAN_POINT('Ctrl Pts',(16.4729170185102,22.8170009119346,1.34141701125129));
#59142=CARTESIAN_POINT('Ctrl Pts',(17.4951365695679,22.825157606059,1.34460171392323));
#59143=CARTESIAN_POINT('Ctrl Pts',(16.4959915982081,23.1201346539405,0.364476810515272));
#59144=CARTESIAN_POINT('Ctrl Pts',(16.4748883009626,22.7593742589264,1.31935155897431));
#59145=CARTESIAN_POINT('Ctrl Pts',(17.4957486646468,22.766778878317,1.32213859505898));
#59146=CARTESIAN_POINT('Ctrl Pts',(16.4974846918856,22.908978123431,0.292108636005814));
#59147=CARTESIAN_POINT('Ctrl Pts',(16.480387411174,22.585590732172,1.25646842577618));
#59148=CARTESIAN_POINT('Ctrl Pts',(17.4973322492083,22.5908151027927,1.25817682493942));
#59149=CARTESIAN_POINT('Ctrl Pts',(16.4981644144038,22.7668843481313,0.249028531548178));
#59150=CARTESIAN_POINT('Ctrl Pts',(16.4835124139739,22.4682695938112,1.21884858897264));
#59151=CARTESIAN_POINT('Ctrl Pts',(17.498053166605,22.4724036234601,1.2201009747895));
#59152=CARTESIAN_POINT('Ctrl Pts',(16.4991365090799,22.4800959201519,0.173028058336329));
#59153=CARTESIAN_POINT('Ctrl Pts',(16.4888528045335,22.2310570860755,1.15235685094956));
#59154=CARTESIAN_POINT('Ctrl Pts',(17.4990841764838,22.2334132667759,1.15292883950236));
#59155=CARTESIAN_POINT('Ctrl Pts',(16.4994286224241,22.3354012063648,0.140107924718887));
#59156=CARTESIAN_POINT('Ctrl Pts',(16.4910714022229,22.1111134362735,1.12345029266905));
#59157=CARTESIAN_POINT('Ctrl Pts',(17.4993939933432,22.1128343386246,1.12383276180865));
#59158=CARTESIAN_POINT('Ctrl Pts',(16.4998074835914,22.0434113899889,0.0844280845233825));
#59159=CARTESIAN_POINT('Ctrl Pts',(16.4947342938488,21.8687662112482,1.07450481854977));
#59160=CARTESIAN_POINT('Ctrl Pts',(17.4997958160672,21.8695094916702,1.07462078171355));
#59161=CARTESIAN_POINT('Ctrl Pts',(16.4998941390599,21.8961163485439,0.0616681376515486));
#59162=CARTESIAN_POINT('Ctrl Pts',(16.4961809127729,21.7463003703735,1.0544381008806));
#59163=CARTESIAN_POINT('Ctrl Pts',(17.4998877231583,21.7467636237625,1.05450466730936));
#59164=CARTESIAN_POINT('Ctrl Pts',(16.4999646344616,21.6731910279211,0.0352767822043904));
#59165=CARTESIAN_POINT('Ctrl Pts',(16.4978347597081,21.5607763684425,1.03115602986482));
#59166=CARTESIAN_POINT('Ctrl Pts',(17.4999624911392,21.5609925232796,1.031178974074));
#59167=CARTESIAN_POINT('Ctrl Pts',(16.4999777889481,21.5985517799239,0.0277724453695535));
#59168=CARTESIAN_POINT('Ctrl Pts',(16.4982997216056,21.4986420637007,1.0245316792856));
#59169=CARTESIAN_POINT('Ctrl Pts',(17.499976442793,21.4987931499252,1.02454635336124));
#59170=CARTESIAN_POINT('Ctrl Pts',(16.4999899371909,21.4860893308933,0.0184840127014977));
#59171=CARTESIAN_POINT('Ctrl Pts',(16.4988720208443,21.4049879523016,1.01633002306669));
#59172=CARTESIAN_POINT('Ctrl Pts',(17.499989327339,21.4050744424167,1.01633687984765));
#59173=CARTESIAN_POINT('Ctrl Pts',(16.4999926953601,21.448517894679,0.0157159728075137));
#59174=CARTESIAN_POINT('Ctrl Pts',(16.4990419025216,21.3736970698179,1.01388537562505));
#59175=CARTESIAN_POINT('Ctrl Pts',(17.4999922526425,21.3737649122275,1.01389038008064));
#59176=CARTESIAN_POINT('Ctrl Pts',(16.4999966178257,21.3732055924448,0.0108420698560791));
#59177=CARTESIAN_POINT('Ctrl Pts',(16.4993402987244,21.3109670684979,1.00958040502331));
#59178=CARTESIAN_POINT('Ctrl Pts',(17.4999964128575,21.3110046603757,1.00958263742506));
#59179=CARTESIAN_POINT('Ctrl Pts',(16.4999977775395,21.3355743663222,0.00874340271113735));
#59180=CARTESIAN_POINT('Ctrl Pts',(16.4994683856541,21.2796180343658,1.00772626682737));
#59181=CARTESIAN_POINT('Ctrl Pts',(17.499997642836,21.2796453052717,1.0077277548556));
#59182=CARTESIAN_POINT('Ctrl Pts',(16.5000015057495,21.1476258471459,-6.83792717788806E-5));
#59183=CARTESIAN_POINT('Ctrl Pts',(16.5000052077858,21.1230590208582,0.999941955565308));
#59184=CARTESIAN_POINT('Ctrl Pts',(17.5000015970427,21.1230215392753,0.999939564038385));
#59185=CARTESIAN_POINT('Ctrl Pts',(16.5000002892947,20.9978414168731,-0.00175010211135428));
#59186=CARTESIAN_POINT('Ctrl Pts',(16.5001062656831,20.9981824204012,0.998453734603185));
#59187=CARTESIAN_POINT('Ctrl Pts',(17.5000003068456,20.9982011807243,0.998453192447992));
#59188=CARTESIAN_POINT('Ctrl Pts',(16.4999995141463,20.6993924312047,0.00535189244501871));
#59189=CARTESIAN_POINT('Ctrl Pts',(16.499675246758,20.7494912128809,1.00473020199914));
#59190=CARTESIAN_POINT('Ctrl Pts',(17.4999994846828,20.7494936926738,1.00473020809944));
#59191=CARTESIAN_POINT('Ctrl Pts',(16.4999998611331,20.5507279300157,0.0141361157985634));
#59192=CARTESIAN_POINT('Ctrl Pts',(16.4991427830948,20.6255982356581,1.01249911380526));
#59193=CARTESIAN_POINT('Ctrl Pts',(17.4999998527873,20.6256066083462,1.01249404173988));
#59194=CARTESIAN_POINT('Ctrl Pts',(16.4999522523993,20.2545094474017,0.0420822492766633));
#59195=CARTESIAN_POINT('Ctrl Pts',(16.4974126080831,20.379000809699,1.03716536090374));
#59196=CARTESIAN_POINT('Ctrl Pts',(17.4999493585349,20.378757872835,1.03719390719024));
#59197=CARTESIAN_POINT('Ctrl Pts',(16.4999043691725,20.106955309657,0.0612441917327677));
#59198=CARTESIAN_POINT('Ctrl Pts',(16.49621379071,20.2562217364147,1.05407787581568));
#59199=CARTESIAN_POINT('Ctrl Pts',(17.4998985730686,20.255796045571,1.05412997524387));
#59200=CARTESIAN_POINT('Ctrl Pts',(16.4997777634116,19.9599613252167,0.0856373635093353));
#59201=CARTESIAN_POINT('Ctrl Pts',(16.494639994887,20.1341916960038,1.07553284116397));
#59202=CARTESIAN_POINT('Ctrl Pts',(17.4997642945274,20.1333011043472,1.07568958896027));
#59203=CARTESIAN_POINT('',(16.5375681109059,20.0478523395152,0.351922735556661));
#59204=CARTESIAN_POINT('Ctrl Pts',(17.4999100362562,20.3177786532602,1.04676003808511));
#59205=CARTESIAN_POINT('Ctrl Pts',(17.497412412154,20.317337698044,1.04682077239613));
#59206=CARTESIAN_POINT('Ctrl Pts',(17.4949148321613,20.3168954823132,1.0468722967329));
#59207=CARTESIAN_POINT('Ctrl Pts',(17.4924172962765,20.316452006012,1.04691461131551));
#59208=CARTESIAN_POINT('Ctrl Pts',(17.4915847843149,20.3163041805782,1.04692871617638));
#59209=CARTESIAN_POINT('Ctrl Pts',(17.490762085069,20.3161579632937,1.04694165678216));
#59210=CARTESIAN_POINT('Ctrl Pts',(17.489917898285,20.3160077756803,1.04695388308451));
#59211=CARTESIAN_POINT('Ctrl Pts',(17.4865411511487,20.3154070252269,1.04700278829394));
#59212=CARTESIAN_POINT('Ctrl Pts',(17.4831669066207,20.3148043885298,1.04703482418623));
#59213=CARTESIAN_POINT('Ctrl Pts',(17.4797951548174,20.3141998724626,1.04705005790662));
#59214=CARTESIAN_POINT('Ctrl Pts',(17.4730516512108,20.3129908403283,1.0470805253474));
#59215=CARTESIAN_POINT('Ctrl Pts',(17.4663181182136,20.3117742914819,1.04704378959848));
#59216=CARTESIAN_POINT('Ctrl Pts',(17.4595944841994,20.3105502727928,1.04694032080793));
#59217=CARTESIAN_POINT('Ctrl Pts',(17.446147216171,20.3081022354146,1.04673338322681));
#59218=CARTESIAN_POINT('Ctrl Pts',(17.4327395412199,20.3056243303144,1.04625959729685));
#59219=CARTESIAN_POINT('Ctrl Pts',(17.4193710601051,20.3031168246039,1.04552169141653));
#59220=CARTESIAN_POINT('Ctrl Pts',(17.3926340978756,20.2981018131829,1.0440458796559));
#59221=CARTESIAN_POINT('Ctrl Pts',(17.3660537227381,20.2929685399409,1.04151486242535));
#59222=CARTESIAN_POINT('Ctrl Pts',(17.3396290846692,20.287717410052,1.03793473510459));
#59223=CARTESIAN_POINT('Ctrl Pts',(17.3132044466002,20.2824662801631,1.03435460778383));
#59224=CARTESIAN_POINT('Ctrl Pts',(17.2869355447269,20.2770972972993,1.02972539672272));
#59225=CARTESIAN_POINT('Ctrl Pts',(17.2608245587767,20.2716085915521,1.02403256038389));
#59226=CARTESIAN_POINT('Ctrl Pts',(17.2477690658017,20.2688642386785,1.02118614221447));
#59227=CARTESIAN_POINT('Ctrl Pts',(17.234753135717,20.2660899091362,1.01807350559858));
#59228=CARTESIAN_POINT('Ctrl Pts',(17.2217772917725,20.2632851599956,1.01469078953784));
#59229=CARTESIAN_POINT('Ctrl Pts',(17.2152893698003,20.2618827854253,1.01299943150747));
#59230=CARTESIAN_POINT('Ctrl Pts',(17.2088052768564,20.2604714323889,1.01123870857771));
#59231=CARTESIAN_POINT('Ctrl Pts',(17.20235370637,20.2590573280976,1.009416302857));
#59232=CARTESIAN_POINT('Ctrl Pts',(17.1959021358836,20.2576432238063,1.0075938971363));
#59233=CARTESIAN_POINT('Ctrl Pts',(17.1894803216323,20.2562257911111,1.00570923654773));
#59234=CARTESIAN_POINT('Ctrl Pts',(17.1830880283661,20.2548050536997,1.00376281463061));
#59235=CARTESIAN_POINT('Ctrl Pts',(17.1575188553016,20.249122104054,0.99597712696212));
#59236=CARTESIAN_POINT('Ctrl Pts',(17.1324212808169,20.2433863569365,0.987204804132461));
#59237=CARTESIAN_POINT('Ctrl Pts',(17.1077863027231,20.2375986909455,0.977464745590708));
#59238=CARTESIAN_POINT('Ctrl Pts',(17.0831513246293,20.2318110249545,0.967724687048955));
#59239=CARTESIAN_POINT('Ctrl Pts',(17.0589789712759,20.225971430241,0.957016828161272));
#59240=CARTESIAN_POINT('Ctrl Pts',(17.0352693339654,20.2200798256262,0.945341032704729));
#59241=CARTESIAN_POINT('Ctrl Pts',(17.0115596966549,20.2141882210115,0.933665237248187));
#59242=CARTESIAN_POINT('Ctrl Pts',(16.988312746797,20.2082446154472,0.921021563266389));
#59243=CARTESIAN_POINT('Ctrl Pts',(16.9655376048733,20.2022479693789,0.907390857660355));
#59244=CARTESIAN_POINT('Ctrl Pts',(16.9541500339115,20.1992496463448,0.900575504857338));
#59245=CARTESIAN_POINT('Ctrl Pts',(16.9428805950743,20.1962380202549,0.893513121755632));
#59246=CARTESIAN_POINT('Ctrl Pts',(16.9317313026216,20.1932128989287,0.886199374602489));
#59247=CARTESIAN_POINT('Ctrl Pts',(16.9261566563953,20.1917003382657,0.882542501025918));
#59248=CARTESIAN_POINT('Ctrl Pts',(16.9206120585836,20.1901844007644,0.878822767087584));
#59249=CARTESIAN_POINT('Ctrl Pts',(16.9150978270253,20.1886650515396,0.875039504162688));
#59250=CARTESIAN_POINT('Ctrl Pts',(16.9095835954671,20.1871457023148,0.871256241237792));
#59251=CARTESIAN_POINT('Ctrl Pts',(16.9041070265371,20.1856249264553,0.867414287379847));
#59252=CARTESIAN_POINT('Ctrl Pts',(16.8986841658931,20.184107238926,0.863525316408129));
#59253=CARTESIAN_POINT('Ctrl Pts',(16.8769927233169,20.1780364888088,0.847969432521257));
#59254=CARTESIAN_POINT('Ctrl Pts',(16.8560810285277,20.1719935559081,0.831609081359371));
#59255=CARTESIAN_POINT('Ctrl Pts',(16.835932407024,20.1659779433814,0.814461434518674));
#59256=CARTESIAN_POINT('Ctrl Pts',(16.8157837855203,20.1599623308546,0.797313787677976));
#59257=CARTESIAN_POINT('Ctrl Pts',(16.796398295399,20.153974028425,0.779378781668851));
#59258=CARTESIAN_POINT('Ctrl Pts',(16.7777743700881,20.1480131320867,0.76065799712203));
#59259=CARTESIAN_POINT('Ctrl Pts',(16.7591504447772,20.1420522357484,0.741937212575208));
#59260=CARTESIAN_POINT('Ctrl Pts',(16.7412880466671,20.1361187517238,0.722430687544411));
#59261=CARTESIAN_POINT('Ctrl Pts',(16.7242005076968,20.1302133641119,0.702124551441759));
#59262=CARTESIAN_POINT('Ctrl Pts',(16.7156567382117,20.127260670306,0.691971483390434));
#59263=CARTESIAN_POINT('Ctrl Pts',(16.7073069447631,20.1243149669166,0.681618309087091));
#59264=CARTESIAN_POINT('Ctrl Pts',(16.6991542585567,20.1213764519223,0.67106171344245));
#59265=CARTESIAN_POINT('Ctrl Pts',(16.6950779154534,20.1199071944251,0.665783415620129));
#59266=CARTESIAN_POINT('Ctrl Pts',(16.6910508666661,20.1184397316079,0.660454247788119));
#59267=CARTESIAN_POINT('Ctrl Pts',(16.6870736074572,20.1169740855827,0.65507369560794));
#59268=CARTESIAN_POINT('Ctrl Pts',(16.6830963482483,20.1155084395574,0.649693143427761));
#59269=CARTESIAN_POINT('Ctrl Pts',(16.6791647000557,20.1140430113909,0.644255147297184));
#59270=CARTESIAN_POINT('Ctrl Pts',(16.6752988732391,20.1125852953334,0.638787354378224));
#59271=CARTESIAN_POINT('Ctrl Pts',(16.6598355659724,20.1067544311035,0.616916182702385));
#59272=CARTESIAN_POINT('Ctrl Pts',(16.6453887468324,20.1010345149467,0.594526308078098));
#59273=CARTESIAN_POINT('Ctrl Pts',(16.6319321474346,20.095422943538,0.571631075588535));
#59274=CARTESIAN_POINT('Ctrl Pts',(16.6184755480369,20.0898113721293,0.548735843098972));
#59275=CARTESIAN_POINT('Ctrl Pts',(16.6060092707311,20.084308135995,0.525335196488614));
#59276=CARTESIAN_POINT('Ctrl Pts',(16.594527070435,20.0789128413188,0.501432270733023));
#59277=CARTESIAN_POINT('Ctrl Pts',(16.583044870139,20.0735175466426,0.477529344977431));
#59278=CARTESIAN_POINT('Ctrl Pts',(16.572546719852,20.0682301946996,0.453124147417704));
#59279=CARTESIAN_POINT('Ctrl Pts',(16.5630457927051,20.0630525023684,0.428209898952689));
#59280=CARTESIAN_POINT('Ctrl Pts',(16.5535448655582,20.0578748100371,0.403295650487674));
#59281=CARTESIAN_POINT('Ctrl Pts',(16.54504099411,20.0528067872061,0.377872409037217));
#59282=CARTESIAN_POINT('Ctrl Pts',(16.5375681503014,20.0478524311852,0.35192279925056));
#59283=CARTESIAN_POINT('Ctrl Pts',(16.4999922300468,20.5440053495025,0.0163638449572259));
#59284=CARTESIAN_POINT('Ctrl Pts',(16.4999770343612,20.5198614768197,0.0316719654762678));
#59285=CARTESIAN_POINT('Ctrl Pts',(16.5002263989813,20.4961497241895,0.0468431030935451));
#59286=CARTESIAN_POINT('Ctrl Pts',(16.5020179270435,20.412886263937,0.100672073666557));
#59287=CARTESIAN_POINT('Ctrl Pts',(16.5049029406463,20.3540801618161,0.139580047345334));
#59288=CARTESIAN_POINT('Ctrl Pts',(16.5156498028587,20.2121142842092,0.235607659679802));
#59289=CARTESIAN_POINT('Ctrl Pts',(16.5251347070846,20.1294122583419,0.29333516665824));
#59290=CARTESIAN_POINT('Ctrl Pts',(16.5375680971716,20.0478522665949,0.351922636958438));
#59291=CARTESIAN_POINT('Ctrl Pts',(16.4260332126742,25.1379309164222,1.56059122805689));
#59292=CARTESIAN_POINT('Ctrl Pts',(16.4226910805317,25.1576364103843,1.59576908821006));
#59293=CARTESIAN_POINT('Ctrl Pts',(16.4195841592766,25.176720276254,1.62999587635092));
#59294=CARTESIAN_POINT('Ctrl Pts',(16.4010380336176,25.2940925947309,1.84168171849569));
#59295=CARTESIAN_POINT('Ctrl Pts',(16.3882950542161,25.3896976994372,2.01860511761247));
#59296=CARTESIAN_POINT('Ctrl Pts',(16.3564248514291,25.5987026766223,2.41684917061561));
#59297=CARTESIAN_POINT('Ctrl Pts',(16.3372998166613,25.7068837309083,2.63036802356939));
#59298=CARTESIAN_POINT('Ctrl Pts',(16.3099522015712,25.8138525750283,2.84895274231535));
#59299=CARTESIAN_POINT('Ctrl Pts',(12.0866114872764,19.9820083891277,11.2322670354491));
#59300=CARTESIAN_POINT('Ctrl Pts',(12.3807269288992,20.0835512235879,10.9157806962192));
#59301=CARTESIAN_POINT('Ctrl Pts',(12.8191333955962,20.1516736576064,10.9275087434525));
#59302=CARTESIAN_POINT('Ctrl Pts',(12.0675878268092,20.1081184594252,11.2527376663919));
#59303=CARTESIAN_POINT('Ctrl Pts',(12.3622278967634,20.1967330860491,10.9367605323266));
#59304=CARTESIAN_POINT('Ctrl Pts',(12.7989568015267,20.2567653007514,10.9456014580243));
#59305=CARTESIAN_POINT('Ctrl Pts',(12.0519050645098,20.2355538181535,11.2695119158229));
#59306=CARTESIAN_POINT('Ctrl Pts',(12.3469366141942,20.3114015985704,10.9539972243665));
#59307=CARTESIAN_POINT('Ctrl Pts',(12.7823235531825,20.3629615151636,10.9604271979261));
#59308=CARTESIAN_POINT('Ctrl Pts',(12.0337154085966,20.4287937461634,11.288922538981));
#59309=CARTESIAN_POINT('Ctrl Pts',(12.3292036429553,20.4853989396882,10.9739392026073));
#59310=CARTESIAN_POINT('Ctrl Pts',(12.7630314940089,20.5239947884517,10.9775830523308));
#59311=CARTESIAN_POINT('Ctrl Pts',(12.0285416186745,20.4935550919164,11.2944333696097));
#59312=CARTESIAN_POINT('Ctrl Pts',(12.3241592547639,20.5437171707118,10.9796013224493));
#59313=CARTESIAN_POINT('Ctrl Pts',(12.757544140988,20.5779625766115,10.9824537355451));
#59314=CARTESIAN_POINT('Ctrl Pts',(12.0221588199083,20.5912338278851,11.3012259052763));
#59315=CARTESIAN_POINT('Ctrl Pts',(12.3179359141494,20.6317011591869,10.9865804526371));
#59316=CARTESIAN_POINT('Ctrl Pts',(12.7507745059785,20.6593615232303,10.9884572396224));
#59317=CARTESIAN_POINT('Ctrl Pts',(12.0202608919841,20.6238828763539,11.3032444010669));
#59318=CARTESIAN_POINT('Ctrl Pts',(12.3160853794008,20.6611104736368,10.9886544060349));
#59319=CARTESIAN_POINT('Ctrl Pts',(12.7487615520924,20.6865690636343,10.9902412634538));
#59320=CARTESIAN_POINT('Ctrl Pts',(12.0177642067175,20.6729926478103,11.3058986793241));
#59321=CARTESIAN_POINT('Ctrl Pts',(12.3136509329996,20.7053522841239,10.9913817152174));
#59322=CARTESIAN_POINT('Ctrl Pts',(12.7461135525852,20.7274938731722,10.9925872166321));
#59323=CARTESIAN_POINT('Ctrl Pts',(12.0169904627187,20.6893850602612,11.3067210676687));
#59324=CARTESIAN_POINT('Ctrl Pts',(12.3128964800711,20.7201199078126,10.9922267255499));
#59325=CARTESIAN_POINT('Ctrl Pts',(12.7452929149993,20.7411542168826,10.9933140749918));
#59326=CARTESIAN_POINT('Ctrl Pts',(12.0155640244321,20.7221292061764,11.3082369208426));
#59327=CARTESIAN_POINT('Ctrl Pts',(12.311505593863,20.7496195010182,10.9937842864445));
#59328=CARTESIAN_POINT('Ctrl Pts',(12.7437800259182,20.7684410051488,10.994653844147));
#59329=CARTESIAN_POINT('Ctrl Pts',(12.0149107569711,20.7384917126866,11.3089309950962));
#59330=CARTESIAN_POINT('Ctrl Pts',(12.3108685826693,20.764361377477,10.9944974844729));
#59331=CARTESIAN_POINT('Ctrl Pts',(12.7430871664801,20.7820764272374,10.9952672936768));
#59332=CARTESIAN_POINT('Ctrl Pts',(12.0095689908778,20.8856685275638,11.3146056335284));
#59333=CARTESIAN_POINT('Ctrl Pts',(12.3056609603354,20.8969330014969,11.0003271040206));
#59334=CARTESIAN_POINT('Ctrl Pts',(12.7374216570268,20.9047237729811,11.0002827566569));
#59335=CARTESIAN_POINT('Ctrl Pts',(12.0086433373455,21.0158830521051,11.3155866742477));
#59336=CARTESIAN_POINT('Ctrl Pts',(12.3047572432467,21.0143356842118,11.0013363733449));
#59337=CARTESIAN_POINT('Ctrl Pts',(12.7364399032656,21.0132358767584,11.0011498385414));
#59338=CARTESIAN_POINT('Ctrl Pts',(12.0142277814707,21.2751278248493,11.3096572627521));
#59339=CARTESIAN_POINT('Ctrl Pts',(12.3102031016944,21.2479351155163,10.9952432127086));
#59340=CARTESIAN_POINT('Ctrl Pts',(12.7423627985092,21.2292731873702,10.9959091966857));
#59341=CARTESIAN_POINT('Ctrl Pts',(12.0207379593602,21.4041580408216,11.302746481911));
#59342=CARTESIAN_POINT('Ctrl Pts',(12.3165572121242,21.3642312602987,10.9881354276293));
#59343=CARTESIAN_POINT('Ctrl Pts',(12.7492675327281,21.3367983673583,10.9898011836399));
#59344=CARTESIAN_POINT('Ctrl Pts',(12.0409988281294,21.6610588333447,11.2811597960023));
#59345=CARTESIAN_POINT('Ctrl Pts',(12.3363065386174,21.595548212528,10.9659614584083));
#59346=CARTESIAN_POINT('Ctrl Pts',(12.7707563327911,21.5508823611137,10.9707220417886));
#59347=CARTESIAN_POINT('Ctrl Pts',(12.0547495047205,21.7889294026305,11.2664837866553));
#59348=CARTESIAN_POINT('Ctrl Pts',(12.349718084816,21.7106645499933,10.9508766506942));
#59349=CARTESIAN_POINT('Ctrl Pts',(12.7853403839175,21.6574411688554,10.9577508216129));
#59350=CARTESIAN_POINT('Ctrl Pts',(12.0806691551057,21.9798772439527,11.238665107521));
#59351=CARTESIAN_POINT('Ctrl Pts',(12.3749467442548,21.8822386065852,10.922339947102));
#59352=CARTESIAN_POINT('Ctrl Pts',(12.8128309220202,21.8165643699622,10.9331636050952));
#59353=CARTESIAN_POINT('Ctrl Pts',(12.0901914143202,22.043383452334,11.2284239908148));
#59354=CARTESIAN_POINT('Ctrl Pts',(12.3842191682733,21.9393067824406,10.9118296385023));
#59355=CARTESIAN_POINT('Ctrl Pts',(12.8229302879886,21.869486210272,10.9241121131162));
#59356=CARTESIAN_POINT('Ctrl Pts',(12.1057822814319,22.1384289822797,11.2116053173785));
#59357=CARTESIAN_POINT('Ctrl Pts',(12.399387260399,22.024630165775,10.8945839141828));
#59358=CARTESIAN_POINT('Ctrl Pts',(12.8394660560276,21.9486908185696,10.9092471239345));
#59359=CARTESIAN_POINT('Ctrl Pts',(12.1111971576597,22.1700751906362,11.2057562102194));
#59360=CARTESIAN_POINT('Ctrl Pts',(12.4046562361949,22.0530398313492,10.8885851232551));
#59361=CARTESIAN_POINT('Ctrl Pts',(12.8452091066483,21.9750626588589,10.9040774585348));
#59362=CARTESIAN_POINT('Ctrl Pts',(12.1196444127229,22.2174911125637,11.1966171908215));
#59363=CARTESIAN_POINT('Ctrl Pts',(12.4128724109568,22.0955840554947,10.8792160256234));
#59364=CARTESIAN_POINT('Ctrl Pts',(12.8541683165045,22.0145759271388,10.896000042389));
#59365=CARTESIAN_POINT('Ctrl Pts',(12.1225150265228,22.233290970441,11.1935091880825));
#59366=CARTESIAN_POINT('Ctrl Pts',(12.415664714645,22.1097605880446,10.8760295004639));
#59367=CARTESIAN_POINT('Ctrl Pts',(12.8572129069367,22.0277424753804,10.8932530703498));
#59368=CARTESIAN_POINT('Ctrl Pts',(12.1283510335089,22.2648029487245,11.1871855137895));
#59369=CARTESIAN_POINT('Ctrl Pts',(12.4213408466648,22.1380298284887,10.869546765911));
#59370=CARTESIAN_POINT('Ctrl Pts',(12.8634026112788,22.0540024572575,10.887663964133));
#59371=CARTESIAN_POINT('Ctrl Pts',(12.1313179098281,22.2805235674223,11.1839682389273));
#59372=CARTESIAN_POINT('Ctrl Pts',(12.4242261847655,22.1521303131032,10.8662488345689));
#59373=CARTESIAN_POINT('Ctrl Pts',(12.8665492983217,22.0671029728649,10.8848204132664));
#59374=CARTESIAN_POINT('Ctrl Pts',(12.158453868661,22.4216940521507,11.1545177680223));
#59375=CARTESIAN_POINT('Ctrl Pts',(12.4506457697523,22.2788848408611,10.836026130008));
#59376=CARTESIAN_POINT('Ctrl Pts',(12.8953298605484,22.1847450433553,10.8587909560006));
#59377=CARTESIAN_POINT('Ctrl Pts',(12.185657553851,22.5449416423991,11.1248253769103));
#59378=CARTESIAN_POINT('Ctrl Pts',(12.4770970806105,22.3892794656903,10.8055914845914));
#59379=CARTESIAN_POINT('Ctrl Pts',(12.9241822542658,22.2874513687631,10.8325476820865));
#59380=CARTESIAN_POINT('Ctrl Pts',(12.2456284410546,22.7872847696196,11.0587781318782));
#59381=CARTESIAN_POINT('Ctrl Pts',(12.5352981208323,22.6058827713513,10.7380176167549));
#59382=CARTESIAN_POINT('Ctrl Pts',(12.987787740331,22.4894039745858,10.7741725908326));
#59383=CARTESIAN_POINT('Ctrl Pts',(12.2783962022139,22.9063798510103,11.0224225011533));
#59384=CARTESIAN_POINT('Ctrl Pts',(12.5670873483069,22.7121519963084,10.7008302239268));
#59385=CARTESIAN_POINT('Ctrl Pts',(13.0225414267954,22.5886498759212,10.7420400897768));
#59386=CARTESIAN_POINT('Ctrl Pts',(12.348978997876,23.1406674713625,10.9432869286375));
#59387=CARTESIAN_POINT('Ctrl Pts',(12.6354186655169,22.9206728285625,10.6200488154105));
#59388=CARTESIAN_POINT('Ctrl Pts',(13.0974019672394,22.7838895593894,10.672097032513));
#59389=CARTESIAN_POINT('Ctrl Pts',(12.3867944287769,23.2558597170703,10.9005065193677));
#59390=CARTESIAN_POINT('Ctrl Pts',(12.6720038124617,23.0229760377839,10.5764003243843));
#59391=CARTESIAN_POINT('Ctrl Pts',(13.137509242867,22.8798830976101,10.634286065381));
#59392=CARTESIAN_POINT('Ctrl Pts',(12.4469685868315,23.4258627923054,10.831615883529));
#59393=CARTESIAN_POINT('Ctrl Pts',(12.7300143003336,23.173317069492,10.5063568717909));
#59394=CARTESIAN_POINT('Ctrl Pts',(13.2013303192544,23.0215523268955,10.5733978767148));
#59395=CARTESIAN_POINT('Ctrl Pts',(12.4676023227972,23.4820658196941,10.8078648704614));
#59396=CARTESIAN_POINT('Ctrl Pts',(12.7499178282157,23.2230124750191,10.4821924416464));
#59397=CARTESIAN_POINT('Ctrl Pts',(13.2232145849018,23.0683881830955,10.552405819973));
#59398=CARTESIAN_POINT('Ctrl Pts',(12.4993789165946,23.5656872650545,10.7710625930677));
#59399=CARTESIAN_POINT('Ctrl Pts',(12.7805178446485,23.2967857258851,10.4448117710785));
#59400=CARTESIAN_POINT('Ctrl Pts',(13.2569170326935,23.1380727208702,10.5198785544187));
#59401=CARTESIAN_POINT('Ctrl Pts',(12.5101166355672,23.5934665898445,10.7585899951691));
#59402=CARTESIAN_POINT('Ctrl Pts',(12.7908606252549,23.3212906461701,10.4321395053253));
#59403=CARTESIAN_POINT('Ctrl Pts',(13.2683055226197,23.1612221582558,10.508854793852));
#59404=CARTESIAN_POINT('Ctrl Pts',(12.53179209151,23.6486249072268,10.7333342394064));
#59405=CARTESIAN_POINT('Ctrl Pts',(12.8117286055676,23.3699078275031,10.4064914643755));
#59406=CARTESIAN_POINT('Ctrl Pts',(13.2912946424622,23.2071874226369,10.4865327872123));
#59407=CARTESIAN_POINT('Ctrl Pts',(12.5427358651168,23.6760204684585,10.7205441432531));
#59408=CARTESIAN_POINT('Ctrl Pts',(12.8222602521224,23.3940350953736,10.3935077573717));
#59409=CARTESIAN_POINT('Ctrl Pts',(13.3029016751728,23.2300170570987,10.4752284095746));
#59410=CARTESIAN_POINT('Ctrl Pts',(12.5979638689366,23.8121011103179,10.6557938094435));
#59411=CARTESIAN_POINT('Ctrl Pts',(12.8754924750573,23.5140302972315,10.3276719371624));
#59412=CARTESIAN_POINT('Ctrl Pts',(13.3614768304949,23.3434175917318,10.4179995785188));
#59413=CARTESIAN_POINT('Ctrl Pts',(12.643771837576,23.9180998292818,10.601437989252));
#59414=CARTESIAN_POINT('Ctrl Pts',(12.919492062782,23.6069903768932,10.2725850710442));
#59415=CARTESIAN_POINT('Ctrl Pts',(13.4100610400541,23.4317498578972,10.369957819201));
#59416=CARTESIAN_POINT('Ctrl Pts',(12.7381614324257,24.124811694524,10.487835670056));
#59417=CARTESIAN_POINT('Ctrl Pts',(13.0099210300387,23.7875812880369,10.157752716871));
#59418=CARTESIAN_POINT('Ctrl Pts',(13.5101712160083,23.6040097452743,10.2695517281672));
#59419=CARTESIAN_POINT('Ctrl Pts',(12.786743768146,24.2255239557177,10.4285885456025));
#59420=CARTESIAN_POINT('Ctrl Pts',(13.0563860864973,23.8752192933041,10.0979525157025));
#59421=CARTESIAN_POINT('Ctrl Pts',(13.5616979361181,23.6879366298853,10.2171868461805));
#59422=CARTESIAN_POINT('Ctrl Pts',(12.8862872577475,24.4219918048204,10.3053324039794));
#59423=CARTESIAN_POINT('Ctrl Pts',(13.151326026437,24.0454360470123,9.97389759363243));
#59424=CARTESIAN_POINT('Ctrl Pts',(13.667274364072,23.8516598372297,10.1082483365308));
#59425=CARTESIAN_POINT('Ctrl Pts',(12.937248915859,24.517746816217,10.2413230126633));
#59426=CARTESIAN_POINT('Ctrl Pts',(13.1998342286936,24.1280161508586,9.90958748677937));
#59427=CARTESIAN_POINT('Ctrl Pts',(13.7213246079408,23.9314556802555,10.0516743801166));
#59428=CARTESIAN_POINT('Ctrl Pts',(13.041219018545,24.7045359647819,10.1085959989972));
#59429=CARTESIAN_POINT('Ctrl Pts',(13.2985011177469,24.2883032081281,9.77665045676705));
#59430=CARTESIAN_POINT('Ctrl Pts',(13.8315959285483,24.0871133039103,9.93436515039151));
#59431=CARTESIAN_POINT('Ctrl Pts',(13.0942278294105,24.795569743092,10.0398781851834));
#59432=CARTESIAN_POINT('Ctrl Pts',(13.3486907582046,24.3660062569181,9.7079672620327));
#59433=CARTESIAN_POINT('Ctrl Pts',(13.8878173950481,24.1629747859347,9.87362970929413));
#59434=CARTESIAN_POINT('Ctrl Pts',(13.2020102216455,24.9730727963289,9.89772107757119));
#59435=CARTESIAN_POINT('Ctrl Pts',(13.4504091689276,24.5166541489231,9.56636618824304));
#59436=CARTESIAN_POINT('Ctrl Pts',(14.0021320530417,24.310893996916,9.74798580071625));
#59437=CARTESIAN_POINT('Ctrl Pts',(13.2567840727296,25.0595418800033,9.82428174061243));
#59438=CARTESIAN_POINT('Ctrl Pts',(13.5019665153703,24.5895901088978,9.49339094237622));
#59439=CARTESIAN_POINT('Ctrl Pts',(14.0602255319109,24.3829515666393,9.68307729610358));
#59440=CARTESIAN_POINT('Ctrl Pts',(13.3262035084363,25.1648285421005,9.72948365953242));
#59441=CARTESIAN_POINT('Ctrl Pts',(13.5668872401933,24.6775576076175,9.39982331745309));
#59442=CARTESIAN_POINT('Ctrl Pts',(14.1338522058603,24.4706904517579,9.59929111319616));
#59443=CARTESIAN_POINT('Ctrl Pts',(13.3401350908287,25.1857457215109,9.71037394265934));
#59444=CARTESIAN_POINT('Ctrl Pts',(13.5799441680015,24.6950553454771,9.3809208785823));
#59445=CARTESIAN_POINT('Ctrl Pts',(14.1486281266942,24.4881214345812,9.58240121196993));
#59446=CARTESIAN_POINT('Ctrl Pts',(13.3680902095933,25.2273004400984,9.67185248522811));
#59447=CARTESIAN_POINT('Ctrl Pts',(13.6061221656083,24.7297560468975,9.34285051244273));
#59448=CARTESIAN_POINT('Ctrl Pts',(14.1782774949656,24.5227503667599,9.54835446924372));
#59449=CARTESIAN_POINT('Ctrl Pts',(13.3821134917764,25.2479373475695,9.6524409830328));
#59450=CARTESIAN_POINT('Ctrl Pts',(13.6192433303242,24.7469581458693,9.32368199427145));
#59451=CARTESIAN_POINT('Ctrl Pts',(14.1931506731412,24.5399477896631,9.53119783858767));
#59452=CARTESIAN_POINT('Ctrl Pts',(13.4242368819105,25.3093150518009,9.59386146914878));
#59453=CARTESIAN_POINT('Ctrl Pts',(13.6586630795446,24.7980792953747,9.26582885724692));
#59454=CARTESIAN_POINT('Ctrl Pts',(14.2378269958757,24.591095876457,9.47942301556463));
#59455=CARTESIAN_POINT('Ctrl Pts',(13.4524167277085,25.3495622852733,9.55431246433107));
#59456=CARTESIAN_POINT('Ctrl Pts',(13.6849643583523,24.8314404027354,9.22687348103602));
#59457=CARTESIAN_POINT('Ctrl Pts',(14.2677147112974,24.6246352377576,9.44446808724288));
#59458=CARTESIAN_POINT('Ctrl Pts',(13.5372063494346,25.4683224074992,9.43417480126614));
#59459=CARTESIAN_POINT('Ctrl Pts',(13.7641233205245,24.9297095823926,9.10852127370187));
#59460=CARTESIAN_POINT('Ctrl Pts',(14.3576430977025,24.7236020061896,9.33828580903671));
#59461=CARTESIAN_POINT('Ctrl Pts',(13.5940653376125,25.5448561996849,9.35209697288459));
#59462=CARTESIAN_POINT('Ctrl Pts',(13.8169186749523,24.9923773886975,9.02809366159298));
#59463=CARTESIAN_POINT('Ctrl Pts',(14.417948085536,24.7873801664062,9.26574227412286));
#59464=CARTESIAN_POINT('Ctrl Pts',(13.6654272847918,25.6372918612587,9.24698560403133));
#59465=CARTESIAN_POINT('Ctrl Pts',(13.8827103346352,25.067184492195,8.92587537114921));
#59466=CARTESIAN_POINT('Ctrl Pts',(14.4936349989743,24.8644098843817,9.17284081161668));
#59467=CARTESIAN_POINT('Ctrl Pts',(13.6797141539562,25.6556172191055,9.22583750988905));
#59468=CARTESIAN_POINT('Ctrl Pts',(13.8959117260276,25.0820279842197,8.90526390781971));
#59469=CARTESIAN_POINT('Ctrl Pts',(14.5087877390924,24.8796810159181,9.1541493143201));
#59470=CARTESIAN_POINT('Ctrl Pts',(13.7083139270417,25.6919453148001,9.18328842901607));
#59471=CARTESIAN_POINT('Ctrl Pts',(13.9223129183792,25.1113853618828,8.86383826463687));
#59472=CARTESIAN_POINT('Ctrl Pts',(14.539120831663,24.9099544290033,9.11654280339907));
#59473=CARTESIAN_POINT('Ctrl Pts',(13.7226326555818,25.7099552850125,9.16187867514917));
#59474=CARTESIAN_POINT('Ctrl Pts',(13.9355182094804,25.1259044915328,8.8430149308617));
#59475=CARTESIAN_POINT('Ctrl Pts',(14.5543073620133,24.9249627375437,9.09762004121136));
#59476=CARTESIAN_POINT('Ctrl Pts',(13.7655806510432,25.7634487878384,9.09733261854258));
#59477=CARTESIAN_POINT('Ctrl Pts',(13.9751305079505,25.1689723680322,8.78023637313619));
#59478=CARTESIAN_POINT('Ctrl Pts',(14.5998582661927,24.9695406564653,9.04057175872457));
#59479=CARTESIAN_POINT('Ctrl Pts',(13.7941780979144,25.7983673942214,9.05391542849186));
#59480=CARTESIAN_POINT('Ctrl Pts',(14.0014262760392,25.1969111868538,8.73814081795549));
#59481=CARTESIAN_POINT('Ctrl Pts',(14.6301888917935,24.9986394952372,9.00219797980234));
#59482=CARTESIAN_POINT('Ctrl Pts',(13.8798356042923,25.9009302358346,8.92250522728221));
#59483=CARTESIAN_POINT('Ctrl Pts',(14.080204374513,25.2787388705709,8.6107394872982));
#59484=CARTESIAN_POINT('Ctrl Pts',(14.7210377619961,25.084108529757,8.88605259972134));
#59485=CARTESIAN_POINT('Ctrl Pts',(13.9367602535074,25.9663840884067,8.83335453123031));
#59486=CARTESIAN_POINT('Ctrl Pts',(14.1322279259698,25.330245918761,8.52486074193159));
#59487=CARTESIAN_POINT('Ctrl Pts',(14.7814123902207,25.1386534070522,8.80725779285579));
#59488=CARTESIAN_POINT('Ctrl Pts',(14.0500984561988,26.0915862509637,8.65194613998907));
#59489=CARTESIAN_POINT('Ctrl Pts',(14.2353745951717,25.4276650654009,8.35098471144773));
#59490=CARTESIAN_POINT('Ctrl Pts',(14.9016195746192,25.242988542423,8.64692209332295));
#59491=CARTESIAN_POINT('Ctrl Pts',(14.1065121739022,26.1513343014395,8.55968841168897));
#59492=CARTESIAN_POINT('Ctrl Pts',(14.2864905523139,25.473527188847,8.26296704102961));
#59493=CARTESIAN_POINT('Ctrl Pts',(14.9614523057975,25.2927785845191,8.56538117201096));
#59494=CARTESIAN_POINT('Ctrl Pts',(14.2186950223458,26.2651812652254,8.37201667934135));
#59495=CARTESIAN_POINT('Ctrl Pts',(14.3876971990642,25.5597553401026,8.0848856095321));
#59496=CARTESIAN_POINT('Ctrl Pts',(15.0804341144655,25.3876510543683,8.39950969127342));
#59497=CARTESIAN_POINT('Ctrl Pts',(14.2744642813816,26.3192800792414,8.27660270041679));
#59498=CARTESIAN_POINT('Ctrl Pts',(14.4377774098147,25.6000699835723,7.99480545474144));
#59499=CARTESIAN_POINT('Ctrl Pts',(15.1395833288898,25.4327333992899,8.31517915444208));
#59500=CARTESIAN_POINT('Ctrl Pts',(14.3852368576413,26.4218103331842,8.08253941101095));
#59501=CARTESIAN_POINT('Ctrl Pts',(14.536806721599,25.6752490298323,7.81265136249611));
#59502=CARTESIAN_POINT('Ctrl Pts',(15.2570693943164,25.5181752777314,8.14365857030466));
#59503=CARTESIAN_POINT('Ctrl Pts',(14.4402402789567,26.4702418187271,7.9838901831176));
#59504=CARTESIAN_POINT('Ctrl Pts',(14.5857421530009,25.71006068656,7.72056538801955));
#59505=CARTESIAN_POINT('Ctrl Pts',(15.3154063566312,25.5585348487929,8.05646859620055));
#59506=CARTESIAN_POINT('Ctrl Pts',(14.5493685169342,26.5613453046831,7.7832459506642));
#59507=CARTESIAN_POINT('Ctrl Pts',(14.682393434828,25.7742304787433,7.53443013914731));
#59508=CARTESIAN_POINT('Ctrl Pts',(15.4311484268895,25.6344544207156,7.87913152204095));
#59509=CARTESIAN_POINT('Ctrl Pts',(14.6034934217443,26.604017500099,7.68125109313529));
#59510=CARTESIAN_POINT('Ctrl Pts',(14.7300925300169,25.803534633669,7.4403736510247));
#59511=CARTESIAN_POINT('Ctrl Pts',(15.4885536292969,25.6700145831945,7.78898455200868));
#59512=CARTESIAN_POINT('Ctrl Pts',(14.6839417041762,26.6635790246801,7.52564054729126));
#59513=CARTESIAN_POINT('Ctrl Pts',(14.8005111418582,25.8432706371624,7.29814620728082));
#59514=CARTESIAN_POINT('Ctrl Pts',(15.5738775649483,25.7196491873441,7.65144997866894));
#59515=CARTESIAN_POINT('Ctrl Pts',(14.7106346565754,26.6826911151509,7.47333370333937));
#59516=CARTESIAN_POINT('Ctrl Pts',(14.8238726296942,25.8558472906946,7.25038337988665));
#59517=CARTESIAN_POINT('Ctrl Pts',(15.6021882722161,25.7355759291614,7.6052191822394));
#59518=CARTESIAN_POINT('Ctrl Pts',(14.7504796027575,26.7102247625861,7.39420202921272));
#59519=CARTESIAN_POINT('Ctrl Pts',(14.8586259533269,25.8736455053003,7.17845152574216));
#59520=CARTESIAN_POINT('Ctrl Pts',(15.6444480634853,25.758520635554,7.53527957127637));
#59521=CARTESIAN_POINT('Ctrl Pts',(14.7637288390933,26.7192135210666,7.36771288292358));
#59522=CARTESIAN_POINT('Ctrl Pts',(14.8701815395122,25.8794092498503,7.15438535620414));
#59523=CARTESIAN_POINT('Ctrl Pts',(15.6585002839332,25.7660112674848,7.51186744702555));
#59524=CARTESIAN_POINT('Ctrl Pts',(14.7901608727406,26.7368086126918,7.31450775636524));
#59525=CARTESIAN_POINT('Ctrl Pts',(14.8932084661783,25.8905852574532,7.10612929617896));
#59526=CARTESIAN_POINT('Ctrl Pts',(15.686534258921,25.7806738439805,7.46484271396204));
#59527=CARTESIAN_POINT('Ctrl Pts',(14.8033451749285,26.7454155612302,7.28778833164477));
#59528=CARTESIAN_POINT('Ctrl Pts',(14.9046806639825,25.8959968778302,7.0819365849418));
#59529=CARTESIAN_POINT('Ctrl Pts',(15.7005176097801,25.7878463010393,7.44122706080441));
#59530=CARTESIAN_POINT('Ctrl Pts',(14.9213099621474,26.8208949071534,7.04707639020546));
#59531=CARTESIAN_POINT('Ctrl Pts',(15.0080298043219,25.9433374988707,6.86262545158575));
#59532=CARTESIAN_POINT('Ctrl Pts',(15.8256317779751,25.8507457558477,7.22847660744676));
#59533=CARTESIAN_POINT('Ctrl Pts',(15.0219275551717,26.8744045260676,6.83003873153216));
#59534=CARTESIAN_POINT('Ctrl Pts',(15.0944925963321,25.9727974869176,6.66927856790164));
#59535=CARTESIAN_POINT('Ctrl Pts',(15.9323474070797,25.8953371048986,7.03665039403292));
#59536=CARTESIAN_POINT('Ctrl Pts',(15.166313899323,26.9342469486805,6.4997966771251));
#59537=CARTESIAN_POINT('Ctrl Pts',(15.217408331198,26.0000381535133,6.38029442707274));
#59538=CARTESIAN_POINT('Ctrl Pts',(16.0854844386362,25.9452057906459,6.74476979038736));
#59539=CARTESIAN_POINT('Ctrl Pts',(15.2133526217003,26.9507812969501,6.38893411293837));
#59540=CARTESIAN_POINT('Ctrl Pts',(15.2574505187818,26.0062612054673,6.28360198582695));
#59541=CARTESIAN_POINT('Ctrl Pts',(16.1353739927578,25.9589844139741,6.64678520082825));
#59542=CARTESIAN_POINT('Ctrl Pts',(15.3052181971078,26.9769019217655,6.16562024702973));
#59543=CARTESIAN_POINT('Ctrl Pts',(15.3354770678807,26.0130878248151,6.09018543098795));
#59544=CARTESIAN_POINT('Ctrl Pts',(16.2328071787053,25.9807516016223,6.44941183449709));
#59545=CARTESIAN_POINT('Ctrl Pts',(15.3500450744532,26.9864883979585,6.05316897490136));
#59546=CARTESIAN_POINT('Ctrl Pts',(15.3734229734647,26.0136448619288,5.99351603678512));
#59547=CARTESIAN_POINT('Ctrl Pts',(16.2803508365928,25.9887403314043,6.35002308388268));
#59548=CARTESIAN_POINT('Ctrl Pts',(15.4374530818873,26.9985121419444,5.8266440401815));
#59549=CARTESIAN_POINT('Ctrl Pts',(15.4473305488898,26.0091461456237,5.80010605796439));
#59550=CARTESIAN_POINT('Ctrl Pts',(16.3730562989198,25.9987601185148,6.14981165167035));
#59551=CARTESIAN_POINT('Ctrl Pts',(15.4800342357322,27.0009497744696,5.71257042320435));
#59552=CARTESIAN_POINT('Ctrl Pts',(15.4832543677699,26.0040503216918,5.70342562420715));
#59553=CARTESIAN_POINT('Ctrl Pts',(16.4182181288652,26.0007914784145,6.04898901042871));
#59554=CARTESIAN_POINT('Ctrl Pts',(15.5629140223877,26.9983869468892,5.48275732741083));
#59555=CARTESIAN_POINT('Ctrl Pts',(15.553198440089,25.9881837534892,5.50991450819736));
#59556=CARTESIAN_POINT('Ctrl Pts',(16.5061209327771,25.9986557893846,5.84587137521601));
#59557=CARTESIAN_POINT('Ctrl Pts',(15.6032126798844,26.993387062768,5.36701791538311));
#59558=CARTESIAN_POINT('Ctrl Pts',(15.5871816734266,25.9773800666379,5.41314943781346));
#59559=CARTESIAN_POINT('Ctrl Pts',(16.5488619332758,25.994489218574,5.7435764404109));
#59560=CARTESIAN_POINT('Ctrl Pts',(15.6521341808709,26.9822443529922,5.22126814446177));
#59561=CARTESIAN_POINT('Ctrl Pts',(15.6284283573509,25.9602766635703,5.29230273030841));
#59562=CARTESIAN_POINT('Ctrl Pts',(16.6007483736347,25.9852036275934,5.61475719837616));
#59563=CARTESIAN_POINT('Ctrl Pts',(15.6618458801285,26.9797708939527,5.19206438394472));
#59564=CARTESIAN_POINT('Ctrl Pts',(15.6366386050155,25.9566647485312,5.26807127988625));
#59565=CARTESIAN_POINT('Ctrl Pts',(16.6110486607591,25.9831424115216,5.58894579390439));
#59566=CARTESIAN_POINT('Ctrl Pts',(15.6811234037693,26.974326874309,5.13354825979902));
#59567=CARTESIAN_POINT('Ctrl Pts',(15.6529451403897,25.949071911402,5.2195917195971));
#59568=CARTESIAN_POINT('Ctrl Pts',(16.6314945191325,25.9786057286966,5.53722699728326));
#59569=CARTESIAN_POINT('Ctrl Pts',(15.6906700852009,26.9713614250745,5.10429370826743));
#59570=CARTESIAN_POINT('Ctrl Pts',(15.6610246184452,25.9450979582591,5.19539286772508));
#59571=CARTESIAN_POINT('Ctrl Pts',(16.6416197872961,25.976134520913,5.51137070173943));
#59572=CARTESIAN_POINT('Ctrl Pts',(15.7189906916946,26.9617499071457,5.01668212725527));
#59573=CARTESIAN_POINT('Ctrl Pts',(15.6850272934586,25.9326582303476,5.12297462527296));
#59574=CARTESIAN_POINT('Ctrl Pts',(16.6716567942978,25.9681249225861,5.43393622360837));
#59575=CARTESIAN_POINT('Ctrl Pts',(15.7374648005442,26.9543833549931,4.95841772357253));
#59576=CARTESIAN_POINT('Ctrl Pts',(15.700692464456,25.9236837080238,5.07499871525326));
#59577=CARTESIAN_POINT('Ctrl Pts',(16.6912505459564,25.9619861291773,5.38243990717622));
#59578=CARTESIAN_POINT('Ctrl Pts',(15.7916941691089,26.9294183822048,4.78405831366508));
#59579=CARTESIAN_POINT('Ctrl Pts',(15.7468332080221,25.8946946466028,4.93160995684196));
#59580=CARTESIAN_POINT('Ctrl Pts',(16.748766543145,25.941181985138,5.22833436818176));
#59581=CARTESIAN_POINT('Ctrl Pts',(15.826256817311,26.9089571134584,4.66839662254084));
#59582=CARTESIAN_POINT('Ctrl Pts',(15.7763008752334,25.8726888517142,4.83719393920763));
#59583=CARTESIAN_POINT('Ctrl Pts',(16.785423884099,25.9241309356715,5.12610816476558));
#59584=CARTESIAN_POINT('Ctrl Pts',(15.8592935131526,26.8846780167695,4.55332947014332));
#59585=CARTESIAN_POINT('Ctrl Pts',(15.8045942913409,25.8480831184251,4.74384742394865));
#59586=CARTESIAN_POINT('Ctrl Pts',(16.82046281698,25.9038983473079,5.02440735997516));
#59587=CARTESIAN_POINT('Ctrl Pts',(12.2613198608839,20.1060920634664,11.0892508104087));
#59588=CARTESIAN_POINT('Ctrl Pts',(12.2877096573058,20.1180918018476,11.0727355939116));
#59589=CARTESIAN_POINT('Ctrl Pts',(12.3147120693345,20.1300903154246,11.0577588203659));
#59590=CARTESIAN_POINT('Ctrl Pts',(12.3422975139329,20.1420817712088,11.0442572149087));
#59591=CARTESIAN_POINT('Ctrl Pts',(12.3559433417106,20.1480136437168,11.0375783092223));
#59592=CARTESIAN_POINT('Ctrl Pts',(12.3697324633206,20.1539441026838,11.0312608526765));
#59593=CARTESIAN_POINT('Ctrl Pts',(12.3836643352525,20.1598738261723,11.0253004693755));
#59594=CARTESIAN_POINT('Ctrl Pts',(12.4130618840363,20.1723860956205,11.0127235048641));
#59595=CARTESIAN_POINT('Ctrl Pts',(12.44309018573,20.1848921965551,11.0017350664173));
#59596=CARTESIAN_POINT('Ctrl Pts',(12.4737513223635,20.1973907787835,10.9923335427643));
#59597=CARTESIAN_POINT('Ctrl Pts',(12.4869951325672,20.2027894322264,10.9882726367263));
#59598=CARTESIAN_POINT('Ctrl Pts',(12.5003572194867,20.2081867124763,10.9845084380645));
#59599=CARTESIAN_POINT('Ctrl Pts',(12.5138382575052,20.2135823421314,10.9810437928846));
#59600=CARTESIAN_POINT('Ctrl Pts',(12.5250111044503,20.2180541449871,10.9781723559625));
#59601=CARTESIAN_POINT('Ctrl Pts',(12.5362658706435,20.2225248735315,10.9755066482006));
#59602=CARTESIAN_POINT('Ctrl Pts',(12.5476035673882,20.2269944600046,10.9730491517934));
#59603=CARTESIAN_POINT('Ctrl Pts',(12.5589412641329,20.2314640464776,10.9705916553862));
#59604=CARTESIAN_POINT('Ctrl Pts',(12.5703725446618,20.2359365220228,10.9683411866695));
#59605=CARTESIAN_POINT('Ctrl Pts',(12.5818127411584,20.2403787346282,10.9663142420145));
#59606=CARTESIAN_POINT('Ctrl Pts',(12.6046931341517,20.2492631598391,10.9622603527046));
#59607=CARTESIAN_POINT('Ctrl Pts',(12.6276769122765,20.2580536197943,10.9590831995557));
#59608=CARTESIAN_POINT('Ctrl Pts',(12.6507625114774,20.2667513813436,10.9567688098102));
#59609=CARTESIAN_POINT('Ctrl Pts',(12.6738481106782,20.275449142893,10.9544544200647));
#59610=CARTESIAN_POINT('Ctrl Pts',(12.6970355355578,20.2840542046749,10.9530028263328));
#59611=CARTESIAN_POINT('Ctrl Pts',(12.7203247848531,20.2925665415703,10.952413903835));
#59612=CARTESIAN_POINT('Ctrl Pts',(12.7319694095007,20.296822710018,10.9521194425861));
#59613=CARTESIAN_POINT('Ctrl Pts',(12.7436395141875,20.3010556774401,10.9520408617454));
#59614=CARTESIAN_POINT('Ctrl Pts',(12.7553352452135,20.3052653212751,10.9521794392714));
#59615=CARTESIAN_POINT('Ctrl Pts',(12.7611831107265,20.3073701431925,10.9522487280344));
#59616=CARTESIAN_POINT('Ctrl Pts',(12.7670373831595,20.3094691325677,10.9523723200043));
#59617=CARTESIAN_POINT('Ctrl Pts',(12.7728980912063,20.311562268036,10.9525504583199));
#59618=CARTESIAN_POINT('Ctrl Pts',(12.774363268218,20.3120855519031,10.9525949928988));
#59619=CARTESIAN_POINT('Ctrl Pts',(12.7758288474657,20.3126084698698,10.952642936901));
#59620=CARTESIAN_POINT('Ctrl Pts',(12.7772948299171,20.3131310202127,10.9526942944998));
#59621=CARTESIAN_POINT('Ctrl Pts',(12.7780278211428,20.3133922953841,10.9527199732992));
#59622=CARTESIAN_POINT('Ctrl Pts',(12.7787609131694,20.3136534786491,10.952746505501));
#59623=CARTESIAN_POINT('Ctrl Pts',(12.7794941056814,20.3139145709935,10.9527738918099));
#59624=CARTESIAN_POINT('Ctrl Pts',(12.7802272981934,20.3141756633379,10.9528012781189));
#59625=CARTESIAN_POINT('Ctrl Pts',(12.7809702417849,20.3144401343266,10.9528299067247));
#59626=CARTESIAN_POINT('Ctrl Pts',(12.7816933178538,20.3146973332162,10.9528585865539));
#59627=CARTESIAN_POINT('Ctrl Pts',(12.784585622129,20.3157261287749,10.9529733058707));
#59628=CARTESIAN_POINT('Ctrl Pts',(12.7874779796508,20.3167531168603,10.9531012855059));
#59629=CARTESIAN_POINT('Ctrl Pts',(12.790367822021,20.3177766834169,10.9532422736611));
#59630=CARTESIAN_POINT('Ctrl Pts',(15.8637983830994,26.6272203519198,4.6763017624696));
#59631=CARTESIAN_POINT('Ctrl Pts',(15.8349038320035,26.6601158718637,4.75787351480363));
#59632=CARTESIAN_POINT('Ctrl Pts',(15.8052672194834,26.6925210251888,4.83935638988722));
#59633=CARTESIAN_POINT('Ctrl Pts',(15.7751639364047,26.7244625096831,4.9208424051611));
#59634=CARTESIAN_POINT('Ctrl Pts',(15.7735322678848,26.7261938130293,4.92525913823247));
#59635=CARTESIAN_POINT('Ctrl Pts',(15.7718992639185,26.7279237294146,4.92967580195018));
#59636=CARTESIAN_POINT('Ctrl Pts',(15.7702649656506,26.7296522715952,4.93409242389849));
#59637=CARTESIAN_POINT('Ctrl Pts',(15.7502539098552,26.7508172906735,4.98817145584254));
#59638=CARTESIAN_POINT('Ctrl Pts',(15.7300480550329,26.7717766681125,5.04224424269192));
#59639=CARTESIAN_POINT('Ctrl Pts',(15.709725991688,26.7925423987736,5.09636326895675));
#59640=CARTESIAN_POINT('Ctrl Pts',(15.7010873400666,26.8013696477494,5.11936858126495));
#59641=CARTESIAN_POINT('Ctrl Pts',(15.6924243940276,26.8101626876449,5.14239245762853));
#59642=CARTESIAN_POINT('Ctrl Pts',(15.6837524821722,26.8189188830466,5.1654118929897));
#59643=CARTESIAN_POINT('Ctrl Pts',(15.68209242477,26.8205950747831,5.16981848575752));
#59644=CARTESIAN_POINT('Ctrl Pts',(15.6804314503341,26.8222700879288,5.17422670287004));
#59645=CARTESIAN_POINT('Ctrl Pts',(15.6787696557313,26.8239439009101,5.17863639594407));
#59646=CARTESIAN_POINT('Ctrl Pts',(15.6683658191531,26.8344229797867,5.20624373443547));
#59647=CARTESIAN_POINT('Ctrl Pts',(15.6579486373731,26.844849877472,5.23385227711352));
#59648=CARTESIAN_POINT('Ctrl Pts',(15.6475281571989,26.8552273352648,5.26147252908649));
#59649=CARTESIAN_POINT('Ctrl Pts',(15.6287933916902,26.8738847517249,5.3111304081236));
#59650=CARTESIAN_POINT('Ctrl Pts',(15.6100478265525,26.8923841385894,5.36082626140884));
#59651=CARTESIAN_POINT('Ctrl Pts',(15.5913526570138,26.9107267231326,5.4106217245225));
#59652=CARTESIAN_POINT('Ctrl Pts',(15.5759753763904,26.925813993098,5.45157983450311));
#59653=CARTESIAN_POINT('Ctrl Pts',(15.5606365219061,26.940795775563,5.49259231312282));
#59654=CARTESIAN_POINT('Ctrl Pts',(15.5453788495309,26.9556741079129,5.53367425118021));
#59655=CARTESIAN_POINT('Ctrl Pts',(15.5374315984396,26.9634237724814,5.55507256601038));
#59656=CARTESIAN_POINT('Ctrl Pts',(15.5295055620971,26.9711442394673,5.57649219744023));
#59657=CARTESIAN_POINT('Ctrl Pts',(15.5216083672387,26.9788375422302,5.59793131348772));
#59658=CARTESIAN_POINT('Ctrl Pts',(15.5143439910773,26.9859143645949,5.61765246844561));
#59659=CARTESIAN_POINT('Ctrl Pts',(15.5071040241837,26.9929681813793,5.63739011108275));
#59660=CARTESIAN_POINT('Ctrl Pts',(15.4998946833985,27.,5.65714286308472));
#59661=CARTESIAN_POINT('Origin',(-11.,51.,-13.6106575888162));
#59662=CARTESIAN_POINT('Origin',(-11.,51.,-13.6106575888162));
#59663=CARTESIAN_POINT('Origin',(-11.,51.,-13.6106575888162));
#59664=CARTESIAN_POINT('Origin',(-11.,52.,-13.6106575888162));
#59665=CARTESIAN_POINT('Ctrl Pts',(-10.3714285714286,38.7323075626015,-12.8329057265981));
#59666=CARTESIAN_POINT('Ctrl Pts',(-10.3703047272601,38.7337956967718,-12.8338140064349));
#59667=CARTESIAN_POINT('Ctrl Pts',(-10.3691828501228,38.7352838331315,-12.8347247235238));
#59668=CARTESIAN_POINT('Ctrl Pts',(-10.2297794583371,38.9205231532402,-12.9483917264144));
#59669=CARTESIAN_POINT('Ctrl Pts',(-10.1237094532379,39.1011906672438,-13.0964292382757));
#59670=CARTESIAN_POINT('Ctrl Pts',(-10.0208952490217,39.360673140197,-13.3756530051914));
#59671=CARTESIAN_POINT('Ctrl Pts',(-10.,39.4508344663996,-13.4925906505731));
#59672=CARTESIAN_POINT('Ctrl Pts',(-10.,39.5242048993244,-13.6106575888162));
#59673=CARTESIAN_POINT('Origin',(6.61363325216158E-15,38.7323075626015,
8.67361737988404E-16));
#59674=CARTESIAN_POINT('Origin',(-6.5,38.7323075626015,-16.2480768092719));
#59675=CARTESIAN_POINT('Origin',(-6.5,40.2323075626015,-31.8229001029736));
#59676=CARTESIAN_POINT('Ctrl Pts',(-6.,40.2323075626015,-16.7705098312484));
#59677=CARTESIAN_POINT('Ctrl Pts',(-6.,40.2152260685424,-16.7705098300399));
#59678=CARTESIAN_POINT('Ctrl Pts',(-6.00087270480098,40.1983584811302,-16.7697298783156));
#59679=CARTESIAN_POINT('Ctrl Pts',(-6.00256838001511,40.1816934989509,-16.7682104533614));
#59680=CARTESIAN_POINT('Ctrl Pts',(-6.00291333028549,40.178303350849,-16.7679013575838));
#59681=CARTESIAN_POINT('Ctrl Pts',(-6.00329235512771,40.1749215836645,-16.7675616445011));
#59682=CARTESIAN_POINT('Ctrl Pts',(-6.0037052686087,40.1715481408978,-16.7671913871201));
#59683=CARTESIAN_POINT('Ctrl Pts',(-6.005335465801,40.1582296681913,-16.765729597736));
#59684=CARTESIAN_POINT('Ctrl Pts',(-6.00749386985472,40.1450410361966,-16.7637923412657));
#59685=CARTESIAN_POINT('Ctrl Pts',(-6.01016893654584,40.1319804512336,-16.7613838478594));
#59686=CARTESIAN_POINT('Ctrl Pts',(-6.01150217107971,40.1254711470122,-16.7601834715868));
#59687=CARTESIAN_POINT('Ctrl Pts',(-6.01296373632936,40.1189936487289,-16.7588660602385));
#59688=CARTESIAN_POINT('Ctrl Pts',(-6.01455377974561,40.1125480291574,-16.7574302675289));
#59689=CARTESIAN_POINT('Ctrl Pts',(-6.0169439717228,40.1028588168814,-16.7552719489697));
#59690=CARTESIAN_POINT('Ctrl Pts',(-6.01963110947182,40.0932249571053,-16.7528410281537));
#59691=CARTESIAN_POINT('Ctrl Pts',(-6.02257533346268,40.0837623210638,-16.7501687385702));
#59692=CARTESIAN_POINT('Ctrl Pts',(-6.02389791871011,40.0795115769393,-16.7489683099374));
#59693=CARTESIAN_POINT('Ctrl Pts',(-6.02527425556365,40.0752883249674,-16.7477175528816));
#59694=CARTESIAN_POINT('Ctrl Pts',(-6.02670067639266,40.0711003969021,-16.7464194186541));
#59695=CARTESIAN_POINT('Ctrl Pts',(-6.02807072595986,40.0670779731429,-16.745172585882));
#59696=CARTESIAN_POINT('Ctrl Pts',(-6.02948329310936,40.063098660006,-16.7438852854621));
#59697=CARTESIAN_POINT('Ctrl Pts',(-6.03093707782595,40.0591602985701,-16.7425585794677));
#59698=CARTESIAN_POINT('Ctrl Pts',(-6.03387632863431,40.0511977495752,-16.7398762554468));
#59699=CARTESIAN_POINT('Ctrl Pts',(-6.03698370699615,40.0434031654531,-16.7370331048754));
#59700=CARTESIAN_POINT('Ctrl Pts',(-6.04024790247354,40.0357674679134,-16.7340364148325));
#59701=CARTESIAN_POINT('Ctrl Pts',(-6.0449141209408,40.024852118904,-16.7297525995659));
#59702=CARTESIAN_POINT('Ctrl Pts',(-6.0499000474802,40.0142610236446,-16.7251561505607));
#59703=CARTESIAN_POINT('Ctrl Pts',(-6.05518149077389,40.0039727938111,-16.7202613803198));
#59704=CARTESIAN_POINT('Ctrl Pts',(-6.05744858312296,39.9995565072311,-16.7181602697812));
#59705=CARTESIAN_POINT('Ctrl Pts',(-6.0597701483618,39.9951960798736,-16.7160040490599));
#59706=CARTESIAN_POINT('Ctrl Pts',(-6.06214427791603,39.9908901509711,-16.7137939059645));
#59707=CARTESIAN_POINT('Ctrl Pts',(-6.06864070612356,39.9791076608659,-16.7077462006395));
#59708=CARTESIAN_POINT('Ctrl Pts',(-6.07553063592893,39.9677331969345,-16.7012947219666));
#59709=CARTESIAN_POINT('Ctrl Pts',(-6.08278766669716,39.9567462769058,-16.6944505893577));
#59710=CARTESIAN_POINT('Ctrl Pts',(-6.08461402447538,39.9539812277425,-16.6927281445694));
#59711=CARTESIAN_POINT('Ctrl Pts',(-6.08646377242624,39.9512405363443,-16.6909806468571));
#59712=CARTESIAN_POINT('Ctrl Pts',(-6.08833629232153,39.9485242090016,-16.6892084804434));
#59713=CARTESIAN_POINT('Ctrl Pts',(-6.09070655159091,39.9450858476368,-16.686965249875));
#59714=CARTESIAN_POINT('Ctrl Pts',(-6.0931134023071,39.9416865866905,-16.6846823645151));
#59715=CARTESIAN_POINT('Ctrl Pts',(-6.09555574756902,39.9383265314523,-16.6823604186901));
#59716=CARTESIAN_POINT('Ctrl Pts',(-6.09801610063588,39.9349417019858,-16.6800213527845));
#59717=CARTESIAN_POINT('Ctrl Pts',(-6.10051625664023,39.9315916991154,-16.6776390419408));
#59718=CARTESIAN_POINT('Ctrl Pts',(-6.10304466826099,39.928290351569,-16.6752240173384));
#59719=CARTESIAN_POINT('Ctrl Pts',(-6.10678165416141,39.92341096835,-16.6716546171608));
#59720=CARTESIAN_POINT('Ctrl Pts',(-6.11056908515597,39.9186518404417,-16.668024432723));
#59721=CARTESIAN_POINT('Ctrl Pts',(-6.11440532151745,39.9140046239577,-16.6643343458043));
#59722=CARTESIAN_POINT('Ctrl Pts',(-6.12544919130915,39.9006260807951,-16.6537112153166));
#59723=CARTESIAN_POINT('Ctrl Pts',(-6.13689162615053,39.8881758726312,-16.6425950921152));
#59724=CARTESIAN_POINT('Ctrl Pts',(-6.14866874643051,39.8765458402052,-16.6310255748251));
#59725=CARTESIAN_POINT('Ctrl Pts',(-6.16044586671049,39.8649158077793,-16.619456057535));
#59726=CARTESIAN_POINT('Ctrl Pts',(-6.17255719994684,39.8541058231107,-16.6074330450772));
#59727=CARTESIAN_POINT('Ctrl Pts',(-6.18495795774414,39.8440440390462,-16.5949803772694));
#59728=CARTESIAN_POINT('Ctrl Pts',(-6.19115833664278,39.839013147014,-16.5887540433655));
#59729=CARTESIAN_POINT('Ctrl Pts',(-6.19743103892612,39.8341693874632,-16.5824202196346));
#59730=CARTESIAN_POINT('Ctrl Pts',(-6.2037717941715,39.8295062938081,-16.5759807931943));
#59731=CARTESIAN_POINT('Ctrl Pts',(-6.20694217179419,39.8271747469806,-16.5727610799741));
#59732=CARTESIAN_POINT('Ctrl Pts',(-6.21012955915248,39.824888363891,-16.5695149694884));
#59733=CARTESIAN_POINT('Ctrl Pts',(-6.21333344646887,39.8226463997159,-16.5662426651369));
#59734=CARTESIAN_POINT('Ctrl Pts',(-6.21653733378526,39.8204044355407,-16.5629703607854));
#59735=CARTESIAN_POINT('Ctrl Pts',(-6.21975872711503,39.8182063277282,-16.5596708190893));
#59736=CARTESIAN_POINT('Ctrl Pts',(-6.22298327133341,39.816060360099,-16.5563585361363));
#59737=CARTESIAN_POINT('Ctrl Pts',(-6.23588144820696,39.8074764895821,-16.5431094043243));
#59738=CARTESIAN_POINT('Ctrl Pts',(-6.24887960590686,39.7996874748855,-16.5296056075263));
#59739=CARTESIAN_POINT('Ctrl Pts',(-6.26195557855337,39.7926087889069,-16.515863299996));
#59740=CARTESIAN_POINT('Ctrl Pts',(-6.26491334532597,39.7910076000127,-16.5127548092022));
#59741=CARTESIAN_POINT('Ctrl Pts',(-6.2678751485978,39.7894428128996,-16.5096340420518));
#59742=CARTESIAN_POINT('Ctrl Pts',(-6.27084071420014,39.7879135687944,-16.506501210133));
#59743=CARTESIAN_POINT('Ctrl Pts',(-6.28528892650271,39.780463103535,-16.4912380776512));
#59744=CARTESIAN_POINT('Ctrl Pts',(-6.2998262820572,39.7738559475515,-16.4756886097743));
#59745=CARTESIAN_POINT('Ctrl Pts',(-6.31443187001688,39.768018354096,-16.4598673206089));
#59746=CARTESIAN_POINT('Ctrl Pts',(-6.32333492367592,39.7644599620671,-16.4502232181747));
#59747=CARTESIAN_POINT('Ctrl Pts',(-6.33226341030448,39.7611876883161,-16.440478106521));
#59748=CARTESIAN_POINT('Ctrl Pts',(-6.34121473427545,39.7581899257814,-16.4306331935693));
#59749=CARTESIAN_POINT('Ctrl Pts',(-6.34735648803554,39.7561330770538,-16.4238783234143));
#59750=CARTESIAN_POINT('Ctrl Pts',(-6.35350901798207,39.7542054768412,-16.4170764545765));
#59751=CARTESIAN_POINT('Ctrl Pts',(-6.3596706706762,39.7524037396,-16.4102288970642));
#59752=CARTESIAN_POINT('Ctrl Pts',(-6.3635201769234,39.7512781002448,-16.4059508702538));
#59753=CARTESIAN_POINT('Ctrl Pts',(-6.36737627692165,39.7502009295338,-16.4016516058271));
#59754=CARTESIAN_POINT('Ctrl Pts',(-6.37122409342676,39.7491753178836,-16.3973476877078));
#59755=CARTESIAN_POINT('Ctrl Pts',(-6.37457974424939,39.7482808899468,-16.3935942742178));
#59756=CARTESIAN_POINT('Ctrl Pts',(-6.3779317495519,39.7474248597862,-16.389834380521));
#59757=CARTESIAN_POINT('Ctrl Pts',(-6.38128159473997,39.7466060693528,-16.3860663752365));
#59758=CARTESIAN_POINT('Ctrl Pts',(-6.38955863476667,39.7445829426677,-16.3767561149677));
#59759=CARTESIAN_POINT('Ctrl Pts',(-6.39781703593733,39.7427883967616,-16.3674024363885));
#59760=CARTESIAN_POINT('Ctrl Pts',(-6.40605643102158,39.7412122502155,-16.3580063013025));
#59761=CARTESIAN_POINT('Ctrl Pts',(-6.41109566421616,39.7402482753225,-16.3522596032327));
#59762=CARTESIAN_POINT('Ctrl Pts',(-6.4161277746267,39.7393658825604,-16.3464970397648));
#59763=CARTESIAN_POINT('Ctrl Pts',(-6.42115275150614,39.7385633481733,-16.3407187505363));
#59764=CARTESIAN_POINT('Ctrl Pts',(-6.43174690801946,39.7368713652831,-16.3285363859334));
#59765=CARTESIAN_POINT('Ctrl Pts',(-6.4423094285119,39.7355342933199,-16.3162840767447));
#59766=CARTESIAN_POINT('Ctrl Pts',(-6.45283975421962,39.7345366200808,-16.3039636584199));
#59767=CARTESIAN_POINT('Ctrl Pts',(-6.4686319955505,39.7330404178742,-16.2854868301735));
#59768=CARTESIAN_POINT('Ctrl Pts',(-6.48435190789287,39.7323075626015,-16.266856742178));
#59769=CARTESIAN_POINT('Ctrl Pts',(-6.5,39.7323075626015,-16.2480768092719));
#59770=CARTESIAN_POINT('Origin',(-5.,52.,-16.7705098312484));
#59771=CARTESIAN_POINT('Origin',(-5.,40.2323075626015,-16.7705098312484));
#59772=CARTESIAN_POINT('Ctrl Pts',(-14.1696709084508,34.2228423347593,-8.45401835497186));
#59773=CARTESIAN_POINT('Ctrl Pts',(-14.4598881528388,34.2800112558736,-7.96758898230353));
#59774=CARTESIAN_POINT('Ctrl Pts',(-15.0284388422964,34.3091931864527,-7.97011831445158));
#59775=CARTESIAN_POINT('Ctrl Pts',(-14.1687509928547,34.2417094783908,-8.45556021361394));
#59776=CARTESIAN_POINT('Ctrl Pts',(-14.4590195349379,34.2974823791094,-7.96916514970434));
#59777=CARTESIAN_POINT('Ctrl Pts',(-15.027463174257,34.3259639809838,-7.97157191635228));
#59778=CARTESIAN_POINT('Ctrl Pts',(-14.1678668544491,34.2605265108349,-8.45704153677041));
#59779=CARTESIAN_POINT('Ctrl Pts',(-14.4581845937863,34.3149090256939,-7.97067959720386));
#59780=CARTESIAN_POINT('Ctrl Pts',(-15.0265254516828,34.3426902318517,-7.97296845218914));
#59781=CARTESIAN_POINT('Ctrl Pts',(-14.1661635328208,34.2981938523499,-8.45989441550156));
#59782=CARTESIAN_POINT('Ctrl Pts',(-14.4565759909218,34.3497943960948,-7.97359633424001));
#59783=CARTESIAN_POINT('Ctrl Pts',(-15.024718898452,34.3761723132014,-7.97565803480127));
#59784=CARTESIAN_POINT('Ctrl Pts',(-14.1653454356421,34.3170219168472,-8.46126415076535));
#59785=CARTESIAN_POINT('Ctrl Pts',(-14.4558033400937,34.3672326811367,-7.97499678944735));
#59786=CARTESIAN_POINT('Ctrl Pts',(-15.0238512196152,34.3929083705295,-7.97694936773952));
#59787=CARTESIAN_POINT('Ctrl Pts',(-14.1629917065432,34.373489337447,-8.46520379440197));
#59788=CARTESIAN_POINT('Ctrl Pts',(-14.4535804037852,34.41953098386,-7.97902465759217));
#59789=CARTESIAN_POINT('Ctrl Pts',(-15.0213548402835,34.4431016332889,-7.98066350984471));
#59790=CARTESIAN_POINT('Ctrl Pts',(-14.1615566384215,34.4111119211253,-8.4676041477937));
#59791=CARTESIAN_POINT('Ctrl Pts',(-14.4522248265318,34.454380888302,-7.98147914140516));
#59792=CARTESIAN_POINT('Ctrl Pts',(-15.0198327983173,34.4765439298872,-7.98292646932796));
#59793=CARTESIAN_POINT('Ctrl Pts',(-14.1576526183944,34.5239129308506,-8.47413110853782));
#59794=CARTESIAN_POINT('Ctrl Pts',(-14.4485372614658,34.5588642949711,-7.98815276719896));
#59795=CARTESIAN_POINT('Ctrl Pts',(-15.0156921710414,34.5768114940933,-7.98907983290995));
#59796=CARTESIAN_POINT('Ctrl Pts',(-14.1555848703909,34.5990246231075,-8.47758373051289));
#59797=CARTESIAN_POINT('Ctrl Pts',(-14.446583355318,34.6284571865908,-7.99168420593832));
#59798=CARTESIAN_POINT('Ctrl Pts',(-15.0134991049499,34.6435774427604,-7.99233483016131));
#59799=CARTESIAN_POINT('Ctrl Pts',(-14.1509771790097,34.8240952679178,-8.4852743386372));
#59800=CARTESIAN_POINT('Ctrl Pts',(-14.4422301623517,34.8369697425827,-7.99954874151129));
#59801=CARTESIAN_POINT('Ctrl Pts',(-15.008612159576,34.8436402381527,-7.99958523498254));
#59802=CARTESIAN_POINT('Ctrl Pts',(-14.1500330992177,34.9737899010413,-8.48684678418226));
#59803=CARTESIAN_POINT('Ctrl Pts',(-14.4413373565372,34.9757252603891,-8.00115815623579));
#59804=CARTESIAN_POINT('Ctrl Pts',(-15.0076108628144,34.9767021342601,-8.00106767539272));
#59805=CARTESIAN_POINT('Ctrl Pts',(-14.1534989333457,35.4218322689878,-8.48106645017854));
#59806=CARTESIAN_POINT('Ctrl Pts',(-14.4446127086534,35.3909181528281,-7.99524560707017));
#59807=CARTESIAN_POINT('Ctrl Pts',(-15.0112867474724,35.3749620168757,-7.99561820204977));
#59808=CARTESIAN_POINT('Ctrl Pts',(-14.1642118082204,35.7191401530233,-8.46324178895702));
#59809=CARTESIAN_POINT('Ctrl Pts',(-14.454761563286,35.6666794668494,-7.97697017454646));
#59810=CARTESIAN_POINT('Ctrl Pts',(-15.0226488876287,35.6392356915726,-7.97881380780291));
#59811=CARTESIAN_POINT('Ctrl Pts',(-14.2018700963651,36.3110245203784,-8.3998954453284));
#59812=CARTESIAN_POINT('Ctrl Pts',(-14.4903036805241,36.2145680745722,-7.91223236340415));
#59813=CARTESIAN_POINT('Ctrl Pts',(-15.0625894960227,36.1653551292289,-7.91909334909917));
#59814=CARTESIAN_POINT('Ctrl Pts',(-14.2288151924285,36.6056011119585,-8.35437505244428));
#59815=CARTESIAN_POINT('Ctrl Pts',(-14.5157733460828,36.4872920363756,-7.86562765440656));
#59816=CARTESIAN_POINT('Ctrl Pts',(-15.0911676285592,36.4272009883655,-7.87617850054425));
#59817=CARTESIAN_POINT('Ctrl Pts',(-14.2678515285549,36.9354562627635,-8.28724846986359));
#59818=CARTESIAN_POINT('Ctrl Pts',(-14.5524221273012,36.7911880341194,-7.7973135407053));
#59819=CARTESIAN_POINT('Ctrl Pts',(-15.1325698029845,36.7204055669061,-7.81289418035236));
#59820=CARTESIAN_POINT('Ctrl Pts',(-14.272310834891,36.9720923458365,-8.27956682548256));
#59821=CARTESIAN_POINT('Ctrl Pts',(-14.5566164314028,36.8250040101967,-7.78948085637131));
#59822=CARTESIAN_POINT('Ctrl Pts',(-15.1372993703662,36.7529709740877,-7.80565222610578));
#59823=CARTESIAN_POINT('Ctrl Pts',(-14.2814663750741,37.0452925529125,-8.26376437000761));
#59824=CARTESIAN_POINT('Ctrl Pts',(-14.5652251137911,36.8925526698609,-7.77337133120969));
#59825=CARTESIAN_POINT('Ctrl Pts',(-15.1470097917179,36.8180378248002,-7.79075428816105));
#59826=CARTESIAN_POINT('Ctrl Pts',(-14.2861536017617,37.081785083136,-8.25565910563603));
#59827=CARTESIAN_POINT('Ctrl Pts',(-14.5696312954759,36.9262202981498,-7.76510980926654));
#59828=CARTESIAN_POINT('Ctrl Pts',(-15.1519810928061,36.850475629465,-7.78311296160134));
#59829=CARTESIAN_POINT('Ctrl Pts',(-14.3005366026303,37.1909436147287,-8.23073635121615));
#59830=CARTESIAN_POINT('Ctrl Pts',(-14.5831518360579,37.0269359064794,-7.7397041366779));
#59831=CARTESIAN_POINT('Ctrl Pts',(-15.1672357906114,36.9475054352928,-7.7596167619714));
#59832=CARTESIAN_POINT('Ctrl Pts',(-14.3105536680637,37.263290615546,-8.21331202705747));
#59833=CARTESIAN_POINT('Ctrl Pts',(-14.5925608990619,37.0936355928615,-7.7219524972774));
#59834=CARTESIAN_POINT('Ctrl Pts',(-15.1778599510383,37.0118138805059,-7.74318978992613));
#59835=CARTESIAN_POINT('Ctrl Pts',(-14.3418348010998,37.4790826477386,-8.15864801908498));
#59836=CARTESIAN_POINT('Ctrl Pts',(-14.6219410641221,37.2926085843646,-7.66625367882849));
#59837=CARTESIAN_POINT('Ctrl Pts',(-15.211036910134,37.2036290201708,-7.69165469791198));
#59838=CARTESIAN_POINT('Ctrl Pts',(-14.3643283878283,37.6212795682079,-8.11901917638115));
#59839=CARTESIAN_POINT('Ctrl Pts',(-14.6430362895773,37.4235089284438,-7.62591654935295));
#59840=CARTESIAN_POINT('Ctrl Pts',(-15.2348937448071,37.3300262828855,-7.65429417319524));
#59841=CARTESIAN_POINT('Ctrl Pts',(-14.4363019502445,38.0430610597211,-7.9907944336361));
#59842=CARTESIAN_POINT('Ctrl Pts',(-14.7105067497658,37.8118623201918,-7.49538846499181));
#59843=CARTESIAN_POINT('Ctrl Pts',(-15.3112293408869,37.7049431641283,-7.53340889331172));
#59844=CARTESIAN_POINT('Ctrl Pts',(-14.49026980554,38.3178484315225,-7.8928871878268));
#59845=CARTESIAN_POINT('Ctrl Pts',(-14.7609541970719,38.0639420611781,-7.39588717756517));
#59846=CARTESIAN_POINT('Ctrl Pts',(-15.3684679759171,37.9491986058153,-7.44110576650622));
#59847=CARTESIAN_POINT('Ctrl Pts',(-14.6080482783172,38.8552917835711,-7.67271221247472));
#59848=CARTESIAN_POINT('Ctrl Pts',(-14.8703740139742,38.5549584396854,-7.17322618837634));
#59849=CARTESIAN_POINT('Ctrl Pts',(-15.4933845372648,38.4269260298234,-7.2335333987612));
#59850=CARTESIAN_POINT('Ctrl Pts',(-14.6718611162741,39.1179471327802,-7.55044413842592));
#59851=CARTESIAN_POINT('Ctrl Pts',(-14.9295100780991,38.794189655202,-7.04967693049274));
#59852=CARTESIAN_POINT('Ctrl Pts',(-15.5610648206959,38.6603974512983,-7.11826383427611));
#59853=CARTESIAN_POINT('Ctrl Pts',(-14.7480666188548,39.4067715675604,-7.3989787087425));
#59854=CARTESIAN_POINT('Ctrl Pts',(-14.999316825149,39.0547855952716,-6.89817098281311));
#59855=CARTESIAN_POINT('Ctrl Pts',(-15.6418888381287,38.9171302822837,-6.97546814291349));
#59856=CARTESIAN_POINT('Ctrl Pts',(-14.7565941785648,39.4387656880567,-7.38195749962283));
#59857=CARTESIAN_POINT('Ctrl Pts',(-15.0071581686653,39.0837656036217,-6.88107637534832));
#59858=CARTESIAN_POINT('Ctrl Pts',(-15.6509332197322,38.9455695005142,-6.95942121181813));
#59859=CARTESIAN_POINT('Ctrl Pts',(-14.7737256022962,39.502412269052,-7.34761186407861));
#59860=CARTESIAN_POINT('Ctrl Pts',(-15.0228997481459,39.1413825527381,-6.84659981861948));
#59861=CARTESIAN_POINT('Ctrl Pts',(-15.6691029114839,39.002144239138,-6.92704148796774));
#59862=CARTESIAN_POINT('Ctrl Pts',(-14.7823346424693,39.5340844533758,-7.33027717344031));
#59863=CARTESIAN_POINT('Ctrl Pts',(-15.0308049908594,39.1700375342947,-6.82920681792526));
#59864=CARTESIAN_POINT('Ctrl Pts',(-15.6782337117527,39.0302972919077,-6.91069901878126));
#59865=CARTESIAN_POINT('Ctrl Pts',(-14.808284656594,39.6286524867301,-7.27779013265149));
#59866=CARTESIAN_POINT('Ctrl Pts',(-15.0546319241823,39.2556023565078,-6.77653515305077));
#59867=CARTESIAN_POINT('Ctrl Pts',(-15.7057564538778,39.1143577659461,-6.8612162865755));
#59868=CARTESIAN_POINT('Ctrl Pts',(-14.8257484822497,39.6910999140348,-7.24215491242092));
#59869=CARTESIAN_POINT('Ctrl Pts',(-15.0706345822693,39.31199951062,-6.74082930478049));
#59870=CARTESIAN_POINT('Ctrl Pts',(-15.7242786933826,39.1698665902847,-6.8276207929431));
#59871=CARTESIAN_POINT('Ctrl Pts',(-14.8785762907581,39.876683136037,-7.1333351875412));
#59872=CARTESIAN_POINT('Ctrl Pts',(-15.1190327204018,39.4796219387076,-6.63176677641015));
#59873=CARTESIAN_POINT('Ctrl Pts',(-15.7803081869927,39.3348294541919,-6.72502980625943));
#59874=CARTESIAN_POINT('Ctrl Pts',(-14.9143760584171,39.9980613049761,-7.05823809590922));
#59875=CARTESIAN_POINT('Ctrl Pts',(-15.1516954791241,39.5888243403568,-6.5567294842393));
#59876=CARTESIAN_POINT('Ctrl Pts',(-15.8182776378986,39.4427211600206,-6.65423120166715));
#59877=CARTESIAN_POINT('Ctrl Pts',(-15.0231004266237,40.3553871225062,-6.82537958602282));
#59878=CARTESIAN_POINT('Ctrl Pts',(-15.2508296348633,39.9103610239103,-6.3239951350709));
#59879=CARTESIAN_POINT('Ctrl Pts',(-15.9335913612037,39.7603441088107,-6.43470129294701));
#59880=CARTESIAN_POINT('Ctrl Pts',(-15.0973449297501,40.5845463158894,-6.66007288714214));
#59881=CARTESIAN_POINT('Ctrl Pts',(-15.31792988494,40.114768031037,-6.15976330372408));
#59882=CARTESIAN_POINT('Ctrl Pts',(-16.0123355319573,39.9640411696614,-6.2788565940716));
#59883=CARTESIAN_POINT('Ctrl Pts',(-15.2472968949109,41.0254173108877,-6.30922595793956));
#59884=CARTESIAN_POINT('Ctrl Pts',(-15.4523126364001,40.5055857309467,-5.81354666702777));
#59885=CARTESIAN_POINT('Ctrl Pts',(-16.1713754941982,40.3559264985848,-5.94809181206602));
#59886=CARTESIAN_POINT('Ctrl Pts',(-15.3230087426575,41.2371284648137,-6.12368686448347));
#59887=CARTESIAN_POINT('Ctrl Pts',(-15.5196455447178,40.6918988399555,-5.63122192702778));
#59888=CARTESIAN_POINT('Ctrl Pts',(-16.2516759396333,40.5441141908017,-5.77317280154761));
#59889=CARTESIAN_POINT('Ctrl Pts',(-15.4173521697931,41.4908768942127,-5.87860618526534));
#59890=CARTESIAN_POINT('Ctrl Pts',(-15.6023498902727,40.9125245108878,-5.39340306565551));
#59891=CARTESIAN_POINT('Ctrl Pts',(-16.3517371496677,40.7696683504473,-5.54212030933746));
#59892=CARTESIAN_POINT('Ctrl Pts',(-15.4362061333438,41.541080480963,-5.82893036895881));
#59893=CARTESIAN_POINT('Ctrl Pts',(-15.6189216498825,40.9563040712589,-5.34503370394812));
#59894=CARTESIAN_POINT('Ctrl Pts',(-16.3717337779055,40.814293760811,-5.49528788992432));
#59895=CARTESIAN_POINT('Ctrl Pts',(-15.4644422759024,41.6155621820111,-5.75341180123559));
#59896=CARTESIAN_POINT('Ctrl Pts',(-15.6436600403385,41.0210733659742,-5.27169025022555));
#59897=CARTESIAN_POINT('Ctrl Pts',(-16.4016812016563,40.8804997173657,-5.42409193382638));
#59898=CARTESIAN_POINT('Ctrl Pts',(-15.4738394697509,41.6402325166288,-5.72809098740203));
#59899=CARTESIAN_POINT('Ctrl Pts',(-15.6518901269291,41.042522534143,-5.24709833812979));
#59900=CARTESIAN_POINT('Ctrl Pts',(-16.4116479225022,40.9024289036886,-5.40022045953334));
#59901=CARTESIAN_POINT('Ctrl Pts',(-15.4925703942472,41.689181898316,-5.67723496738244));
#59902=CARTESIAN_POINT('Ctrl Pts',(-15.6682749940766,41.0850380021743,-5.1977485436834));
#59903=CARTESIAN_POINT('Ctrl Pts',(-16.4315140544655,40.9459394651512,-5.35227539009512));
#59904=CARTESIAN_POINT('Ctrl Pts',(-15.5019086640392,41.7134729307954,-5.65168764188966));
#59905=CARTESIAN_POINT('Ctrl Pts',(-15.6764336314637,41.1061140969787,-5.17297859437461));
#59906=CARTESIAN_POINT('Ctrl Pts',(-16.4414182800811,40.967531494057,-5.32819036948575));
#59907=CARTESIAN_POINT('Ctrl Pts',(-15.5484555651202,41.8340156143712,-5.52335553940722));
#59908=CARTESIAN_POINT('Ctrl Pts',(-15.7171539857794,41.2108612547213,-5.04834447526745));
#59909=CARTESIAN_POINT('Ctrl Pts',(-16.4907862052723,41.074680546041,-5.20720387542547));
#59910=CARTESIAN_POINT('Ctrl Pts',(-15.5852305114518,41.9275319640208,-5.41878553611691));
#59911=CARTESIAN_POINT('Ctrl Pts',(-15.7490791740827,41.2915492195499,-4.94737813664718));
#59912=CARTESIAN_POINT('Ctrl Pts',(-16.5297899365528,41.1578061902771,-5.10861936072794));
#59913=CARTESIAN_POINT('Ctrl Pts',(-15.6938508583456,42.199498468939,-5.0993756835597));
#59914=CARTESIAN_POINT('Ctrl Pts',(-15.8432282443095,41.526068650345,-4.63908945210971));
#59915=CARTESIAN_POINT('Ctrl Pts',(-16.64499333428,41.3995541945398,-4.80749222676696));
#59916=CARTESIAN_POINT('Ctrl Pts',(-15.7639910093299,42.369390564411,-4.87885064391805));
#59917=CARTESIAN_POINT('Ctrl Pts',(-15.9031097774975,41.6705184443034,-4.42842552480797));
#59918=CARTESIAN_POINT('Ctrl Pts',(-16.7193844041967,41.5505693905269,-4.59958983270443));
#59919=CARTESIAN_POINT('Ctrl Pts',(-15.8980969848804,42.6866289429011,-4.42234195955402));
#59920=CARTESIAN_POINT('Ctrl Pts',(-16.0164770439618,41.938203868012,-3.99591210397994));
#59921=CARTESIAN_POINT('Ctrl Pts',(-16.8616180139052,41.8325590604172,-4.16921127494601));
#59922=CARTESIAN_POINT('Ctrl Pts',(-15.9620670091645,42.8339757168234,-4.18635981457349));
#59923=CARTESIAN_POINT('Ctrl Pts',(-16.069837618137,42.061051465547,-3.77409145591909));
#59924=CARTESIAN_POINT('Ctrl Pts',(-16.9294650101271,41.9635339702937,-3.94673652549938));
#59925=CARTESIAN_POINT('Ctrl Pts',(-16.0521582726785,43.037709823846,-3.82021108244197));
#59926=CARTESIAN_POINT('Ctrl Pts',(-16.1440256404094,42.2291011383052,-3.43385778245536));
#59927=CARTESIAN_POINT('Ctrl Pts',(-17.0250163496069,42.1446309546378,-3.60154580164102));
#59928=CARTESIAN_POINT('Ctrl Pts',(-16.0812108244472,43.102733976819,-3.69612831892062));
#59929=CARTESIAN_POINT('Ctrl Pts',(-16.1678670548505,42.2825951618778,-3.31868636626619));
#59930=CARTESIAN_POINT('Ctrl Pts',(-17.0558296625103,42.2024302014641,-3.48456541848317));
#59931=CARTESIAN_POINT('Ctrl Pts',(-16.1231583043917,43.1958323041313,-3.50684228674254));
#59932=CARTESIAN_POINT('Ctrl Pts',(-16.2020593980967,42.358743766398,-3.14397959827399));
#59933=CARTESIAN_POINT('Ctrl Pts',(-17.1003194136399,42.2851842704153,-3.30611394037726));
#59934=CARTESIAN_POINT('Ctrl Pts',(-16.1368688153599,43.2261249913638,-3.44321966940264));
#59935=CARTESIAN_POINT('Ctrl Pts',(-16.2132166154573,42.3834909358494,-3.0852944650872));
#59936=CARTESIAN_POINT('Ctrl Pts',(-17.1148608648885,42.3121111033463,-3.24613302164169));
#59937=CARTESIAN_POINT('Ctrl Pts',(-16.1570050576291,43.2704363362883,-3.3469780073553));
#59938=CARTESIAN_POINT('Ctrl Pts',(-16.2295461487012,42.4195814461551,-2.99676810231204));
#59939=CARTESIAN_POINT('Ctrl Pts',(-17.1362174853078,42.3514989656337,-3.15540014162311));
#59940=CARTESIAN_POINT('Ctrl Pts',(-16.1636460804533,43.2850199841448,-3.31476016326283));
#59941=CARTESIAN_POINT('Ctrl Pts',(-16.234927397343,42.4314525764685,-2.96714277235139));
#59942=CARTESIAN_POINT('Ctrl Pts',(-17.1432609944394,42.3644622081519,-3.12502641655731));
#59943=CARTESIAN_POINT('Ctrl Pts',(-16.176779066406,43.3138032530051,-3.25006285951472));
#59944=CARTESIAN_POINT('Ctrl Pts',(-16.2455540938229,42.4548543838694,-2.90771276300664));
#59945=CARTESIAN_POINT('Ctrl Pts',(-17.1571899188963,42.3900473359813,-3.0640323254552));
#59946=CARTESIAN_POINT('Ctrl Pts',(-16.1832563592051,43.3279707317643,-3.21765573302902));
#59947=CARTESIAN_POINT('Ctrl Pts',(-16.2507873073283,42.4663580683418,-2.87797525515983));
#59948=CARTESIAN_POINT('Ctrl Pts',(-17.164059774934,42.4026406504781,-3.03348015236247));
#59949=CARTESIAN_POINT('Ctrl Pts',(-16.2407423662139,43.4534701977211,-2.92546660438112));
#59950=CARTESIAN_POINT('Ctrl Pts',(-16.2973926330638,42.5686355463496,-2.60882804918763));
#59951=CARTESIAN_POINT('Ctrl Pts',(-17.2250297821921,42.5141957311396,-2.75801565386698));
#59952=CARTESIAN_POINT('Ctrl Pts',(-16.2860851710674,43.5507845829967,-2.66201787685001));
#59953=CARTESIAN_POINT('Ctrl Pts',(-16.3334056853608,42.6464652770683,-2.36955567429105));
#59954=CARTESIAN_POINT('Ctrl Pts',(-17.27312063616,42.6006974071258,-2.50964648325415));
#59955=CARTESIAN_POINT('Ctrl Pts',(-16.3644674413509,43.7174968151427,-2.12770174998652));
#59956=CARTESIAN_POINT('Ctrl Pts',(-16.395286619085,42.7792030237934,-1.88723589636282));
#59957=CARTESIAN_POINT('Ctrl Pts',(-17.3562533467079,42.7488860578871,-2.00591410770285));
#59958=CARTESIAN_POINT('Ctrl Pts',(-16.3975090775376,43.7868935216046,-1.85683435243505));
#59959=CARTESIAN_POINT('Ctrl Pts',(-16.4209906605381,42.8337387768024,-1.64478289056291));
#59960=CARTESIAN_POINT('Ctrl Pts',(-17.3912975066884,42.810572019061,-1.75055090464328));
#59961=CARTESIAN_POINT('Ctrl Pts',(-16.4371973244655,43.8698191922474,-1.44484551307843));
#59962=CARTESIAN_POINT('Ctrl Pts',(-16.4517290374466,42.8986843931254,-1.27807359738039));
#59963=CARTESIAN_POINT('Ctrl Pts',(-17.4333911016012,42.8842837265137,-1.36214391805839));
#59964=CARTESIAN_POINT('Ctrl Pts',(-16.4487802554229,43.8939261909356,-1.30656641831514));
#59965=CARTESIAN_POINT('Ctrl Pts',(-16.4606689802262,42.9175109064172,-1.15517368833686));
#59966=CARTESIAN_POINT('Ctrl Pts',(-17.4456760285918,42.9057121696064,-1.23177978830181));
#59967=CARTESIAN_POINT('Ctrl Pts',(-16.4685324538335,43.9349488754536,-1.02806931366241));
#59968=CARTESIAN_POINT('Ctrl Pts',(-16.4758894976883,42.9495081386978,-0.908068000066032));
#59969=CARTESIAN_POINT('Ctrl Pts',(-17.4666253297105,42.9421767782951,-0.969223595380726));
#59970=CARTESIAN_POINT('Ctrl Pts',(-16.4767018066094,43.9518647448791,-0.887851353093695));
#59971=CARTESIAN_POINT('Ctrl Pts',(-16.4821582142198,42.9626536650404,-0.783956213361243));
#59972=CARTESIAN_POINT('Ctrl Pts',(-17.4752897950108,42.9572131064008,-0.837031578665104));
#59973=CARTESIAN_POINT('Ctrl Pts',(-16.4862967209135,43.9717089312722,-0.676029616417883));
#59974=CARTESIAN_POINT('Ctrl Pts',(-16.4895137451409,42.9780633749711,-0.596718279805704));
#59975=CARTESIAN_POINT('Ctrl Pts',(-17.4854662190897,42.9748523834323,-0.637334318512984));
#59976=CARTESIAN_POINT('Ctrl Pts',(-16.4890517437789,43.977401569991,-0.605173122314613));
#59977=CARTESIAN_POINT('Ctrl Pts',(-16.4916238230334,42.9824805634447,-0.534110465633991));
#59978=CARTESIAN_POINT('Ctrl Pts',(-17.4883882131625,42.9799125065679,-0.57053358332299));
#59979=CARTESIAN_POINT('Ctrl Pts',(-16.492506023628,43.9845357058383,-0.498508314718125));
#59980=CARTESIAN_POINT('Ctrl Pts',(-16.4942681869357,42.9880140786458,-0.439912398698345));
#59981=CARTESIAN_POINT('Ctrl Pts',(-17.49205184321,42.9862539607906,-0.469974168759785));
#59982=CARTESIAN_POINT('Ctrl Pts',(-16.4935448911152,43.9866805929804,-0.462870708599939));
#59983=CARTESIAN_POINT('Ctrl Pts',(-16.4950632373273,42.9896773373646,-0.408444310922235));
#59984=CARTESIAN_POINT('Ctrl Pts',(-17.4931536723775,42.9881605271315,-0.436376425617608));
#59985=CARTESIAN_POINT('Ctrl Pts',(-16.495392016117,43.9904934577505,-0.391554086603203));
#59986=CARTESIAN_POINT('Ctrl Pts',(-16.4964765826267,42.9926335814917,-0.345482344139571));
#59987=CARTESIAN_POINT('Ctrl Pts',(-17.4951127443838,42.9915497401849,-0.36914189982643));
#59988=CARTESIAN_POINT('Ctrl Pts',(-16.4961991039929,43.9921590221803,-0.355925418204801));
#59989=CARTESIAN_POINT('Ctrl Pts',(-16.4970939068081,42.9939245371181,-0.314034598998794));
#59990=CARTESIAN_POINT('Ctrl Pts',(-17.4959687466422,42.9930302419732,-0.335552582820379));
#59991=CARTESIAN_POINT('Ctrl Pts',(-16.4996553193878,43.9992904788907,-0.177929344977772));
#59992=CARTESIAN_POINT('Ctrl Pts',(-16.499737824245,42.9994528692837,-0.156906377895304));
#59993=CARTESIAN_POINT('Ctrl Pts',(-17.4996344297213,42.9993693144289,-0.167744837011927));
#59994=CARTESIAN_POINT('Ctrl Pts',(-16.5005671676994,44.0011697501096,-0.0360034841747721));
#59995=CARTESIAN_POINT('Ctrl Pts',(-16.5004336035839,43.0009063138008,-0.0317784680747621));
#59996=CARTESIAN_POINT('Ctrl Pts',(-17.5006015414388,43.0010397779723,-0.0339426786824198));
#59997=CARTESIAN_POINT('Ctrl Pts',(-16.4978545553025,43.9955752404001,0.388390909530019));
#59998=CARTESIAN_POINT('Ctrl Pts',(-16.4983604076717,42.9965730007167,0.34258128637437));
#59999=CARTESIAN_POINT('Ctrl Pts',(-17.4977245284721,42.9960668801614,0.366159780026568));
#60000=CARTESIAN_POINT('Ctrl Pts',(-16.488785846129,43.9768969118701,0.669479171266392));
#60001=CARTESIAN_POINT('Ctrl Pts',(-16.4914621272788,42.9821709666193,0.590248849637306));
#60002=CARTESIAN_POINT('Ctrl Pts',(-17.488106200346,42.9794639216913,0.631158814660471));
#60003=CARTESIAN_POINT('Ctrl Pts',(-16.4566137829713,43.9102406346531,1.22805693613211));
#60004=CARTESIAN_POINT('Ctrl Pts',(-16.4667388442969,42.9303002753056,1.08490481084554));
#60005=CARTESIAN_POINT('Ctrl Pts',(-17.4539843153664,42.9202138974404,1.15776411487348));
#60006=CARTESIAN_POINT('Ctrl Pts',(-16.4335093295897,43.8622622073091,1.50554633472257));
#60007=CARTESIAN_POINT('Ctrl Pts',(-16.4489907660971,42.8929980278654,1.33109833842561));
#60008=CARTESIAN_POINT('Ctrl Pts',(-17.4294795919199,42.8775664063642,1.41937028185803));
#60009=CARTESIAN_POINT('Ctrl Pts',(-16.3960891495453,43.783793740335,1.85015317363005));
#60010=CARTESIAN_POINT('Ctrl Pts',(-16.4197798825902,42.8310926576272,1.63991769895437));
#60011=CARTESIAN_POINT('Ctrl Pts',(-17.3897915222624,42.8078166581088,1.74425215023244));
#60012=CARTESIAN_POINT('Ctrl Pts',(-16.3881779026531,43.767173088473,1.91896157031875));
#60013=CARTESIAN_POINT('Ctrl Pts',(-16.4136093423201,42.817995097094,1.70150596722071));
#60014=CARTESIAN_POINT('Ctrl Pts',(-17.3814008058283,42.7930427452666,1.80912201914365));
#60015=CARTESIAN_POINT('Ctrl Pts',(-16.375673948842,43.740841555206,2.0220039170481));
#60016=CARTESIAN_POINT('Ctrl Pts',(-16.4038270264028,42.7971893690875,1.79393530076847));
#60017=CARTESIAN_POINT('Ctrl Pts',(-17.3681390366586,42.7696369379822,1.90626631910862));
#60018=CARTESIAN_POINT('Ctrl Pts',(-16.3713997812811,43.7318309227685,2.05632298830878));
#60019=CARTESIAN_POINT('Ctrl Pts',(-16.4004812785263,42.7900667948439,1.82472882562818));
#60020=CARTESIAN_POINT('Ctrl Pts',(-17.3636058286238,42.7616274868815,1.93862099907206));
#60021=CARTESIAN_POINT('Ctrl Pts',(-16.3626396751579,43.7133407089755,2.12490420765856));
#60022=CARTESIAN_POINT('Ctrl Pts',(-16.3936154941633,42.7754354074154,1.88631707234903));
#60023=CARTESIAN_POINT('Ctrl Pts',(-17.3543148069932,42.7451917413354,2.0032766940958));
#60024=CARTESIAN_POINT('Ctrl Pts',(-16.3581504674953,43.7038542075336,2.15919050412873));
#60025=CARTESIAN_POINT('Ctrl Pts',(-16.3900932136698,42.7679218136654,1.9171321516777));
#60026=CARTESIAN_POINT('Ctrl Pts',(-17.3495535260841,42.7367592956301,2.03560047527918));
#60027=CARTESIAN_POINT('Ctrl Pts',(-16.335218649852,43.6553329579177,2.33016678950607));
#60028=CARTESIAN_POINT('Ctrl Pts',(-16.3721055730023,42.7295090646878,2.07069458061821));
#60029=CARTESIAN_POINT('Ctrl Pts',(-17.3252319015473,42.6936292957481,2.19679023923976));
#60030=CARTESIAN_POINT('Ctrl Pts',(-16.315354751774,43.6131097667714,2.46525055695651));
#60031=CARTESIAN_POINT('Ctrl Pts',(-16.3564409704719,42.6959272836267,2.19259820200646));
#60032=CARTESIAN_POINT('Ctrl Pts',(-17.3041641304931,42.6560975705951,2.32414193923568));
#60033=CARTESIAN_POINT('Ctrl Pts',(-16.2515056057596,43.4765147512805,2.8655905997197));
#60034=CARTESIAN_POINT('Ctrl Pts',(-16.3058885440615,42.5869423044208,2.55446830067613));
#60035=CARTESIAN_POINT('Ctrl Pts',(-17.2364453397946,42.5346797786526,2.7015668953238));
#60036=CARTESIAN_POINT('Ctrl Pts',(-16.2032672081898,43.3722448995847,3.12594764367366));
#60037=CARTESIAN_POINT('Ctrl Pts',(-16.2673330709852,42.5030995032564,2.7919929023725));
#60038=CARTESIAN_POINT('Ctrl Pts',(-17.1852834023163,42.441995466392,2.94702134755456));
#60039=CARTESIAN_POINT('Ctrl Pts',(-16.0968875664402,43.1381380127393,3.63422998231717));
#60040=CARTESIAN_POINT('Ctrl Pts',(-16.1809970935074,42.3122776252218,3.25988799511517));
#60041=CARTESIAN_POINT('Ctrl Pts',(-17.07245651017,42.2339004556738,3.42621008435598));
#60042=CARTESIAN_POINT('Ctrl Pts',(-16.0387426559475,43.0082992884229,3.88215383492437));
#60043=CARTESIAN_POINT('Ctrl Pts',(-16.1333904856796,42.2057238967836,3.48991370242924));
#60044=CARTESIAN_POINT('Ctrl Pts',(-17.0107876651219,42.118488256322,3.65994300926234));
#60045=CARTESIAN_POINT('Ctrl Pts',(-15.9607089630699,42.8300074294681,4.18445557032663));
#60046=CARTESIAN_POINT('Ctrl Pts',(-16.0682434684036,42.0567601433772,3.77421115204722));
#60047=CARTESIAN_POINT('Ctrl Pts',(-16.9280246578707,41.9600066039851,3.94494127844591));
#60048=CARTESIAN_POINT('Ctrl Pts',(-15.9448345125254,42.7935473084438,4.2445349020985));
#60049=CARTESIAN_POINT('Ctrl Pts',(-16.0550169591108,42.026372413421,3.83055888715714));
#60050=CARTESIAN_POINT('Ctrl Pts',(-16.9111881192775,41.9275976074833,4.00158172585483));
#60051=CARTESIAN_POINT('Ctrl Pts',(-15.9125710995365,42.7190148602521,4.3639323057479));
#60052=CARTESIAN_POINT('Ctrl Pts',(-16.0280522148975,41.964087720814,3.94277369967183));
#60053=CARTESIAN_POINT('Ctrl Pts',(-16.8769693480609,41.8613465424687,4.1141449347411));
#60054=CARTESIAN_POINT('Ctrl Pts',(-15.8961777996028,42.6809324048149,4.42326572017825));
#60055=CARTESIAN_POINT('Ctrl Pts',(-16.0143130159987,41.9321895117794,3.99865250806258));
#60056=CARTESIAN_POINT('Ctrl Pts',(-16.8595825146128,41.8274954710167,4.17008216045151));
#60057=CARTESIAN_POINT('Ctrl Pts',(-15.8462844618934,42.5643109368609,4.60002845907672));
#60058=CARTESIAN_POINT('Ctrl Pts',(-15.9724388258778,41.8344100525786,4.16519179553658));
#60059=CARTESIAN_POINT('Ctrl Pts',(-16.8066653386068,41.723831943736,4.33672716677812));
#60060=CARTESIAN_POINT('Ctrl Pts',(-15.8122905956358,42.4839122053499,4.71544824060082));
#60061=CARTESIAN_POINT('Ctrl Pts',(-15.9437057928047,41.7665897154923,4.27457431431909));
#60062=CARTESIAN_POINT('Ctrl Pts',(-16.7706112375754,41.652366404853,4.44554042885686));
#60063=CARTESIAN_POINT('Ctrl Pts',(-15.708466257085,42.2349319229732,5.05470392926197));
#60064=CARTESIAN_POINT('Ctrl Pts',(-15.8557182823553,41.5561640523473,4.59624091151791));
#60065=CARTESIAN_POINT('Ctrl Pts',(-16.6604945155305,41.4310505980033,4.76537744171326));
#60066=CARTESIAN_POINT('Ctrl Pts',(-15.6367937805477,42.0585895493903,5.27155542705688));
#60067=CARTESIAN_POINT('Ctrl Pts',(-15.7941524221352,41.4054489545328,4.80429063353521));
#60068=CARTESIAN_POINT('Ctrl Pts',(-16.5844782517039,41.274301821729,4.96981656414753));
#60069=CARTESIAN_POINT('Ctrl Pts',(-15.490346672854,41.6855007303992,5.68751055477781));
#60070=CARTESIAN_POINT('Ctrl Pts',(-15.6669541386688,41.0833353282907,5.20593767654318));
#60071=CARTESIAN_POINT('Ctrl Pts',(-16.42915556251,40.9426673158617,5.36196281266631));
#60072=CARTESIAN_POINT('Ctrl Pts',(-15.4155675047962,41.4887542028889,5.88661251495239));
#60073=CARTESIAN_POINT('Ctrl Pts',(-15.6013785695094,40.9122288799408,5.39970005563699));
#60074=CARTESIAN_POINT('Ctrl Pts',(-16.3498443229104,40.7677815136044,5.54966836406231));
#60075=CARTESIAN_POINT('Ctrl Pts',(-15.3024448812762,41.1779991716065,6.17216839972268));
#60076=CARTESIAN_POINT('Ctrl Pts',(-15.5009241601739,40.6387285873814,5.6799934650858));
#60077=CARTESIAN_POINT('Ctrl Pts',(-16.2298657833509,40.4915548192431,5.81887929950314));
#60078=CARTESIAN_POINT('Ctrl Pts',(-15.2645790020526,41.0718024829547,6.26516634094168));
#60079=CARTESIAN_POINT('Ctrl Pts',(-15.4672614165944,40.5452444380058,5.77127906622756));
#60080=CARTESIAN_POINT('Ctrl Pts',(-16.1897050020046,40.3971577625623,5.90655412600363));
#60081=CARTESIAN_POINT('Ctrl Pts',(-15.2077254227751,40.9084929741541,6.4013676517502));
#60082=CARTESIAN_POINT('Ctrl Pts',(-15.4164278105277,40.4007199180155,5.90553521152224));
#60083=CARTESIAN_POINT('Ctrl Pts',(-16.1294057515143,40.2519937548357,6.03495940239176));
#60084=CARTESIAN_POINT('Ctrl Pts',(-15.1887651989012,40.853386989109,6.44621852703614));
#60085=CARTESIAN_POINT('Ctrl Pts',(-15.3994674120309,40.3519488749432,5.94974031533987));
#60086=CARTESIAN_POINT('Ctrl Pts',(-16.1092964229923,40.2030106569473,6.07724305571356));
#60087=CARTESIAN_POINT('Ctrl Pts',(-15.1508585131677,40.7418148130405,6.53481506085914));
#60088=CARTESIAN_POINT('Ctrl Pts',(-15.365491794666,40.2530328359572,6.03717495128596));
#60089=CARTESIAN_POINT('Ctrl Pts',(-16.0690923625353,40.1038353894078,6.16076840762205));
#60090=CARTESIAN_POINT('Ctrl Pts',(-15.1319787469483,40.685544542223,6.57840481672826));
#60091=CARTESIAN_POINT('Ctrl Pts',(-15.348535637605,40.2030632212813,6.08025593853515));
#60092=CARTESIAN_POINT('Ctrl Pts',(-16.0490683678638,40.0538173708934,6.20186312687394));
#60093=CARTESIAN_POINT('Ctrl Pts',(-15.0380664911524,40.4019030685421,6.79276143414887));
#60094=CARTESIAN_POINT('Ctrl Pts',(-15.2644245680603,39.9519367964584,6.29138993605124));
#60095=CARTESIAN_POINT('Ctrl Pts',(-15.9494644607597,39.8016916163679,6.40395017364007));
#60096=CARTESIAN_POINT('Ctrl Pts',(-14.9644461532019,40.1675514041411,6.95288768593992));
#60097=CARTESIAN_POINT('Ctrl Pts',(-15.1976171693671,39.7421821058477,6.45092268656129));
#60098=CARTESIAN_POINT('Ctrl Pts',(-15.8713822833035,39.5933790259089,6.55491094954876));
#60099=CARTESIAN_POINT('Ctrl Pts',(-14.8222211698946,39.6838140960417,7.25114166432459));
#60100=CARTESIAN_POINT('Ctrl Pts',(-15.06786594057,39.3068953284827,6.74885869506734));
#60101=CARTESIAN_POINT('Ctrl Pts',(-15.7205376048291,39.1633903075869,6.83609315171071));
#60102=CARTESIAN_POINT('Ctrl Pts',(-14.7536128479239,39.4344290298586,7.38926853498414));
#60103=CARTESIAN_POINT('Ctrl Pts',(-15.0048054725226,39.0812939904251,6.88766092280371));
#60104=CARTESIAN_POINT('Ctrl Pts',(-15.6477712019922,38.9417146931311,6.96631377005003));
#60105=CARTESIAN_POINT('Ctrl Pts',(-14.6235443336384,38.9199395169773,7.64345031191053));
#60106=CARTESIAN_POINT('Ctrl Pts',(-14.8848011659622,38.6139543580119,7.14351801279062));
#60107=CARTESIAN_POINT('Ctrl Pts',(-15.5098197481496,38.4843906818341,7.20594642230858));
#60108=CARTESIAN_POINT('Ctrl Pts',(-14.5620800221653,38.6548384656211,7.7595087284317));
#60109=CARTESIAN_POINT('Ctrl Pts',(-14.827716689627,38.3720620877045,7.26095612384862));
#60110=CARTESIAN_POINT('Ctrl Pts',(-15.4446303262328,38.2487453026412,7.31536176370244));
#60111=CARTESIAN_POINT('Ctrl Pts',(-14.4912109590877,38.3128451067789,7.89022745753408));
#60112=CARTESIAN_POINT('Ctrl Pts',(-14.7615399553527,38.0581196581985,7.39373762359809));
#60113=CARTESIAN_POINT('Ctrl Pts',(-15.369466168806,37.944751206059,7.43859827658201));
#60114=CARTESIAN_POINT('Ctrl Pts',(-14.4773360216078,38.2439139811986,7.91565127929397));
#60115=CARTESIAN_POINT('Ctrl Pts',(-14.7486090785329,37.9949822886081,7.41950389459761));
#60116=CARTESIAN_POINT('Ctrl Pts',(-15.3547503258741,37.883479094363,7.46256686250324));
#60117=CARTESIAN_POINT('Ctrl Pts',(-14.4570026893877,38.1396985883734,7.95268958299778));
#60118=CARTESIAN_POINT('Ctrl Pts',(-14.7296347176249,37.8994093453111,7.45707777466083));
#60119=CARTESIAN_POINT('Ctrl Pts',(-15.3331846705994,37.7908431896831,7.49748512881753));
#60120=CARTESIAN_POINT('Ctrl Pts',(-14.4502995623675,38.1047958815478,7.9648621653037));
#60121=CARTESIAN_POINT('Ctrl Pts',(-14.7233795289916,37.8674039475413,7.46942463090051));
#60122=CARTESIAN_POINT('Ctrl Pts',(-15.326075293378,37.7598185613842,7.50896096392519));
#60123=CARTESIAN_POINT('Ctrl Pts',(-14.4370862536553,38.0348626145466,7.98878759631039));
#60124=CARTESIAN_POINT('Ctrl Pts',(-14.711044089513,37.8032526976823,7.49369902639856));
#60125=CARTESIAN_POINT('Ctrl Pts',(-15.3120611781612,37.6976556573663,7.531516925812));
#60126=CARTESIAN_POINT('Ctrl Pts',(-14.430578191227,37.9998443555349,8.00053668324475));
#60127=CARTESIAN_POINT('Ctrl Pts',(-14.7049654891278,37.7711173950731,7.50562346769514));
#60128=CARTESIAN_POINT('Ctrl Pts',(-15.3051586876244,37.6665283160382,7.54259350608998));
#60129=CARTESIAN_POINT('Ctrl Pts',(-14.3985378950991,37.8244951111472,8.05821896776018));
#60130=CARTESIAN_POINT('Ctrl Pts',(-14.6750683621745,37.6103672676509,7.56410181532715));
#60131=CARTESIAN_POINT('Ctrl Pts',(-15.2711765555705,37.5106623209909,7.59697411101706));
#60132=CARTESIAN_POINT('Ctrl Pts',(-14.3745058364078,37.6833906877742,8.10096493484399));
#60133=CARTESIAN_POINT('Ctrl Pts',(-14.652561930448,37.4806229720141,7.60757184213281));
#60134=CARTESIAN_POINT('Ctrl Pts',(-15.2456880081703,37.3852361669233,7.63727333921995));
#60135=CARTESIAN_POINT('Ctrl Pts',(-14.3074780704631,37.2575991659697,8.21914076587046));
#60136=CARTESIAN_POINT('Ctrl Pts',(-14.5898331467566,37.0893377713944,7.72760627073598));
#60137=CARTESIAN_POINT('Ctrl Pts',(-15.1745979538034,37.0067548141695,7.74868489717074));
#60138=CARTESIAN_POINT('Ctrl Pts',(-14.2695523034726,36.9704386282229,8.28453464061196));
#60139=CARTESIAN_POINT('Ctrl Pts',(-14.5540974775854,36.8241663199945,7.79441727640368));
#60140=CARTESIAN_POINT('Ctrl Pts',(-15.1343736550051,36.7515010028509,7.81033568794618));
#60141=CARTESIAN_POINT('Ctrl Pts',(-14.2086105787285,36.3893814021093,8.38862459376293));
#60142=CARTESIAN_POINT('Ctrl Pts',(-14.4967075641971,36.2872858361014,7.90063819784113));
#60143=CARTESIAN_POINT('Ctrl Pts',(-15.069738492784,36.2350056907777,7.90846763065641));
#60144=CARTESIAN_POINT('Ctrl Pts',(-14.1855946049829,36.0954849072401,8.42732167623407));
#60145=CARTESIAN_POINT('Ctrl Pts',(-14.474938277723,36.0150460990806,7.94027178393654));
#60146=CARTESIAN_POINT('Ctrl Pts',(-15.04532761125,35.9737643619689,7.94494972814297));
#60147=CARTESIAN_POINT('Ctrl Pts',(-14.1632592796937,35.6493675288365,8.46476803043535));
#60148=CARTESIAN_POINT('Ctrl Pts',(-14.4538374531707,35.601719694416,7.97857185535198));
#60149=CARTESIAN_POINT('Ctrl Pts',(-15.0216386300259,35.5772155811991,7.98025268877251));
#60150=CARTESIAN_POINT('Ctrl Pts',(-14.1578452220156,35.4997817266829,8.47381023741147));
#60151=CARTESIAN_POINT('Ctrl Pts',(-14.4487195544893,35.4631107873063,7.98782407910831));
#60152=CARTESIAN_POINT('Ctrl Pts',(-15.0158964475708,35.4442504237115,7.98877732802181));
#60153=CARTESIAN_POINT('Ctrl Pts',(-14.1528931524912,35.2740434072532,8.48207673460457));
#60154=CARTESIAN_POINT('Ctrl Pts',(-14.4440400975708,35.2539384493497,7.99627922136717));
#60155=CARTESIAN_POINT('Ctrl Pts',(-15.0106442526529,35.2435941397839,7.99657065897525));
#60156=CARTESIAN_POINT('Ctrl Pts',(-14.1517706094402,35.1985706100121,8.48394895723216));
#60157=CARTESIAN_POINT('Ctrl Pts',(-14.442979184077,35.184001549869,7.9981943881281));
#60158=CARTESIAN_POINT('Ctrl Pts',(-15.0094536766753,35.1765072088985,7.99833571715932));
#60159=CARTESIAN_POINT('Ctrl Pts',(-14.1508941306251,35.0850155880073,8.4854107517919));
#60160=CARTESIAN_POINT('Ctrl Pts',(-14.4421509241428,35.078778187705,7.99968953263258));
#60161=CARTESIAN_POINT('Ctrl Pts',(-15.0085240779375,35.0755694115626,7.99971384012147));
#60162=CARTESIAN_POINT('Ctrl Pts',(-14.150736560916,35.0470814239072,8.48567350216556));
#60163=CARTESIAN_POINT('Ctrl Pts',(-14.4420020169164,35.0436268600821,7.99995828626213));
#60164=CARTESIAN_POINT('Ctrl Pts',(-15.0083569585472,35.0418501545842,7.99996155087807));
#60165=CARTESIAN_POINT('Ctrl Pts',(-14.150692918513,34.9712377388823,8.48574627995365));
#60166=CARTESIAN_POINT('Ctrl Pts',(-14.4419607755292,34.9733482312172,8.0000327238654));
#60167=CARTESIAN_POINT('Ctrl Pts',(-15.0083106711502,34.9744335456731,8.00003016290435));
#60168=CARTESIAN_POINT('Ctrl Pts',(-14.1508066226917,34.9333329107061,8.48555667952094));
#60169=CARTESIAN_POINT('Ctrl Pts',(-14.4420682290436,34.9382240120611,7.99983879114063));
#60170=CARTESIAN_POINT('Ctrl Pts',(-15.0084312664928,34.940740365072,7.99985141504979));
#60171=CARTESIAN_POINT('Ctrl Pts',(-14.1520509011363,34.7438936238919,8.48348153993902));
#60172=CARTESIAN_POINT('Ctrl Pts',(-14.4432440959225,34.7626780463408,7.99771623713472));
#60173=CARTESIAN_POINT('Ctrl Pts',(-15.0097509557443,34.7723498879043,7.9978950544351));
#60174=CARTESIAN_POINT('Ctrl Pts',(-14.1552091806869,34.5926136214512,8.4782167591127));
#60175=CARTESIAN_POINT('Ctrl Pts',(-14.4462304856527,34.6224662811345,7.99232810421143));
#60176=CARTESIAN_POINT('Ctrl Pts',(-15.0131006462177,34.6378787746227,7.99293162477818));
#60177=CARTESIAN_POINT('Ctrl Pts',(-14.1631498026642,34.366097861864,8.46494029855902));
#60178=CARTESIAN_POINT('Ctrl Pts',(-14.4537301008296,34.4126736274608,7.97875461899514));
#60179=CARTESIAN_POINT('Ctrl Pts',(-15.0215225179599,34.4365314327682,7.98041509627186));
#60180=CARTESIAN_POINT('Ctrl Pts',(-14.1663304572642,34.2906600038508,8.45961782992988));
#60181=CARTESIAN_POINT('Ctrl Pts',(-14.4567347009781,34.34279668575,7.97331176954809));
#60182=CARTESIAN_POINT('Ctrl Pts',(-15.0248959395469,34.3694755589792,7.975397280748));
#60183=CARTESIAN_POINT('Ctrl Pts',(-14.1718962020967,34.1776041375939,8.45028822882502));
#60184=CARTESIAN_POINT('Ctrl Pts',(-14.4619896761171,34.2381138641883,7.96377525778024));
#60185=CARTESIAN_POINT('Ctrl Pts',(-15.0307990022117,34.2689814556387,7.96660169720576));
#60186=CARTESIAN_POINT('Ctrl Pts',(-14.1738839055404,34.1399356702887,8.44695401845093));
#60187=CARTESIAN_POINT('Ctrl Pts',(-14.4638665061005,34.2032333257984,7.96036678089891));
#60188=CARTESIAN_POINT('Ctrl Pts',(-15.0329071725568,34.2354983735906,7.96345833389448));
#60189=CARTESIAN_POINT('Ctrl Pts',(-14.1781231744824,34.0646323657967,8.43983651540518));
#60190=CARTESIAN_POINT('Ctrl Pts',(-14.4678686428001,34.1335117477056,7.95309163191476));
#60191=CARTESIAN_POINT('Ctrl Pts',(-15.0374033668614,34.1685621029298,7.95674823001028));
#60192=CARTESIAN_POINT('Ctrl Pts',(-14.1803761277451,34.026976116557,8.43605088762219));
#60193=CARTESIAN_POINT('Ctrl Pts',(-14.4699954006696,34.0986496666099,7.9492223146372));
#60194=CARTESIAN_POINT('Ctrl Pts',(-15.039792862775,34.1350898813783,7.953179288052));
#60195=CARTESIAN_POINT('Ctrl Pts',(-14.2018025764259,33.6887269670264,8.40001146214908));
#60196=CARTESIAN_POINT('Ctrl Pts',(-14.4902406725494,33.7851897713294,7.91234974711415));
#60197=CARTESIAN_POINT('Ctrl Pts',(-15.062517883968,33.8344239707358,7.91920272479425));
#60198=CARTESIAN_POINT('Ctrl Pts',(-14.2289622534947,33.3934618841932,8.35411823426493));
#60199=CARTESIAN_POINT('Ctrl Pts',(-14.5159096719755,33.5118586162235,7.86536934014895));
#60200=CARTESIAN_POINT('Ctrl Pts',(-15.091323602403,33.5719661192377,7.87593638279283));
#60201=CARTESIAN_POINT('Ctrl Pts',(-14.297587136116,32.8129757621643,8.2361192541527));
#60202=CARTESIAN_POINT('Ctrl Pts',(-14.5804718486074,32.975939942154,7.74503244923851));
#60203=CARTESIAN_POINT('Ctrl Pts',(-15.1641075683963,33.0559784553022,7.76469155241571));
#60204=CARTESIAN_POINT('Ctrl Pts',(-14.3390533631708,32.5277562904371,8.16400873147055));
#60205=CARTESIAN_POINT('Ctrl Pts',(-14.6194905451471,32.7128565901746,7.67142630106037));
#60206=CARTESIAN_POINT('Ctrl Pts',(-15.2080869006233,32.8024500359307,7.6967085685757));
#60207=CARTESIAN_POINT('Ctrl Pts',(-14.4344512245411,31.9668958072417,7.99412958149491));
#60208=CARTESIAN_POINT('Ctrl Pts',(-14.7087759143519,32.1972833069676,7.49877760542043));
#60209=CARTESIAN_POINT('Ctrl Pts',(-15.3092664499803,32.3039073842282,7.53655314061732));
#60210=CARTESIAN_POINT('Ctrl Pts',(-14.4883838105694,31.691255013237,7.89636074701349));
#60211=CARTESIAN_POINT('Ctrl Pts',(-14.7592010426945,31.9443746233512,7.39939956315832));
#60212=CARTESIAN_POINT('Ctrl Pts',(-15.3664676782412,32.0588933451493,7.44438050229219));
#60213=CARTESIAN_POINT('Ctrl Pts',(-14.5550635668316,31.3864313723232,7.77176756628671));
#60214=CARTESIAN_POINT('Ctrl Pts',(-14.8209199446041,31.6669143175934,7.27386759669347));
#60215=CARTESIAN_POINT('Ctrl Pts',(-15.4371886314425,31.7879389976144,7.32691891770422));
#60216=CARTESIAN_POINT('Ctrl Pts',(-14.5625558613898,31.352635473547,7.75772049298618));
#60217=CARTESIAN_POINT('Ctrl Pts',(-14.827877420134,31.6360499048315,7.25966604997201));
#60218=CARTESIAN_POINT('Ctrl Pts',(-15.4451350045509,31.7578981987159,7.31367588564878));
#60219=CARTESIAN_POINT('Ctrl Pts',(-14.5777038502899,31.2851903557158,7.72921800162461));
#60220=CARTESIAN_POINT('Ctrl Pts',(-14.8419359589025,31.5744837961381,7.2308617271771));
#60221=CARTESIAN_POINT('Ctrl Pts',(-15.4612010532912,31.697946982851,7.28680485001122));
#60222=CARTESIAN_POINT('Ctrl Pts',(-14.5853648004003,31.2515184553974,7.71475260653216));
#60223=CARTESIAN_POINT('Ctrl Pts',(-14.849042235293,31.543760796002,7.21624805914054));
#60224=CARTESIAN_POINT('Ctrl Pts',(-15.469326303495,31.6680164047788,7.2731674405612));
#60225=CARTESIAN_POINT('Ctrl Pts',(-14.6085452032034,31.1509057610832,7.67082157327148));
#60226=CARTESIAN_POINT('Ctrl Pts',(-14.8705436711721,31.4519516854403,7.171859977806));
#60227=CARTESIAN_POINT('Ctrl Pts',(-15.4939115790748,31.5785828987784,7.2317509780494));
#60228=CARTESIAN_POINT('Ctrl Pts',(-14.6242529880176,31.0844047949656,7.64083891095088));
#60229=CARTESIAN_POINT('Ctrl Pts',(-14.8850903709531,31.3913603681064,7.14160216923058));
#60230=CARTESIAN_POINT('Ctrl Pts',(-15.5105713510105,31.5194709288242,7.20348449527989));
#60231=CARTESIAN_POINT('Ctrl Pts',(-14.6720790763943,30.8865851637151,7.54883265535859));
#60232=CARTESIAN_POINT('Ctrl Pts',(-14.929376159556,31.2110903439192,7.04872760978158));
#60233=CARTESIAN_POINT('Ctrl Pts',(-15.5612959899498,31.3436312567038,7.11674459069576));
#60234=CARTESIAN_POINT('Ctrl Pts',(-14.7048994575313,30.7569483641181,7.48475247389081));
#60235=CARTESIAN_POINT('Ctrl Pts',(-14.95966877612,31.0933259986506,6.98419535501427));
#60236=CARTESIAN_POINT('Ctrl Pts',(-15.5961054854356,31.2283985458312,7.05633229878906));
#60237=CARTESIAN_POINT('Ctrl Pts',(-14.8057173802565,30.3745068040017,7.28444119078806));
#60238=CARTESIAN_POINT('Ctrl Pts',(-15.052677543726,30.7458140689667,6.78241054451384));
#60239=CARTESIAN_POINT('Ctrl Pts',(-15.7030335847703,30.888450492549,6.86748664417107));
#60240=CARTESIAN_POINT('Ctrl Pts',(-14.8760647694745,30.1281517423914,7.14016324914458));
#60241=CARTESIAN_POINT('Ctrl Pts',(-15.1171363078512,30.5235314070459,6.63773030177344));
#60242=CARTESIAN_POINT('Ctrl Pts',(-15.7776444528623,30.6694682154397,6.73146703642075));
#60243=CARTESIAN_POINT('Ctrl Pts',(-15.0208334639485,29.6517703450343,6.83035843117765));
#60244=CARTESIAN_POINT('Ctrl Pts',(-15.2487759421767,30.0960400709944,6.32894683063836));
#60245=CARTESIAN_POINT('Ctrl Pts',(-15.9311870068286,30.2460180844943,6.43939515378203));
#60246=CARTESIAN_POINT('Ctrl Pts',(-15.0952589444123,29.4217455787918,6.66483128140236));
#60247=CARTESIAN_POINT('Ctrl Pts',(-15.3160581108554,29.8908120505933,6.16445964685839));
#60248=CARTESIAN_POINT('Ctrl Pts',(-16.0101231232976,30.0415516256819,6.28334262225704));
#60249=CARTESIAN_POINT('Ctrl Pts',(-15.1895776666482,29.1442442832826,6.4443022486447));
#60250=CARTESIAN_POINT('Ctrl Pts',(-15.4001942830716,29.6459545222953,5.94785171931794));
#60251=CARTESIAN_POINT('Ctrl Pts',(-16.1101581311846,29.79488380734,6.07543646335386));
#60252=CARTESIAN_POINT('Ctrl Pts',(-15.2085060076969,29.0892469278519,6.39951354132192));
#60253=CARTESIAN_POINT('Ctrl Pts',(-15.4171256703624,29.5972806483711,5.90370851153158));
#60254=CARTESIAN_POINT('Ctrl Pts',(-16.1302336446393,29.745997269232,6.03321141943556));
#60255=CARTESIAN_POINT('Ctrl Pts',(-15.2369722744217,29.0075062116329,6.33129394724583));
#60256=CARTESIAN_POINT('Ctrl Pts',(-15.4425151412656,29.5251196490867,5.83662745356123));
#60257=CARTESIAN_POINT('Ctrl Pts',(-16.160425139482,29.6733388547696,5.96889665059839));
#60258=CARTESIAN_POINT('Ctrl Pts',(-15.246473323653,28.980385210548,6.30838130181911));
#60259=CARTESIAN_POINT('Ctrl Pts',(-15.4509873595446,29.5011789547939,5.81409473052649));
#60260=CARTESIAN_POINT('Ctrl Pts',(-16.170502009992,29.6492312982821,5.94729550340031));
#60261=CARTESIAN_POINT('Ctrl Pts',(-15.2654961612181,28.926395398229,6.26220810975159));
#60262=CARTESIAN_POINT('Ctrl Pts',(-15.4679323239667,29.4535620737581,5.76872117594484));
#60263=CARTESIAN_POINT('Ctrl Pts',(-16.1906777466895,29.601240353964,5.90376522131281));
#60264=CARTESIAN_POINT('Ctrl Pts',(-15.2750230398706,28.8995124220965,6.23893492398287));
#60265=CARTESIAN_POINT('Ctrl Pts',(-15.4764096537653,29.4298736780045,5.74586728371073));
#60266=CARTESIAN_POINT('Ctrl Pts',(-16.2007820120252,29.5773443751773,5.88182417079429));
#60267=CARTESIAN_POINT('Ctrl Pts',(-15.3225922161938,28.7660296571919,6.12195830143935));
#60268=CARTESIAN_POINT('Ctrl Pts',(-15.5187963268113,29.3120701815224,5.63080434349472));
#60269=CARTESIAN_POINT('Ctrl Pts',(-16.2512341685254,29.4586930286934,5.77154317966401));
#60270=CARTESIAN_POINT('Ctrl Pts',(-15.3604967735573,28.6620554042277,6.02628494806573));
#60271=CARTESIAN_POINT('Ctrl Pts',(-15.552341978002,29.22088933467,5.5371846231952));
#60272=CARTESIAN_POINT('Ctrl Pts',(-16.2914359721255,29.3662714703737,5.68134607909259));
#60273=CARTESIAN_POINT('Ctrl Pts',(-15.4734024711476,28.3583437765312,5.73303598356708));
#60274=CARTESIAN_POINT('Ctrl Pts',(-15.6521452749257,28.9546179419119,5.25025045759224));
#60275=CARTESIAN_POINT('Ctrl Pts',(-16.4111844387542,29.0963055792408,5.40488240853399));
#60276=CARTESIAN_POINT('Ctrl Pts',(-15.5475928105337,28.166793334864,5.52924812560617));
#60277=CARTESIAN_POINT('Ctrl Pts',(-15.716867186315,28.7887594038429,5.0526403038573));
#60278=CARTESIAN_POINT('Ctrl Pts',(-16.4898711630596,28.9260385198999,5.21275917575155));
#60279=CARTESIAN_POINT('Ctrl Pts',(-15.6920332500668,27.804967416518,5.10493090212559));
#60280=CARTESIAN_POINT('Ctrl Pts',(-15.8416653101424,28.4777545766966,4.64442044202835));
#60281=CARTESIAN_POINT('Ctrl Pts',(-16.6430655678803,28.6044154813285,4.8127294699215));
#60282=CARTESIAN_POINT('Ctrl Pts',(-15.7622877731009,27.6346927109898,4.88440241921411));
#60283=CARTESIAN_POINT('Ctrl Pts',(-15.9016653391294,28.3329345034696,4.43369484971485));
#60284=CARTESIAN_POINT('Ctrl Pts',(-16.7175779415832,28.4530601877117,4.6048238295626));
#60285=CARTESIAN_POINT('Ctrl Pts',(-15.8634153592665,27.3953869383753,4.54052076838177));
#60286=CARTESIAN_POINT('Ctrl Pts',(-15.9868838517309,28.1316515312056,4.10893296665195));
#60287=CARTESIAN_POINT('Ctrl Pts',(-16.8248344717416,28.2403439451399,4.280625640225));
#60288=CARTESIAN_POINT('Ctrl Pts',(-15.8964154242514,27.3183086387693,4.42370773816891));
#60289=CARTESIAN_POINT('Ctrl Pts',(-16.0146143413019,28.0669533026489,3.99868427600105));
#60290=CARTESIAN_POINT('Ctrl Pts',(-16.8598345410939,28.1718299012522,4.17049887771516));
#60291=CARTESIAN_POINT('Ctrl Pts',(-15.9446833059184,27.2068010501802,4.24510042840518));
#60292=CARTESIAN_POINT('Ctrl Pts',(-16.0548906467027,27.9739186191265,3.83109036355919));
#60293=CARTESIAN_POINT('Ctrl Pts',(-16.9110277485907,28.0727120445427,4.00211488200807));
#60294=CARTESIAN_POINT('Ctrl Pts',(-15.9605671695884,27.1703172329925,4.18499971903105));
#60295=CARTESIAN_POINT('Ctrl Pts',(-16.0681256678962,27.9435097431242,3.7747202284785));
#60296=CARTESIAN_POINT('Ctrl Pts',(-16.9278742708902,28.0402819849552,3.94545428055366));
#60297=CARTESIAN_POINT('Ctrl Pts',(-15.9840630498228,27.1166326670936,4.09398463298263));
#60298=CARTESIAN_POINT('Ctrl Pts',(-16.0876324266849,27.8989052244231,3.68960145288528));
#60299=CARTESIAN_POINT('Ctrl Pts',(-16.9527941436941,27.9925623707134,3.85964881224669));
#60300=CARTESIAN_POINT('Ctrl Pts',(-15.9918400182461,27.098911365518,4.06350224576308));
#60301=CARTESIAN_POINT('Ctrl Pts',(-16.0940844067552,27.8841885644318,3.66110082717283));
#60302=CARTESIAN_POINT('Ctrl Pts',(-16.9610424436527,27.9768101027221,3.83091120811858));
#60303=CARTESIAN_POINT('Ctrl Pts',(-16.0072802673827,27.0638183876329,4.00224638321511));
#60304=CARTESIAN_POINT('Ctrl Pts',(-16.1068754781049,27.8550811453129,3.60388755733143));
#60305=CARTESIAN_POINT('Ctrl Pts',(-16.9774184653475,27.9456163445231,3.77316157340969));
#60306=CARTESIAN_POINT('Ctrl Pts',(-16.0149484597681,27.0464356133835,3.97145286285566));
#60307=CARTESIAN_POINT('Ctrl Pts',(-16.11321832627,27.8406819961272,3.57515643717542));
#60308=CARTESIAN_POINT('Ctrl Pts',(-16.9855513967497,27.9301649896533,3.74413064513307));
#60309=CARTESIAN_POINT('Ctrl Pts',(-16.0833253347986,26.8918211440726,3.69342860679508));
#60310=CARTESIAN_POINT('Ctrl Pts',(-16.1700064472163,27.7120571742295,3.3145971632474));
#60311=CARTESIAN_POINT('Ctrl Pts',(-17.0580723245784,27.7927299060094,3.48202023522934));
#60312=CARTESIAN_POINT('Ctrl Pts',(-16.1392489563977,26.7681000791065,3.44139585389464));
#60313=CARTESIAN_POINT('Ctrl Pts',(-16.2154998129262,27.611079704592,3.08181765987248));
#60314=CARTESIAN_POINT('Ctrl Pts',(-17.1173852570175,27.6827556258494,3.24441359968121));
#60315=CARTESIAN_POINT('Ctrl Pts',(-16.2403199527415,26.5474550953827,2.92755360879577));
#60316=CARTESIAN_POINT('Ctrl Pts',(-16.2970459414564,27.4321275309776,2.61077340535992));
#60317=CARTESIAN_POINT('Ctrl Pts',(-17.2245817678271,27.4866267514743,2.7599832001616));
#60318=CARTESIAN_POINT('Ctrl Pts',(-16.2854701813921,26.4505327273823,2.66574409615585));
#60319=CARTESIAN_POINT('Ctrl Pts',(-16.3329171219314,27.3545890540287,2.37293766614214));
#60320=CARTESIAN_POINT('Ctrl Pts',(-17.272468374468,27.4004735355853,2.51315941724635));
#60321=CARTESIAN_POINT('Ctrl Pts',(-16.3638891417636,26.2837240365077,2.13210289884751));
#60322=CARTESIAN_POINT('Ctrl Pts',(-16.3948333150909,27.2217630392128,1.89119238259305));
#60323=CARTESIAN_POINT('Ctrl Pts',(-17.3556399985759,27.252199143428,2.01006333898577));
#60324=CARTESIAN_POINT('Ctrl Pts',(-16.3971609665106,26.2138347665803,1.86027258862789));
#60325=CARTESIAN_POINT('Ctrl Pts',(-16.4207214647061,27.1668306081169,1.64783726428005));
#60326=CARTESIAN_POINT('Ctrl Pts',(-17.3909282981186,27.1900753483798,1.75379233941467));
#60327=CARTESIAN_POINT('Ctrl Pts',(-16.4372282316227,26.1301157641184,1.44461189527185));
#60328=CARTESIAN_POINT('Ctrl Pts',(-16.4517534962573,27.1012636221844,1.27786031263812));
#60329=CARTESIAN_POINT('Ctrl Pts',(-17.4334238818719,27.1156584568399,1.36192367232642));
#60330=CARTESIAN_POINT('Ctrl Pts',(-16.4489425836071,26.1057357203802,1.30473676381471));
#60331=CARTESIAN_POINT('Ctrl Pts',(-16.4607946572,27.0822242725002,1.15354204459136));
#60332=CARTESIAN_POINT('Ctrl Pts',(-17.4458481948988,27.0939873072066,1.23005486149115));
#60333=CARTESIAN_POINT('Ctrl Pts',(-16.4614235356195,26.0798156556365,1.12817920332052));
#60334=CARTESIAN_POINT('Ctrl Pts',(-16.4704032550175,27.0620254439469,0.997028004066201));
#60335=CARTESIAN_POINT('Ctrl Pts',(-17.4590855680403,27.0709472494042,1.06360328933017));
#60336=CARTESIAN_POINT('Ctrl Pts',(-16.4638105601819,26.074861696503,1.09279299652423));
#60337=CARTESIAN_POINT('Ctrl Pts',(-16.4722410434965,27.0581642796167,0.965648605363661));
#60338=CARTESIAN_POINT('Ctrl Pts',(-17.4616172607913,27.0665437301925,1.03024255564937));
#60339=CARTESIAN_POINT('Ctrl Pts',(-16.4683507346043,26.0654443842168,1.02209528756755));
#60340=CARTESIAN_POINT('Ctrl Pts',(-16.4757345383337,27.0508278725685,0.902983985062077));
#60341=CARTESIAN_POINT('Ctrl Pts',(-17.4664325973152,27.0581727860028,0.963591516895074));
#60342=CARTESIAN_POINT('Ctrl Pts',(-16.470506063436,26.0609765048028,0.986753620408229));
#60343=CARTESIAN_POINT('Ctrl Pts',(-16.4773917386444,27.047349490258,0.871673646590079));
#60344=CARTESIAN_POINT('Ctrl Pts',(-17.4687185521219,27.0542013375728,0.930272773451819));
#60345=CARTESIAN_POINT('Ctrl Pts',(-16.4766286018102,26.0482910800257,0.880750072548012));
#60346=CARTESIAN_POINT('Ctrl Pts',(-16.4820979767805,27.0374753525219,0.777776718980477));
#60347=CARTESIAN_POINT('Ctrl Pts',(-17.4752121534494,27.0429254045267,0.830336768726166));
#60348=CARTESIAN_POINT('Ctrl Pts',(-16.4802523787863,26.0407916272951,0.810109642405695));
#60349=CARTESIAN_POINT('Ctrl Pts',(-16.4848785011,27.0316471633613,0.715279089642234));
#60350=CARTESIAN_POINT('Ctrl Pts',(-17.4790555532451,27.0362592242133,0.763739730217897));
#60351=CARTESIAN_POINT('Ctrl Pts',(-16.4897560121036,26.0211373031105,0.598273404163521));
#60352=CARTESIAN_POINT('Ctrl Pts',(-16.4921690314085,27.0163743171162,0.527896985305773));
#60353=CARTESIAN_POINT('Ctrl Pts',(-17.4891351643784,27.0187887139739,0.564028798530454));
#60354=CARTESIAN_POINT('Ctrl Pts',(-16.4942684087839,26.0118246449525,0.457162601989202));
#60355=CARTESIAN_POINT('Ctrl Pts',(-16.4956179815424,27.0091615199262,0.403342719886046));
#60356=CARTESIAN_POINT('Ctrl Pts',(-17.4939210395996,27.0105107954566,0.430995045648165));
#60357=CARTESIAN_POINT('Ctrl Pts',(-16.4996728834952,26.0006733566253,0.175164846125518));
#60358=CARTESIAN_POINT('Ctrl Pts',(-16.4997511923146,27.0005192273558,0.154469345431858));
#60359=CARTESIAN_POINT('Ctrl Pts',(-17.4996530582721,27.0005985392793,0.165138575470091));
#60360=CARTESIAN_POINT('Ctrl Pts',(-16.5005649496479,25.9988348222276,0.0342778948658427));
#60361=CARTESIAN_POINT('Ctrl Pts',(-16.5004319098763,26.9990972249887,0.0302562756544078));
#60362=CARTESIAN_POINT('Ctrl Pts',(-17.5005991890068,26.9989642864088,0.0323158604794608));
#60363=CARTESIAN_POINT('Ctrl Pts',(-16.4978390182597,26.0044568076987,-0.388049293380772));
#60364=CARTESIAN_POINT('Ctrl Pts',(-16.4983485327184,27.0034518225239,-0.342280149680354));
#60365=CARTESIAN_POINT('Ctrl Pts',(-17.4977080496968,27.0039616068747,-0.365837717665129));
#60366=CARTESIAN_POINT('Ctrl Pts',(-16.4888223219516,26.0230271690527,-0.669156567504712));
#60367=CARTESIAN_POINT('Ctrl Pts',(-16.4914905865413,27.0177691015244,-0.589955966903106));
#60368=CARTESIAN_POINT('Ctrl Pts',(-17.4881448869157,27.020468594845,-0.630854676420441));
#60369=CARTESIAN_POINT('Ctrl Pts',(-16.4645479010849,26.0733210916423,-1.09014697727432));
#60370=CARTESIAN_POINT('Ctrl Pts',(-16.4728185592198,27.0569442887207,-0.963125072170838));
#60371=CARTESIAN_POINT('Ctrl Pts',(-17.4623992890308,27.0651743036164,-1.02774799205062));
#60372=CARTESIAN_POINT('Ctrl Pts',(-16.4546639962014,26.0938323280556,-1.23036518951515));
#60373=CARTESIAN_POINT('Ctrl Pts',(-16.4652151995949,27.0729175749462,-1.08745697835527));
#60374=CARTESIAN_POINT('Ctrl Pts',(-17.4519163596122,27.0834065139337,-1.15994024599047));
#60375=CARTESIAN_POINT('Ctrl Pts',(-16.4400673858426,26.1242298032478,-1.40549624934421));
#60376=CARTESIAN_POINT('Ctrl Pts',(-16.4539221087833,27.0967120128198,-1.2433380557798));
#60377=CARTESIAN_POINT('Ctrl Pts',(-17.4364351061955,27.1104264917492,-1.32504696908299));
#60378=CARTESIAN_POINT('Ctrl Pts',(-16.4370359610415,26.130547367242,-1.44051537232677));
#60379=CARTESIAN_POINT('Ctrl Pts',(-16.4515773822401,27.1016553378582,-1.27449396665141));
#60380=CARTESIAN_POINT('Ctrl Pts',(-17.433219958682,27.1160421042443,-1.35806163047139));
#60381=CARTESIAN_POINT('Ctrl Pts',(-16.4307488113996,26.1436611143959,-1.51053938021269));
#60382=CARTESIAN_POINT('Ctrl Pts',(-16.4467096966894,27.1119250811992,-1.33683413188026));
#60383=CARTESIAN_POINT('Ctrl Pts',(-17.4265517696646,27.1276987683228,-1.42407753017187));
#60384=CARTESIAN_POINT('Ctrl Pts',(-16.4274906111759,26.1504624708553,-1.54556967700777));
#60385=CARTESIAN_POINT('Ctrl Pts',(-16.4441850672634,27.1172550250431,-1.36803947412004));
#60386=CARTESIAN_POINT('Ctrl Pts',(-17.4230961027206,27.1337444184933,-1.45710272580348));
#60387=CARTESIAN_POINT('Ctrl Pts',(-16.4173982522689,26.1715491252668,-1.65044486531198));
#60388=CARTESIAN_POINT('Ctrl Pts',(-16.43635996178,27.1337879226008,-1.46149208806462));
#60389=CARTESIAN_POINT('Ctrl Pts',(-17.4123920858232,27.1524881114378,-1.55597495718666));
#60390=CARTESIAN_POINT('Ctrl Pts',(-16.4102542800575,26.186500310749,-1.72000002026246));
#60391=CARTESIAN_POINT('Ctrl Pts',(-16.4308099461936,27.1455302764211,-1.52357398570511));
#60392=CARTESIAN_POINT('Ctrl Pts',(-17.4048151454351,27.1657780539216,-1.62154884066042));
#60393=CARTESIAN_POINT('Ctrl Pts',(-16.3725127956242,26.2656547133766,-2.06599962503883));
#60394=CARTESIAN_POINT('Ctrl Pts',(-16.4014953816007,27.2076634406906,-1.83207874075241));
#60395=CARTESIAN_POINT('Ctrl Pts',(-17.3647862987107,27.2361375233113,-1.94774375420961));
#60396=CARTESIAN_POINT('Ctrl Pts',(-16.3358579567688,26.3430155684638,-2.33712916293811));
#60397=CARTESIAN_POINT('Ctrl Pts',(-16.3728357498743,27.2687196259979,-2.07564354115728));
#60398=CARTESIAN_POINT('Ctrl Pts',(-17.3259099538696,27.3049027273893,-2.20335409300917));
#60399=CARTESIAN_POINT('Ctrl Pts',(-16.2509489421038,26.5246876648651,-2.86863842077008));
#60400=CARTESIAN_POINT('Ctrl Pts',(-16.3054421715168,27.4140279801895,-2.55725670467926));
#60401=CARTESIAN_POINT('Ctrl Pts',(-17.2358549388741,27.4663890355697,-2.70444026200191));
#60402=CARTESIAN_POINT('Ctrl Pts',(-16.2026914231958,26.6290018643058,-3.12901661081332));
#60403=CARTESIAN_POINT('Ctrl Pts',(-16.2668736654531,27.4979009908363,-2.79478543759917));
#60404=CARTESIAN_POINT('Ctrl Pts',(-17.1846727213246,27.5591127682956,-2.94991464986886));
#60405=CARTESIAN_POINT('Ctrl Pts',(-16.1224929527533,26.8055233058917,-3.511724585575));
#60406=CARTESIAN_POINT('Ctrl Pts',(-16.2015927972012,27.6422088112504,-3.14811650491222));
#60407=CARTESIAN_POINT('Ctrl Pts',(-17.099613737892,27.7160207163362,-3.31071678104154));
#60408=CARTESIAN_POINT('Ctrl Pts',(-16.0944573592689,26.8677122005455,-3.6379817080266));
#60409=CARTESIAN_POINT('Ctrl Pts',(-16.1787224577041,27.6931119961222,-3.2648130549793));
#60410=CARTESIAN_POINT('Ctrl Pts',(-17.0698790172897,27.7712997338665,-3.42974706475798));
#60411=CARTESIAN_POINT('Ctrl Pts',(-16.0578742587549,26.9496675749635,-3.79416704657873));
#60412=CARTESIAN_POINT('Ctrl Pts',(-16.1486081613594,27.7607465434304,-3.4101345555538));
#60413=CARTESIAN_POINT('Ctrl Pts',(-17.0310787593147,27.844148955511,-3.57699250183713));
#60414=CARTESIAN_POINT('Ctrl Pts',(-16.0504807062728,26.9662697489414,-3.82532226629593));
#60415=CARTESIAN_POINT('Ctrl Pts',(-16.1425271619055,27.7744328577361,-3.43908652601369));
#60416=CARTESIAN_POINT('Ctrl Pts',(-17.0232371126848,27.8589064435178,-3.60636442612413));
#60417=CARTESIAN_POINT('Ctrl Pts',(-16.0355419811776,26.999897690748,-3.88746893406826));
#60418=CARTESIAN_POINT('Ctrl Pts',(-16.1302215604399,27.8021911773562,-3.49689960574396));
#60419=CARTESIAN_POINT('Ctrl Pts',(-17.0073930103687,27.8887979473173,-3.66495387724952));
#60420=CARTESIAN_POINT('Ctrl Pts',(-16.0279925473271,27.0169331053863,-3.91847760489801));
#60421=CARTESIAN_POINT('Ctrl Pts',(-16.1239938076285,27.8162702352096,-3.52577621154247));
#60422=CARTESIAN_POINT('Ctrl Pts',(-16.9993860349865,27.9039405380826,-3.69418764098899));
#60423=CARTESIAN_POINT('Ctrl Pts',(-16.005151309949,27.0686067279126,-4.01113187201297));
#60424=CARTESIAN_POINT('Ctrl Pts',(-16.1051372201557,27.8589989859183,-3.61208369701427));
#60425=CARTESIAN_POINT('Ctrl Pts',(-16.9751604803637,27.9498726471105,-3.78153846518201));
#60426=CARTESIAN_POINT('Ctrl Pts',(-15.9896858552224,27.1037684311926,-4.07232971282369));
#60427=CARTESIAN_POINT('Ctrl Pts',(-16.0923233519077,27.8881659099294,-3.66925480659103));
#60428=CARTESIAN_POINT('Ctrl Pts',(-16.9587577251248,27.9811274943278,-3.8392333993061));
#60429=CARTESIAN_POINT('Ctrl Pts',(-15.9112419315778,27.2830923847797,-4.37551697666845));
#60430=CARTESIAN_POINT('Ctrl Pts',(-16.0274373719239,28.0366047023604,-3.95173322375266));
#60431=CARTESIAN_POINT('Ctrl Pts',(-16.875559624845,28.1405265645112,-4.1250665099463));
#60432=CARTESIAN_POINT('Ctrl Pts',(-15.844918315659,27.4377681716844,-4.60912492170408));
#60433=CARTESIAN_POINT('Ctrl Pts',(-15.9717543805869,28.166270657865,-4.1723242724571));
#60434=CARTESIAN_POINT('Ctrl Pts',(-16.8052163950039,28.2780161525077,-4.34530295645177));
#60435=CARTESIAN_POINT('Ctrl Pts',(-15.7069099448858,27.7688775711428,-5.05949097805553));
#60436=CARTESIAN_POINT('Ctrl Pts',(-15.8543812193166,28.447094636339,-4.60083479731583));
#60437=CARTESIAN_POINT('Ctrl Pts',(-16.6588438813315,28.5723356188943,-4.76989048439904));
#60438=CARTESIAN_POINT('Ctrl Pts',(-15.6352206245408,27.9453128342832,-5.27624649105232));
#60439=CARTESIAN_POINT('Ctrl Pts',(-15.7928000382307,28.5978883814961,-4.80878789175796));
#60440=CARTESIAN_POINT('Ctrl Pts',(-16.5828097529458,28.7291669638434,-4.97423911600232));
#60441=CARTESIAN_POINT('Ctrl Pts',(-15.5249581839362,28.2263776622186,-5.58908746041189));
#60442=CARTESIAN_POINT('Ctrl Pts',(-15.696693052097,28.8413995443161,-5.11191611245));
#60443=CARTESIAN_POINT('Ctrl Pts',(-16.4658647407159,28.9790023663985,-5.26917336342192));
#60444=CARTESIAN_POINT('Ctrl Pts',(-15.4877493740823,28.3228072898136,-5.69131489459601));
#60445=CARTESIAN_POINT('Ctrl Pts',(-15.6642132176884,28.9249883773396,-5.21099932125141));
#60446=CARTESIAN_POINT('Ctrl Pts',(-16.4264008511294,29.0647175909937,-5.36554939547687));
#60447=CARTESIAN_POINT('Ctrl Pts',(-15.431421554897,28.4716312472057,-5.84158285664235));
#60448=CARTESIAN_POINT('Ctrl Pts',(-15.6147184969787,29.0547764285091,-5.3573483822539));
#60449=CARTESIAN_POINT('Ctrl Pts',(-16.3666592249758,29.1970055530476,-5.50721616119523));
#60450=CARTESIAN_POINT('Ctrl Pts',(-15.4125599052749,28.5219362190851,-5.8911597188493));
#60451=CARTESIAN_POINT('Ctrl Pts',(-15.5981338876659,29.098657869549,-5.40563341726845));
#60452=CARTESIAN_POINT('Ctrl Pts',(-16.3466544449051,29.2417210836625,-5.55395529043817));
#60453=CARTESIAN_POINT('Ctrl Pts',(-15.3841604516061,28.5984513320056,-5.9647546987206));
#60454=CARTESIAN_POINT('Ctrl Pts',(-15.5730837024597,29.1655935118162,-5.47748185994016));
#60455=CARTESIAN_POINT('Ctrl Pts',(-16.3165338123512,29.3097345173226,-5.62333776313334));
#60456=CARTESIAN_POINT('Ctrl Pts',(-15.3746761425149,28.6241326720875,-5.98915795629746));
#60457=CARTESIAN_POINT('Ctrl Pts',(-15.5647153050045,29.1880623175047,-5.50130549482725));
#60458=CARTESIAN_POINT('Ctrl Pts',(-16.3064746965653,29.3325623752064,-5.64634420119125));
#60459=CARTESIAN_POINT('Ctrl Pts',(-15.3556755438085,28.6758503150148,-6.03770718948676));
#60460=CARTESIAN_POINT('Ctrl Pts',(-15.547931168814,29.2333546452359,-5.54873830674073));
#60461=CARTESIAN_POINT('Ctrl Pts',(-16.2863225465049,29.3785336133291,-5.69211452210701));
#60462=CARTESIAN_POINT('Ctrl Pts',(-15.3461631123057,28.7018763061624,-6.06184308744346));
#60463=CARTESIAN_POINT('Ctrl Pts',(-15.5395188506324,29.2561687234751,-5.57233816417615));
#60464=CARTESIAN_POINT('Ctrl Pts',(-16.2762336039025,29.4016678276794,-5.71486890398771));
#60465=CARTESIAN_POINT('Ctrl Pts',(-15.2606323097608,28.9371409426806,-6.27738721348527));
#60466=CARTESIAN_POINT('Ctrl Pts',(-15.4642290688267,29.4614132947124,-5.7820464495127));
#60467=CARTESIAN_POINT('Ctrl Pts',(-16.1855191168777,29.610791949213,-5.918075487456));
#60468=CARTESIAN_POINT('Ctrl Pts',(-15.1848342114096,29.1545099575102,-6.45796308382094));
#60469=CARTESIAN_POINT('Ctrl Pts',(-15.3964943458008,29.6534800554759,-5.96008229317087));
#60470=CARTESIAN_POINT('Ctrl Pts',(-16.1051271935059,29.8040088510832,-6.08831536510389));
#60471=CARTESIAN_POINT('Ctrl Pts',(-15.0356595911467,29.6056859311573,-6.79804515130241));
#60472=CARTESIAN_POINT('Ctrl Pts',(-15.2622391988625,30.0548640664217,-6.29665836970821));
#60473=CARTESIAN_POINT('Ctrl Pts',(-15.9469116879931,30.2050541610657,-6.40893145588782));
#60474=CARTESIAN_POINT('Ctrl Pts',(-14.9622788975724,29.8394929473934,-6.95754936214554));
#60475=CARTESIAN_POINT('Ctrl Pts',(-15.1956484255345,30.2641311892708,-6.45556673433959));
#60476=CARTESIAN_POINT('Ctrl Pts',(-15.8690836788716,30.4128826199675,-6.55930579570915));
#60477=CARTESIAN_POINT('Ctrl Pts',(-14.8199953655875,30.3240935251076,-7.25568882321979));
#60478=CARTESIAN_POINT('Ctrl Pts',(-15.0658271140403,30.7002416979089,-6.75341440551023));
#60479=CARTESIAN_POINT('Ctrl Pts',(-15.7181769032676,30.8436386889222,-6.8403800356117));
#60480=CARTESIAN_POINT('Ctrl Pts',(-14.7510880041712,30.5748839284072,-7.39432626488165));
#60481=CARTESIAN_POINT('Ctrl Pts',(-15.0024895581545,30.9271154442475,-6.89273010331883));
#60482=CARTESIAN_POINT('Ctrl Pts',(-15.645093337422,31.0665634920556,-6.9710820001448));
#60483=CARTESIAN_POINT('Ctrl Pts',(-14.6691811405517,30.8997312170887,-7.55423164883944));
#60484=CARTESIAN_POINT('Ctrl Pts',(-14.9266314159884,31.2233129771628,-7.0542966399533));
#60485=CARTESIAN_POINT('Ctrl Pts',(-15.5582224218811,31.3553166373777,-7.12183455119867));
#60486=CARTESIAN_POINT('Ctrl Pts',(-14.653011891398,30.9652703749227,-7.5855411589654));
#60487=CARTESIAN_POINT('Ctrl Pts',(-14.9116910431975,31.2829158941087,-7.08584557342882));
#60488=CARTESIAN_POINT('Ctrl Pts',(-15.5410732180678,31.4135736666364,-7.15135193426238));
#60489=CARTESIAN_POINT('Ctrl Pts',(-14.6291056146706,31.0644531496729,-7.63148523917637));
#60490=CARTESIAN_POINT('Ctrl Pts',(-14.8895640652671,31.3732579073334,-7.13220066227062));
#60491=CARTESIAN_POINT('Ctrl Pts',(-15.5157180762066,31.5017361330234,-7.19466621881002));
#60492=CARTESIAN_POINT('Ctrl Pts',(-14.6211948006132,31.0976597721854,-7.64662987407586));
#60493=CARTESIAN_POINT('Ctrl Pts',(-14.8822417942904,31.4035020137527,-7.14747837210504));
#60494=CARTESIAN_POINT('Ctrl Pts',(-15.507327818792,31.5312531308516,-7.20894398896686));
#60495=CARTESIAN_POINT('Ctrl Pts',(-14.6054941177937,31.1643679687753,-7.67657654190212));
#60496=CARTESIAN_POINT('Ctrl Pts',(-14.867701061467,31.4642882513809,-7.17769919573129));
#60497=CARTESIAN_POINT('Ctrl Pts',(-15.4906755795184,31.5905493055579,-7.23717653788107));
#60498=CARTESIAN_POINT('Ctrl Pts',(-14.5977025585871,31.1978776275757,-7.69138168422876));
#60499=CARTESIAN_POINT('Ctrl Pts',(-14.8604807256331,31.4948381920921,-7.19264621846369));
#60500=CARTESIAN_POINT('Ctrl Pts',(-15.4824118045141,31.6203356689469,-7.2511342477555));
#60501=CARTESIAN_POINT('Ctrl Pts',(-14.5591761411658,31.3656598443161,-7.76432516797013));
#60502=CARTESIAN_POINT('Ctrl Pts',(-14.8248199038901,31.6476138839898,-7.26619003874707));
#60503=CARTESIAN_POINT('Ctrl Pts',(-15.4415504529436,31.7694754172071,-7.31990251526702));
#60504=CARTESIAN_POINT('Ctrl Pts',(-14.5296413627691,31.5010285289678,-7.81939903927279));
#60505=CARTESIAN_POINT('Ctrl Pts',(-14.7973600530408,31.7713364293414,-7.32192638233487));
#60506=CARTESIAN_POINT('Ctrl Pts',(-15.4102256876126,31.8898031368429,-7.37182401004875));
#60507=CARTESIAN_POINT('Ctrl Pts',(-14.4452230147646,31.9105732769504,-7.97492632680715));
#60508=CARTESIAN_POINT('Ctrl Pts',(-14.7189160078809,32.1454427835541,-7.47912726165049));
#60509=CARTESIAN_POINT('Ctrl Pts',(-15.3206910766111,32.2538429128796,-7.51844906238992));
#60510=CARTESIAN_POINT('Ctrl Pts',(-14.394524204208,32.1881803100535,-8.06571177616595));
#60511=CARTESIAN_POINT('Ctrl Pts',(-14.6714240271853,32.4005576020766,-7.57152225977134));
#60512=CARTESIAN_POINT('Ctrl Pts',(-15.266919610253,32.5006047200686,-7.60403803792814));
#60513=CARTESIAN_POINT('Ctrl Pts',(-14.3060495457409,32.7527931145422,-8.22161662427291));
#60514=CARTESIAN_POINT('Ctrl Pts',(-14.5884881552083,32.9202575071458,-7.73013444004218));
#60515=CARTESIAN_POINT('Ctrl Pts',(-15.1730828518141,33.0024827684609,-7.75101903992668));
#60516=CARTESIAN_POINT('Ctrl Pts',(-14.2682728616157,33.0397984670644,-8.2867370209155));
#60517=CARTESIAN_POINT('Ctrl Pts',(-14.552893734404,33.1852802024212,-7.79666355226168));
#60518=CARTESIAN_POINT('Ctrl Pts',(-15.133016671222,33.2575986374368,-7.81241200590781));
#60519=CARTESIAN_POINT('Ctrl Pts',(-14.2226573712228,33.4777284594361,-8.36462327469889));
#60520=CARTESIAN_POINT('Ctrl Pts',(-14.5098903723144,33.5903491926421,-7.87622892641895));
#60521=CARTESIAN_POINT('Ctrl Pts',(-15.0846366059366,33.6468697416979,-7.8858401244665));
#60522=CARTESIAN_POINT('Ctrl Pts',(-14.2092942502116,33.6249441231039,-8.38727953342513));
#60523=CARTESIAN_POINT('Ctrl Pts',(-14.4972860759252,33.7265132279608,-7.8993776669338));
#60524=CARTESIAN_POINT('Ctrl Pts',(-15.0704635986376,33.7777281094489,-7.90719955992493));
#60525=CARTESIAN_POINT('Ctrl Pts',(-14.1921874059586,33.8476922922332,-8.41617145140093));
#60526=CARTESIAN_POINT('Ctrl Pts',(-14.4811437317631,33.9326839034157,-7.92890420892895));
#60527=CARTESIAN_POINT('Ctrl Pts',(-15.0523199760526,33.9757264819735,-7.93443773206372));
#60528=CARTESIAN_POINT('Ctrl Pts',(-14.1869748028688,33.9222626039221,-8.42495286656801));
#60529=CARTESIAN_POINT('Ctrl Pts',(-14.4762244556026,34.0017015413618,-7.93787844712968));
#60530=CARTESIAN_POINT('Ctrl Pts',(-15.0467914575584,34.0420112034973,-7.94271650708992));
#60531=CARTESIAN_POINT('Ctrl Pts',(-14.1799126492618,34.0346090885612,-8.43682988299433));
#60532=CARTESIAN_POINT('Ctrl Pts',(-14.4695579078732,34.105716008113,-7.95001849700854));
#60533=CARTESIAN_POINT('Ctrl Pts',(-15.0393012946864,34.1418747453823,-7.95391369446155));
#60534=CARTESIAN_POINT('Ctrl Pts',(-14.1776847259483,34.0721397627187,-8.44057300476486));
#60535=CARTESIAN_POINT('Ctrl Pts',(-14.4674547435269,34.1404623010022,-7.9538444086756));
#60536=CARTESIAN_POINT('Ctrl Pts',(-15.0369383456894,34.1752353446439,-7.95744256335628));
#60537=CARTESIAN_POINT('Ctrl Pts',(-14.1745348393834,34.1285598388531,-8.44586089729133));
#60538=CARTESIAN_POINT('Ctrl Pts',(-14.4644807945682,34.192704719503,-7.95924986164786));
#60539=CARTESIAN_POINT('Ctrl Pts',(-15.0335975569284,34.2253865234225,-7.96242778198736));
#60540=CARTESIAN_POINT('Ctrl Pts',(-14.173516877044,34.1473872089809,-8.4475690610768));
#60541=CARTESIAN_POINT('Ctrl Pts',(-14.4635196895548,34.2101377324663,-7.96099596612494));
#60542=CARTESIAN_POINT('Ctrl Pts',(-15.0325178998889,34.242121963541,-7.96403817202918));
#60543=CARTESIAN_POINT('Ctrl Pts',(-14.1720382860565,34.1756594493329,-8.45004921553296));
#60544=CARTESIAN_POINT('Ctrl Pts',(-14.4621235724204,34.2363181267017,-7.96353136267135));
#60545=CARTESIAN_POINT('Ctrl Pts',(-15.0309496973357,34.2672528438503,-7.96637636482709));
#60546=CARTESIAN_POINT('Ctrl Pts',(-14.171553481119,34.1850887269927,-8.45086225174429));
#60547=CARTESIAN_POINT('Ctrl Pts',(-14.4616658100524,34.2450496654721,-7.96436249848284));
#60548=CARTESIAN_POINT('Ctrl Pts',(-15.0304355102747,34.2756344239947,-7.96714286358229));
#60549=CARTESIAN_POINT('Ctrl Pts',(-14.1706000477243,34.2039577059635,-8.45246089334986));
#60550=CARTESIAN_POINT('Ctrl Pts',(-14.4607655369268,34.2625227778338,-7.96599675441144));
#60551=CARTESIAN_POINT('Ctrl Pts',(-15.029424293044,34.2924068497441,-7.96865000047954));
#60552=CARTESIAN_POINT('Ctrl Pts',(-14.1701308662489,34.2134087629436,-8.45324742565082));
#60553=CARTESIAN_POINT('Ctrl Pts',(-14.4603225019436,34.2712748866038,-7.96680082574036));
#60554=CARTESIAN_POINT('Ctrl Pts',(-15.028926676316,34.3008077891872,-7.96939151350123));
#60555=CARTESIAN_POINT('Ctrl Pts',(-14.1696709084508,34.2228423347593,-8.45401835497186));
#60556=CARTESIAN_POINT('Ctrl Pts',(-14.4598881528388,34.2800112558736,-7.96758898230353));
#60557=CARTESIAN_POINT('Ctrl Pts',(-15.0284388422964,34.3091931864527,-7.97011831445158));
#60558=CARTESIAN_POINT('Ctrl Pts',(-6.,40.2323075626015,-16.7705098312484));
#60559=CARTESIAN_POINT('Ctrl Pts',(-6.,40.2323075626015,-15.4288690447485));
#60560=CARTESIAN_POINT('Ctrl Pts',(-4.71428571428571,40.2323075626015,-15.8121949837485));
#60561=CARTESIAN_POINT('Ctrl Pts',(-6.,40.2152831433091,-16.7705098300439));
#60562=CARTESIAN_POINT('Ctrl Pts',(-5.99999999918455,40.2289031540789,-15.4288690446538));
#60563=CARTESIAN_POINT('Ctrl Pts',(-4.71428571810276,40.1812343046596,-15.8121949826105));
#60564=CARTESIAN_POINT('Ctrl Pts',(-6.00086709959613,40.1984135664914,-16.7697348999033));
#60565=CARTESIAN_POINT('Ctrl Pts',(-5.99947691569071,40.2255290821746,-15.4288072509424));
#60566=CARTESIAN_POINT('Ctrl Pts',(-4.71673836819782,40.1306255743571,-15.8114643341001));
#60567=CARTESIAN_POINT('Ctrl Pts',(-6.00426966178499,40.1649734181343,-16.7666864482411));
#60568=CARTESIAN_POINT('Ctrl Pts',(-5.99746228399819,40.218435826368,-15.4285622514261));
#60569=CARTESIAN_POINT('Ctrl Pts',(-4.72636275685162,40.0303051291139,-15.8085900798646));
#60570=CARTESIAN_POINT('Ctrl Pts',(-6.00680532946631,40.1484027206558,-16.7644127338286));
#60571=CARTESIAN_POINT('Ctrl Pts',(-5.99597239391959,40.2147209114066,-15.4283793290426));
#60572=CARTESIAN_POINT('Ctrl Pts',(-4.7335350744668,39.980593036709,-15.8064462917098));
#60573=CARTESIAN_POINT('Ctrl Pts',(-6.01353255271329,40.1155581374418,-16.7583557139617));
#60574=CARTESIAN_POINT('Ctrl Pts',(-5.99214798696173,40.2065622671074,-15.4278851619237));
#60575=CARTESIAN_POINT('Ctrl Pts',(-4.75256350655548,39.8820592871776,-15.8007353876353));
#60576=CARTESIAN_POINT('Ctrl Pts',(-6.01772404886921,40.0992842400478,-16.7545725300023));
#60577=CARTESIAN_POINT('Ctrl Pts',(-5.98981636127134,40.202124845771,-15.4275745721604));
#60578=CARTESIAN_POINT('Ctrl Pts',(-4.76441945116622,39.8332375945207,-15.7971683851509));
#60579=CARTESIAN_POINT('Ctrl Pts',(-6.0240219807572,40.0791319892091,-16.74885556262));
#60580=CARTESIAN_POINT('Ctrl Pts',(-5.98648250852101,40.1958724239871,-15.4270937726593));
#60581=CARTESIAN_POINT('Ctrl Pts',(-4.78223360305063,39.7727808425291,-15.7917781019688));
#60582=CARTESIAN_POINT('Ctrl Pts',(-6.02533572392216,40.0751078557388,-16.7476616129027));
#60583=CARTESIAN_POINT('Ctrl Pts',(-5.98579543217186,40.1945875299876,-15.4269930200015));
#60584=CARTESIAN_POINT('Ctrl Pts',(-4.78594961957438,39.7607084421942,-15.7906523778123));
#60585=CARTESIAN_POINT('Ctrl Pts',(-6.02806562891379,40.0670929379168,-16.7451772260115));
#60586=CARTESIAN_POINT('Ctrl Pts',(-5.98438622375446,40.191946424886,-15.4267821748928));
#60587=CARTESIAN_POINT('Ctrl Pts',(-4.79367134987588,39.7366636883665,-15.7883099560211));
#60588=CARTESIAN_POINT('Ctrl Pts',(-6.0294779907155,40.0631130239638,-16.7438902481684));
#60589=CARTESIAN_POINT('Ctrl Pts',(-5.98366611306037,40.1905939935738,-15.4266723903639));
#60590=CARTESIAN_POINT('Ctrl Pts',(-4.79766631700306,39.7247239468563,-15.78709651963));
#60591=CARTESIAN_POINT('Ctrl Pts',(-6.03385527087601,40.051254796774,-16.739895758248));
#60592=CARTESIAN_POINT('Ctrl Pts',(-5.98146696546189,40.1864358470219,-15.4263296304894));
#60593=CARTESIAN_POINT('Ctrl Pts',(-4.81004776537665,39.6891492647827,-15.7833302864913));
#60594=CARTESIAN_POINT('Ctrl Pts',(-6.03696028948911,40.0434579430007,-16.7370547926887));
#60595=CARTESIAN_POINT('Ctrl Pts',(-5.97994756331896,40.1835265738621,-15.426083083921));
#60596=CARTESIAN_POINT('Ctrl Pts',(-4.81883053366853,39.6657587040667,-15.7806516615182));
#60597=CARTESIAN_POINT('Ctrl Pts',(-6.04682316560899,40.0203864307978,-16.7280004451824));
#60598=CARTESIAN_POINT('Ctrl Pts',(-5.97529225782466,40.1743463310241,-15.4252854635617));
#60599=CARTESIAN_POINT('Ctrl Pts',(-4.84672838163821,39.5965441666547,-15.7721147057772));
#60600=CARTESIAN_POINT('Ctrl Pts',(-6.05412752167962,40.0054300386619,-16.7212571411063));
#60601=CARTESIAN_POINT('Ctrl Pts',(-5.97205156506919,40.1676130008118,-15.4246764580379));
#60602=CARTESIAN_POINT('Ctrl Pts',(-4.86738927571349,39.551674990914,-15.7657567326582));
#60603=CARTESIAN_POINT('Ctrl Pts',(-6.07016106549893,39.9763502064277,-16.7063311041315));
#60604=CARTESIAN_POINT('Ctrl Pts',(-5.9656350667376,40.1526685017272,-15.4232639946225));
#60605=CARTESIAN_POINT('Ctrl Pts',(-4.91274129944868,39.4644354939485,-15.7516836128517));
#60606=CARTESIAN_POINT('Ctrl Pts',(-6.07889031425637,39.9622267963988,-16.698148412995));
#60607=CARTESIAN_POINT('Ctrl Pts',(-5.96246129227807,40.1444721129303,-15.422462446856));
#60608=CARTESIAN_POINT('Ctrl Pts',(-4.93743260243233,39.4220652635496,-15.7439685032292));
#60609=CARTESIAN_POINT('Ctrl Pts',(-6.09069779316276,39.9450985529772,-16.6869735595439));
#60610=CARTESIAN_POINT('Ctrl Pts',(-5.95877416318781,40.1331449703773,-15.4212977072095));
#60611=CARTESIAN_POINT('Ctrl Pts',(-4.97083090084792,39.3706805338393,-15.7334322133972));
#60612=CARTESIAN_POINT('Ctrl Pts',(-6.09310418619124,39.9416992657338,-16.6846911400641));
#60613=CARTESIAN_POINT('Ctrl Pts',(-5.9580529547782,40.1308323519191,-15.4210572678978));
#60614=CARTESIAN_POINT('Ctrl Pts',(-4.97763755498991,39.3604826718443,-15.7312802176574));
#60615=CARTESIAN_POINT('Ctrl Pts',(-6.09800731088457,39.934953794505,-16.680029715004));
#60616=CARTESIAN_POINT('Ctrl Pts',(-5.95664664771447,40.1260992628088,-15.420559060673));
#60617=CARTESIAN_POINT('Ctrl Pts',(-4.99150639388168,39.3402462584659,-15.7268851599783));
#60618=CARTESIAN_POINT('Ctrl Pts',(-6.10050726882805,39.931603434497,-16.6776476264958));
#60619=CARTESIAN_POINT('Ctrl Pts',(-5.95596070720442,40.1236759648656,-15.4203009955482));
#60620=CARTESIAN_POINT('Ctrl Pts',(-4.99857770366056,39.3301951786403,-15.7246391906029));
#60621=CARTESIAN_POINT('Ctrl Pts',(-6.10811946799149,39.9216641845842,-16.670376806369));
#60622=CARTESIAN_POINT('Ctrl Pts',(-5.95397565819811,40.1162694017168,-15.419501917334));
#60623=CARTESIAN_POINT('Ctrl Pts',(-5.0201093515106,39.3003774278449,-15.7177838461912));
#60624=CARTESIAN_POINT('Ctrl Pts',(-6.11333262437216,39.915200818976,-16.6653744832296));
#60625=CARTESIAN_POINT('Ctrl Pts',(-5.95274853351578,40.1111506689315,-15.4189363070628));
#60626=CARTESIAN_POINT('Ctrl Pts',(-5.03485513807882,39.2809873322929,-15.7130673697086));
#60627=CARTESIAN_POINT('Ctrl Pts',(-6.1293748326009,39.8962861790546,-16.6499024080798));
#60628=CARTESIAN_POINT('Ctrl Pts',(-5.94943970565223,40.0952810454962,-15.4171310107049));
#60629=CARTESIAN_POINT('Ctrl Pts',(-5.08023166821929,39.2242434108254,-15.6984794137196));
#60630=CARTESIAN_POINT('Ctrl Pts',(-6.1406056663782,39.884309238974,-16.6389685998647));
#60631=CARTESIAN_POINT('Ctrl Pts',(-5.94771464892963,40.0839766925516,-15.4157800254322));
#60632=CARTESIAN_POINT('Ctrl Pts',(-5.11199888523177,39.1883125922345,-15.6881703937412));
#60633=CARTESIAN_POINT('Ctrl Pts',(-6.16409905708717,39.8615816843069,-16.6158372464421));
#60634=CARTESIAN_POINT('Ctrl Pts',(-5.94564861891527,40.0599452805169,-15.4126949205069));
#60635=CARTESIAN_POINT('Ctrl Pts',(-5.17845161828455,39.1201299272022,-15.6663608327766));
#60636=CARTESIAN_POINT('Ctrl Pts',(-6.17636172059827,39.8508311824304,-16.6036396930356));
#60637=CARTESIAN_POINT('Ctrl Pts',(-5.94529765421637,40.0472399899623,-15.4109653218148));
#60638=CARTESIAN_POINT('Ctrl Pts',(-5.21313743796322,39.0878784218881,-15.6548602815568));
#60639=CARTESIAN_POINT('Ctrl Pts',(-6.19552162464795,39.8356220321449,-16.5843510979584));
#60640=CARTESIAN_POINT('Ctrl Pts',(-5.94612875976558,40.0271363620363,-15.4079956032292));
#60641=CARTESIAN_POINT('Ctrl Pts',(-5.26733259558317,39.0422509713317,-15.6366738925849));
#60642=CARTESIAN_POINT('Ctrl Pts',(-6.20203613099305,39.8307053430792,-16.5777559291836));
#60643=CARTESIAN_POINT('Ctrl Pts',(-5.94662867798683,40.0202869469601,-15.4069471500247));
#60644=CARTESIAN_POINT('Ctrl Pts',(-5.28575934167097,39.0275009037357,-15.6304555901406));
#60645=CARTESIAN_POINT('Ctrl Pts',(-6.21200068125232,39.8235618043476,-16.567606697845));
#60646=CARTESIAN_POINT('Ctrl Pts',(-5.94775936498885,40.0097653187781,-15.4052685020573));
#60647=CARTESIAN_POINT('Ctrl Pts',(-5.31394478425411,39.0060702879891,-15.6208863152272));
#60648=CARTESIAN_POINT('Ctrl Pts',(-6.21535764108576,39.8212169930998,-16.5641774763452));
#60649=CARTESIAN_POINT('Ctrl Pts',(-5.9481991858846,40.0062198151304,-15.4046917890623));
#60650=CARTESIAN_POINT('Ctrl Pts',(-5.32344018506321,38.9990358545671,-15.6176530490547));
#60651=CARTESIAN_POINT('Ctrl Pts',(-6.22212086912811,39.8166154680804,-16.5572476494714));
#60652=CARTESIAN_POINT('Ctrl Pts',(-5.94920983527497,39.9990692704025,-15.4035042743602));
#60653=CARTESIAN_POINT('Ctrl Pts',(-5.34257045811315,38.9852312785673,-15.6111192124296));
#60654=CARTESIAN_POINT('Ctrl Pts',(-6.22552135620163,39.8143625551259,-16.5537529884858));
#60655=CARTESIAN_POINT('Ctrl Pts',(-5.94977935255954,39.9954706760488,-15.4028946209305));
#60656=CARTESIAN_POINT('Ctrl Pts',(-5.35218897920305,38.9784725405973,-15.6078242462156));
#60657=CARTESIAN_POINT('Ctrl Pts',(-6.24261647292014,39.8033336673682,-16.5361308383412));
#60658=CARTESIAN_POINT('Ctrl Pts',(-5.95294841354305,39.9774321071524,-15.3997736035282));
#60659=CARTESIAN_POINT('Ctrl Pts',(-5.4005437367575,38.9453858752107,-15.5912090764345));
#60660=CARTESIAN_POINT('Ctrl Pts',(-6.25658842504356,39.7952630018719,-16.5215575392438));
#60661=CARTESIAN_POINT('Ctrl Pts',(-5.95654259008027,39.9626139216758,-15.3970056111323));
#60662=CARTESIAN_POINT('Ctrl Pts',(-5.44006440260921,38.9211738813271,-15.5774685367124));
#60663=CARTESIAN_POINT('Ctrl Pts',(-6.28509305730017,39.7805641079001,-16.4914450749466));
#60664=CARTESIAN_POINT('Ctrl Pts',(-5.96611579674779,39.9325466076702,-15.3908337573467));
#60665=CARTESIAN_POINT('Ctrl Pts',(-5.52069179030617,38.8770771975832,-15.5490767852386));
#60666=CARTESIAN_POINT('Ctrl Pts',(-6.29962582233355,39.7739360664052,-16.4759058887031));
#60667=CARTESIAN_POINT('Ctrl Pts',(-5.97206780921745,39.917312384644,-15.3874384220071));
#60668=CARTESIAN_POINT('Ctrl Pts',(-5.56179875453699,38.8571930741266,-15.5344255519103));
#60669=CARTESIAN_POINT('Ctrl Pts',(-6.32923798954882,39.7621006130703,-16.4438289832851));
#60670=CARTESIAN_POINT('Ctrl Pts',(-5.98657812285022,39.8867276348292,-15.3799070345543));
#60671=CARTESIAN_POINT('Ctrl Pts',(-5.64555888478752,38.8216867138941,-15.5041816131072));
#60672=CARTESIAN_POINT('Ctrl Pts',(-6.34431740281587,39.7568932093963,-16.427291325653));
#60673=CARTESIAN_POINT('Ctrl Pts',(-5.99510387590282,39.8713890796003,-15.3757815092243));
#60674=CARTESIAN_POINT('Ctrl Pts',(-5.68821208193698,38.8060645022573,-15.4885889638827));
#60675=CARTESIAN_POINT('Ctrl Pts',(-6.36350899238667,39.7512813707633,-16.4059633038224));
#60676=CARTESIAN_POINT('Ctrl Pts',(-6.00757171375912,39.8522872563196,-15.3700673381977));
#60677=CARTESIAN_POINT('Ctrl Pts',(-5.74249686425784,38.7892289872689,-15.4684796865372));
#60678=CARTESIAN_POINT('Ctrl Pts',(-6.36736640469525,39.7502035609108,-16.4016626515698));
#60679=CARTESIAN_POINT('Ctrl Pts',(-6.01014306585411,39.8484887840959,-15.368902314736));
#60680=CARTESIAN_POINT('Ctrl Pts',(-5.75340783051444,38.7859955579257,-15.464424785742));
#60681=CARTESIAN_POINT('Ctrl Pts',(-6.37508178304079,39.7481470746211,-16.393032726381));
#60682=CARTESIAN_POINT('Ctrl Pts',(-6.01543918049613,39.8409465314235,-15.3665281828108));
#60683=CARTESIAN_POINT('Ctrl Pts',(-5.77523132908179,38.7798260982638,-15.456287999183));
#60684=CARTESIAN_POINT('Ctrl Pts',(-6.37894373953493,39.7471671729223,-16.3886990350584));
#60685=CARTESIAN_POINT('Ctrl Pts',(-6.01816590364594,39.8371987683928,-15.3653180873047));
#60686=CARTESIAN_POINT('Ctrl Pts',(-5.78615514903906,38.7768863939058,-15.4522019473171));
#60687=CARTESIAN_POINT('Ctrl Pts',(-6.39054216941777,39.7443708383147,-16.3756416702532));
#60688=CARTESIAN_POINT('Ctrl Pts',(-6.02657153999075,39.8260491189418,-15.3616221037249));
#60689=CARTESIAN_POINT('Ctrl Pts',(-5.81896213621546,38.7684973890572,-15.4398907177147));
#60690=CARTESIAN_POINT('Ctrl Pts',(-6.39829119296333,39.7426976933212,-16.3668617166323));
#60691=CARTESIAN_POINT('Ctrl Pts',(-6.0324962949229,39.8187094218724,-15.3590612008815));
#60692=CARTESIAN_POINT('Ctrl Pts',(-5.84088080302002,38.7634779552291,-15.4316124756347));
#60693=CARTESIAN_POINT('Ctrl Pts',(-6.42158691874072,39.7382413617845,-16.3402955022825));
#60694=CARTESIAN_POINT('Ctrl Pts',(-6.05116583633343,39.797127595989,-15.351106610322));
#60695=CARTESIAN_POINT('Ctrl Pts',(-5.90677442716201,38.750108959213,-15.4065643308179));
#60696=CARTESIAN_POINT('Ctrl Pts',(-6.43718213048319,39.7360200677615,-16.3222830574036));
#60697=CARTESIAN_POINT('Ctrl Pts',(-6.06488620812391,39.7831957544441,-15.3454045239078));
#60698=CARTESIAN_POINT('Ctrl Pts',(-5.95088659762375,38.743445078172,-15.3895811683148));
#60699=CARTESIAN_POINT('Ctrl Pts',(-6.46849740752571,39.7330531695987,-16.2856443359368));
#60700=CARTESIAN_POINT('Ctrl Pts',(-6.09483924332511,39.7566876277051,-15.333160094272));
#60701=CARTESIAN_POINT('Ctrl Pts',(-6.03946409560143,38.7345443835025,-15.3550360882633));
#60702=CARTESIAN_POINT('Ctrl Pts',(-6.484217551678,39.7323075626015,-16.2670179887174));
#60703=CARTESIAN_POINT('Ctrl Pts',(-6.11103676931995,39.7441010190891,-15.3266299702959));
#60704=CARTESIAN_POINT('Ctrl Pts',(-6.08392963895787,38.7323075641139,-15.3374741067549));
#60705=CARTESIAN_POINT('Ctrl Pts',(-6.5,39.7323075626015,-16.2480768092719));
#60706=CARTESIAN_POINT('Ctrl Pts',(-6.12857142857143,39.7323075626015,-15.3196152773135));
#60707=CARTESIAN_POINT('Ctrl Pts',(-6.12857142857143,38.7323075626015,-15.3196152773135));
#60708=CARTESIAN_POINT('Origin',(-37.,45.4641016151378,-17.5));
#60709=CARTESIAN_POINT('Origin',(-45.2221315177632,44.4440520797063,-25.3383443274765));
#60710=CARTESIAN_POINT('Origin',(-11.,51.,0.));
#60711=CARTESIAN_POINT('Origin',(-6.5,54.4282032302755,-24.));
#60712=CARTESIAN_POINT('',(-6.5,52.3811718911434,-24.5));
#60713=CARTESIAN_POINT('',(-6.5,54.4282032302755,-24.5));
#60714=CARTESIAN_POINT('Ctrl Pts',(-6.50000000000002,52.3811718911434,-24.5));
#60715=CARTESIAN_POINT('Ctrl Pts',(-6.45484712541262,52.3374123315343,-24.5));
#60716=CARTESIAN_POINT('Ctrl Pts',(-6.4063809595238,52.2931062029975,-24.4937365926974));
#60717=CARTESIAN_POINT('Ctrl Pts',(-6.29450947020769,52.1982971503326,-24.4606141098908));
#60718=CARTESIAN_POINT('Ctrl Pts',(-6.23114032575744,52.1503834195514,-24.4274665133501));
#60719=CARTESIAN_POINT('Ctrl Pts',(-6.13253307624096,52.0829899601412,-24.3440537454782));
#60720=CARTESIAN_POINT('Ctrl Pts',(-6.08952339015813,52.0568515986448,-24.2932685081818));
#60721=CARTESIAN_POINT('Ctrl Pts',(-6.0267513370081,52.0210538996719,-24.1747375197227));
#60722=CARTESIAN_POINT('Ctrl Pts',(-6.00719188754555,52.0110551102428,-24.1069871550009));
#60723=CARTESIAN_POINT('Ctrl Pts',(-6.00059405760162,52.0049022588122,-24.0279494392554));
#60724=CARTESIAN_POINT('Ctrl Pts',(-6.,52.0040117065365,-24.0140517567783));
#60725=CARTESIAN_POINT('Ctrl Pts',(-6.,52.0032753870454,-24.));
#60726=CARTESIAN_POINT('Origin',(-27.1034840901754,53.,1.07291666666666));
#60727=CARTESIAN_POINT('Origin',(-27.1034840901754,53.,1.07291666666666));
#60728=CARTESIAN_POINT('Origin',(-5.47112164030075,53.000000000001,-24.5000000000001));
#60729=CARTESIAN_POINT('Origin',(-3.43565291283912,53.,26.90625));
#60730=CARTESIAN_POINT('Origin',(-3.43565291283912,53.,26.90625));
#60731=CARTESIAN_POINT('Origin',(6.61363325216158E-15,53.,24.));
#60732=CARTESIAN_POINT('Origin',(3.43565291283914,53.,26.90625));
#60733=CARTESIAN_POINT('Origin',(3.43565291283914,53.,26.90625));
#60734=CARTESIAN_POINT('Origin',(15.2695685015073,53.,12.9166666666666));
#60735=CARTESIAN_POINT('Origin',(6.61287431064084E-15,53.,0.));
#60736=CARTESIAN_POINT('Origin',(15.2695685015073,53.,-12.9166666666667));
#60737=CARTESIAN_POINT('Origin',(27.1034840901754,53.,1.07291666666666));
#60738=CARTESIAN_POINT('Ctrl Pts',(15.8769086599362,26.2075694296671,4.49152217004988));
#60739=CARTESIAN_POINT('Ctrl Pts',(15.9873632533133,26.9858847285589,4.10107844589208));
#60740=CARTESIAN_POINT('Ctrl Pts',(16.8391456316905,27.0868129846264,4.28736180648697));
#60741=CARTESIAN_POINT('Ctrl Pts',(15.8582352049183,26.2455000465674,4.55753024670209));
#60742=CARTESIAN_POINT('Ctrl Pts',(15.9714605842203,27.0177778865802,4.16347898353059));
#60743=CARTESIAN_POINT('Ctrl Pts',(16.8193404549634,27.1209505355579,4.35036951074904));
#60744=CARTESIAN_POINT('Ctrl Pts',(15.8392331472462,26.2842765272885,4.62312840029494));
#60745=CARTESIAN_POINT('Ctrl Pts',(15.9552081857089,27.0505108449272,4.2257203082126));
#60746=CARTESIAN_POINT('Ctrl Pts',(16.7991867589916,27.155849366436,4.41298592969122));
#60747=CARTESIAN_POINT('Ctrl Pts',(15.810254271091,26.3437152476807,4.72091258212513));
#60748=CARTESIAN_POINT('Ctrl Pts',(15.9303287054477,27.1008592013043,4.31876680254219));
#60749=CARTESIAN_POINT('Ctrl Pts',(16.7684515907413,27.2093442101895,4.50632537208709));
#60750=CARTESIAN_POINT('Ctrl Pts',(15.8005153477853,26.3637405141118,4.75340512204032));
#60751=CARTESIAN_POINT('Ctrl Pts',(15.9219634459718,27.1178269445236,4.34968902000699));
#60752=CARTESIAN_POINT('Ctrl Pts',(16.7581224307191,27.2273669484456,4.53734097703345));
#60753=CARTESIAN_POINT('Ctrl Pts',(15.7808817629062,26.4042169640041,4.81818599630767));
#60754=CARTESIAN_POINT('Ctrl Pts',(15.9050753095569,27.1521659834681,4.4114003037423));
#60755=CARTESIAN_POINT('Ctrl Pts',(16.7372989339143,27.263795750215,4.59917726355392));
#60756=CARTESIAN_POINT('Ctrl Pts',(15.7709841530912,26.4246742589405,4.85048383592628));
#60757=CARTESIAN_POINT('Ctrl Pts',(15.8965503240519,27.1695414485629,4.44219808335061));
#60758=CARTESIAN_POINT('Ctrl Pts',(16.72680147,27.2822073140643,4.63000701827412));
#60759=CARTESIAN_POINT('Ctrl Pts',(15.7211457888462,26.527963020949,5.01135996312586));
#60760=CARTESIAN_POINT('Ctrl Pts',(15.8536759108252,27.2571485161243,4.59535151664664));
#60761=CARTESIAN_POINT('Ctrl Pts',(16.6739426048502,27.3751671919753,4.78357058767493));
#60762=CARTESIAN_POINT('Ctrl Pts',(15.6803478341989,26.6133981550309,5.13748080940201));
#60763=CARTESIAN_POINT('Ctrl Pts',(15.8183072530954,27.3301139516917,4.71622063716264));
#60764=CARTESIAN_POINT('Ctrl Pts',(16.6306720509859,27.452058805977,4.90395866359305));
#60765=CARTESIAN_POINT('Ctrl Pts',(15.5555633441787,26.8779283667801,5.50840431704435));
#60766=CARTESIAN_POINT('Ctrl Pts',(15.7099001145759,27.5563845907162,5.07174318477029));
#60767=CARTESIAN_POINT('Ctrl Pts',(16.4983248790498,27.6901359766523,5.25802199793798));
#60768=CARTESIAN_POINT('Ctrl Pts',(15.4691874138206,27.065223688674,5.74578785429625));
#60769=CARTESIAN_POINT('Ctrl Pts',(15.633882786453,27.7183716325533,5.30193650363448));
#60770=CARTESIAN_POINT('Ctrl Pts',(16.4067140519913,27.8587017525446,5.48461536708638));
#60771=CARTESIAN_POINT('Ctrl Pts',(15.2920609491932,27.4613270309352,6.20183111975059));
#60772=CARTESIAN_POINT('Ctrl Pts',(15.4763461124972,28.0643447982136,5.74688779723174));
#60773=CARTESIAN_POINT('Ctrl Pts',(16.2188526682064,28.2151947332129,5.91992938097804));
#60774=CARTESIAN_POINT('Ctrl Pts',(15.201305139851,27.6701352530085,6.42048862811649));
#60775=CARTESIAN_POINT('Ctrl Pts',(15.394911415866,28.2479943353604,5.96182339691564));
#60776=CARTESIAN_POINT('Ctrl Pts',(16.1225965145591,28.4031221189222,6.12864790645227));
#60777=CARTESIAN_POINT('Ctrl Pts',(15.063397310651,27.9997968012076,6.73477167440303));
#60778=CARTESIAN_POINT('Ctrl Pts',(15.2696355732375,28.541402061921,6.27340007303451));
#60779=CARTESIAN_POINT('Ctrl Pts',(15.9763306474089,28.6998174915388,6.42864535457189));
#60780=CARTESIAN_POINT('Ctrl Pts',(15.0171329992815,28.112431629095,6.83724424346893));
#60781=CARTESIAN_POINT('Ctrl Pts',(15.2275847859334,28.6416330504077,6.37495337745684));
#60782=CARTESIAN_POINT('Ctrl Pts',(15.9272624420383,28.8011888294802,6.52646007755072));
#60783=CARTESIAN_POINT('Ctrl Pts',(14.9474944335502,28.2856028304495,6.98752160996693));
#60784=CARTESIAN_POINT('Ctrl Pts',(15.1639331114985,28.7965496531306,6.52450489168869));
#60785=CARTESIAN_POINT('Ctrl Pts',(15.8534033631529,28.957042899895,6.66990665258495));
#60786=CARTESIAN_POINT('Ctrl Pts',(14.9242413338947,28.3440301462527,7.03704185847933));
#60787=CARTESIAN_POINT('Ctrl Pts',(15.1426746889094,28.8488125585796,6.57377108052547));
#60788=CARTESIAN_POINT('Ctrl Pts',(15.8287409864956,29.0096274805124,6.71717597981947));
#60789=CARTESIAN_POINT('Ctrl Pts',(14.889327508177,28.4327426653544,7.11046135857809));
#60790=CARTESIAN_POINT('Ctrl Pts',(15.1106696590438,28.9283638930351,6.64696562658708));
#60791=CARTESIAN_POINT('Ctrl Pts',(15.7917111742834,29.0894687421935,6.78725822899178));
#60792=CARTESIAN_POINT('Ctrl Pts',(14.8776905601943,28.4624753483755,7.13477680771444));
#60793=CARTESIAN_POINT('Ctrl Pts',(15.1000012851191,28.9550247920885,6.67120233635647));
#60794=CARTESIAN_POINT('Ctrl Pts',(15.7793689575767,29.1162281550713,6.81046843005605));
#60795=CARTESIAN_POINT('Ctrl Pts',(14.8544631761811,28.522162195526,7.183010528203));
#60796=CARTESIAN_POINT('Ctrl Pts',(15.0786880317589,29.0085874834985,6.71930924825527));
#60797=CARTESIAN_POINT('Ctrl Pts',(15.7547338552975,29.1699463138537,6.85650970805247));
#60798=CARTESIAN_POINT('Ctrl Pts',(14.8428668837395,28.5521312162157,7.20694113675592));
#60799=CARTESIAN_POINT('Ctrl Pts',(15.0680376418045,29.0355024561561,6.74319259210144));
#60800=CARTESIAN_POINT('Ctrl Pts',(15.7424347580747,29.1969184306039,6.87935256133954));
#60801=CARTESIAN_POINT('Ctrl Pts',(14.7386765131152,28.8229821364781,7.42065217988111));
#60802=CARTESIAN_POINT('Ctrl Pts',(14.9728123593002,29.2775407023946,6.95538233905929));
#60803=CARTESIAN_POINT('Ctrl Pts',(15.6319298287787,29.4406842412807,7.08334946253237));
#60804=CARTESIAN_POINT('Ctrl Pts',(14.6473111890801,29.071748056285,7.59881636225689));
#60805=CARTESIAN_POINT('Ctrl Pts',(14.8881630949714,29.5024636848611,7.13446033202847));
#60806=CARTESIAN_POINT('Ctrl Pts',(15.535027218385,29.6645735542109,7.25341527124138));
#60807=CARTESIAN_POINT('Ctrl Pts',(14.4693728540855,29.5855591847265,7.93240092198966));
#60808=CARTESIAN_POINT('Ctrl Pts',(14.7224664869594,29.9694548692142,7.47059284153777));
#60809=CARTESIAN_POINT('Ctrl Pts',(15.3463047553347,30.1270035400911,7.57183689452032));
#60810=CARTESIAN_POINT('Ctrl Pts',(14.3827951407555,29.8506033440453,8.08782034517746));
#60811=CARTESIAN_POINT('Ctrl Pts',(14.6412849462596,30.2115686379399,7.62808869657179));
#60812=CARTESIAN_POINT('Ctrl Pts',(15.254479912919,30.3655432686509,7.72019179758978));
#60813=CARTESIAN_POINT('Ctrl Pts',(14.2583927643846,30.261019135023,8.30392342666024));
#60814=CARTESIAN_POINT('Ctrl Pts',(14.5238989245498,30.5889923546909,7.84801190409701));
#60815=CARTESIAN_POINT('Ctrl Pts',(15.1225380068262,30.7349174586429,7.92647201231362));
#60816=CARTESIAN_POINT('Ctrl Pts',(14.2178380489227,30.3999707062553,8.37311388575839));
#60817=CARTESIAN_POINT('Ctrl Pts',(14.4856296693811,30.7167001609698,7.9183828465517));
#60818=CARTESIAN_POINT('Ctrl Pts',(15.0795254320222,30.8599738652951,7.99251745021501));
#60819=CARTESIAN_POINT('Ctrl Pts',(14.1388980403649,30.6823345265142,8.50573436767722));
#60820=CARTESIAN_POINT('Ctrl Pts',(14.4110045335691,30.9766778340591,8.0534028711467));
#60821=CARTESIAN_POINT('Ctrl Pts',(14.9958011856818,31.1141012882541,8.1191097289101));
#60822=CARTESIAN_POINT('Ctrl Pts',(14.1005125570259,30.825746585496,8.56916458200204));
#60823=CARTESIAN_POINT('Ctrl Pts',(14.3746261627414,31.1089703880548,8.11810372149017));
#60824=CARTESIAN_POINT('Ctrl Pts',(14.9550893113803,31.2431721338399,8.17965675141353));
#60825=CARTESIAN_POINT('Ctrl Pts',(14.0448396969175,31.0443707833594,8.65989242941114));
#60826=CARTESIAN_POINT('Ctrl Pts',(14.3217244652542,31.3111850624393,8.21083048026107));
#60827=CARTESIAN_POINT('Ctrl Pts',(14.896042341965,31.4399339005038,8.26626060646187));
#60828=CARTESIAN_POINT('Ctrl Pts',(14.0265998696782,31.1178302470309,8.68939833580717));
#60829=CARTESIAN_POINT('Ctrl Pts',(14.3043940626367,31.3791100903781,8.24097506569154));
#60830=CARTESIAN_POINT('Ctrl Pts',(14.8766970715514,31.5060474140306,8.29442533516559));
#60831=CARTESIAN_POINT('Ctrl Pts',(13.9997539373385,31.2289203061233,8.73253551550609));
#60832=CARTESIAN_POINT('Ctrl Pts',(14.2788527797159,31.4819620626231,8.28509109464653));
#60833=CARTESIAN_POINT('Ctrl Pts',(14.8482241146408,31.6060284614212,8.3356017343517));
#60834=CARTESIAN_POINT('Ctrl Pts',(13.9908909448787,31.266100496257,8.7467275967966));
#60835=CARTESIAN_POINT('Ctrl Pts',(14.2704211048916,31.5163797260547,8.29960214590518));
#60836=CARTESIAN_POINT('Ctrl Pts',(14.838823971551,31.6394906306444,8.34914872097351));
#60837=CARTESIAN_POINT('Ctrl Pts',(13.9733426643655,31.34076551118,8.77473463235667));
#60838=CARTESIAN_POINT('Ctrl Pts',(14.253720076538,31.5855220469117,8.32824609388835));
#60839=CARTESIAN_POINT('Ctrl Pts',(14.8202121599515,31.7066891401708,8.3758827097203));
#60840=CARTESIAN_POINT('Ctrl Pts',(13.9646513850397,31.3782767417852,8.78855907279825));
#60841=CARTESIAN_POINT('Ctrl Pts',(14.2454446251434,31.6202717609735,8.342389472868));
#60842=CARTESIAN_POINT('Ctrl Pts',(14.8109941368322,31.7404492457889,8.38907876649581));
#60843=CARTESIAN_POINT('Ctrl Pts',(13.9217346730834,31.566257920696,8.85660464288024));
#60844=CARTESIAN_POINT('Ctrl Pts',(14.2046283298307,31.794206482269,8.41191502944778));
#60845=CARTESIAN_POINT('Ctrl Pts',(14.7654764146937,31.9096322969191,8.45403135644424));
#60846=CARTESIAN_POINT('Ctrl Pts',(13.8891759531169,31.7177786407323,8.90752381063715));
#60847=CARTESIAN_POINT('Ctrl Pts',(14.1735469248987,31.9348489839235,8.46411039451801));
#60848=CARTESIAN_POINT('Ctrl Pts',(14.7309444404168,32.0460009372101,8.50263601677879));
#60849=CARTESIAN_POINT('Ctrl Pts',(13.797229628424,32.1757915805991,9.04981828300803));
#60850=CARTESIAN_POINT('Ctrl Pts',(14.0858535568985,32.3596444525066,8.60976381822387));
#60851=CARTESIAN_POINT('Ctrl Pts',(14.6334256167163,32.458212559268,8.63846255958131));
#60852=CARTESIAN_POINT('Ctrl Pts',(13.7435707260252,32.4857275239348,9.13075893855157));
#60853=CARTESIAN_POINT('Ctrl Pts',(14.0343219801121,32.6485678536188,8.69311636580977));
#60854=CARTESIAN_POINT('Ctrl Pts',(14.5765146617579,32.7371548930406,8.71572409483911));
#60855=CARTESIAN_POINT('Ctrl Pts',(13.6537210422616,33.1151908161921,9.26457752924306));
#60856=CARTESIAN_POINT('Ctrl Pts',(13.9480657183463,33.2358005618801,8.83077671102261));
#60857=CARTESIAN_POINT('Ctrl Pts',(14.481219547549,33.3036718249763,8.84346002411218));
#60858=CARTESIAN_POINT('Ctrl Pts',(13.6175303913262,33.434717557105,9.31745805895241));
#60859=CARTESIAN_POINT('Ctrl Pts',(13.9131698025808,33.5346731534088,8.88537710590861));
#60860=CARTESIAN_POINT('Ctrl Pts',(14.4428355251485,33.5912458765277,8.89393689342034));
#60861=CARTESIAN_POINT('Ctrl Pts',(13.5846002426724,33.8405183507168,9.36529610646282));
#60862=CARTESIAN_POINT('Ctrl Pts',(13.88142692472,33.9146324799541,8.93474090246188));
#60863=CARTESIAN_POINT('Ctrl Pts',(14.4079096116133,33.956466571422,8.93960048526914));
#60864=CARTESIAN_POINT('Ctrl Pts',(13.5786296974971,33.9219987331534,9.37394813624565));
#60865=CARTESIAN_POINT('Ctrl Pts',(13.875675508425,33.9908623767473,8.94366201738552));
#60866=CARTESIAN_POINT('Ctrl Pts',(14.4015772154364,34.029798911697,8.94785924088037));
#60867=CARTESIAN_POINT('Ctrl Pts',(13.5706234030671,34.0447089994668,9.38553155036112));
#60868=CARTESIAN_POINT('Ctrl Pts',(13.8679615185176,34.1056958349204,8.9556072796306));
#60869=CARTESIAN_POINT('Ctrl Pts',(14.3930856914591,34.1402381454566,8.95891613645648));
#60870=CARTESIAN_POINT('Ctrl Pts',(13.568112892907,34.0856940452786,9.38916021637687));
#60871=CARTESIAN_POINT('Ctrl Pts',(13.8655426622907,34.144048511225,8.95934916121749));
#60872=CARTESIAN_POINT('Ctrl Pts',(14.3904230292606,34.1771246847184,8.96237986304967));
#60873=CARTESIAN_POINT('Ctrl Pts',(13.5634127761087,34.1678290467875,9.39594864334385));
#60874=CARTESIAN_POINT('Ctrl Pts',(13.8610138988738,34.2209130571112,8.9663495479683));
#60875=CARTESIAN_POINT('Ctrl Pts',(14.3854380571442,34.2510461821083,8.96885972533652));
#60876=CARTESIAN_POINT('Ctrl Pts',(13.561221484919,34.2090153261087,9.39911083275795));
#60877=CARTESIAN_POINT('Ctrl Pts',(13.8589022053104,34.2594602815295,8.9696108109939));
#60878=CARTESIAN_POINT('Ctrl Pts',(14.3831139605077,34.2881138315147,8.97187817888002));
#60879=CARTESIAN_POINT('Ctrl Pts',(13.5511043760099,34.4148121032376,9.41370128814102));
#60880=CARTESIAN_POINT('Ctrl Pts',(13.849155508049,34.45201534129,8.98465351724142));
#60881=CARTESIAN_POINT('Ctrl Pts',(14.3723836940155,34.4733309209789,8.98580543178569));
#60882=CARTESIAN_POINT('Ctrl Pts',(13.5456900690161,34.5790374616588,9.42148098687002));
#60883=CARTESIAN_POINT('Ctrl Pts',(13.8439323192676,34.6058139523128,8.99268414889771));
#60884=CARTESIAN_POINT('Ctrl Pts',(14.3666412473947,34.6211337356892,8.9932315081297));
#60885=CARTESIAN_POINT('Ctrl Pts',(13.537394573329,35.0705004043849,9.43340033567814));
#60886=CARTESIAN_POINT('Ctrl Pts',(13.8359355950147,35.065908922897,9.00497875543769));
#60887=CARTESIAN_POINT('Ctrl Pts',(14.3578429948253,35.0634503604854,9.00460906824679));
#60888=CARTESIAN_POINT('Ctrl Pts',(13.5424689320019,35.3965264297717,9.4261476475004));
#60889=CARTESIAN_POINT('Ctrl Pts',(13.840841926183,35.3715820736891,8.99747657812311));
#60890=CARTESIAN_POINT('Ctrl Pts',(14.3632248902148,35.356873767978,8.99768604786805));
#60891=CARTESIAN_POINT('Ctrl Pts',(13.5731452714314,36.04542889236,9.38192153491666));
#60892=CARTESIAN_POINT('Ctrl Pts',(13.8704062236138,35.9789562622814,8.95186307707126));
#60893=CARTESIAN_POINT('Ctrl Pts',(14.3957604001304,35.9408859530551,8.95547021242402));
#60894=CARTESIAN_POINT('Ctrl Pts',(13.5987464460997,36.3683053308453,9.34494758660724));
#60895=CARTESIAN_POINT('Ctrl Pts',(13.8951293553185,36.2813491153718,8.91364706576509));
#60896=CARTESIAN_POINT('Ctrl Pts',(14.4229131602539,36.231474732343,8.92017689772887));
#60897=CARTESIAN_POINT('Ctrl Pts',(13.6429948627497,36.7699519970002,9.28002899073296));
#60898=CARTESIAN_POINT('Ctrl Pts',(13.9376215104944,36.6560661788744,8.84688422821406));
#60899=CARTESIAN_POINT('Ctrl Pts',(14.4698432966875,36.5929567118635,8.85820914649669));
#60900=CARTESIAN_POINT('Ctrl Pts',(13.6524563224124,36.850183759103,9.26610806147943));
#60901=CARTESIAN_POINT('Ctrl Pts',(13.9467191680184,36.7310121656428,8.83254762593825));
#60902=CARTESIAN_POINT('Ctrl Pts',(14.4798781777861,36.6651652938272,8.84492098660861));
#60903=CARTESIAN_POINT('Ctrl Pts',(13.6675536049653,36.9703850215887,9.24381193101625));
#60904=CARTESIAN_POINT('Ctrl Pts',(13.9612232706366,36.8432141958407,8.80960244735883));
#60905=CARTESIAN_POINT('Ctrl Pts',(14.4958904463355,36.7733464241577,8.82363831640363));
#60906=CARTESIAN_POINT('Ctrl Pts',(13.6727368747274,37.0104277105771,9.23614406980858));
#60907=CARTESIAN_POINT('Ctrl Pts',(13.9662034537542,36.8805966404157,8.80170992007976));
#60908=CARTESIAN_POINT('Ctrl Pts',(14.5013878534575,36.8093848422754,8.81631899426101));
#60909=CARTESIAN_POINT('Ctrl Pts',(13.6834029259183,37.0904642664689,9.22033487953449));
#60910=CARTESIAN_POINT('Ctrl Pts',(13.9764488572415,36.9553002795284,8.7854406320722));
#60911=CARTESIAN_POINT('Ctrl Pts',(14.5127003314097,36.8814177386533,8.8012284033937));
#60912=CARTESIAN_POINT('Ctrl Pts',(13.6888901621671,37.1304892288409,9.21218691413121));
#60913=CARTESIAN_POINT('Ctrl Pts',(13.981718702735,36.9926517283056,8.77705647210948));
#60914=CARTESIAN_POINT('Ctrl Pts',(14.5185201272134,36.9174402028251,8.79345080003374));
#60915=CARTESIAN_POINT('Ctrl Pts',(13.7170045302029,37.3300355326774,9.17035509250042));
#60916=CARTESIAN_POINT('Ctrl Pts',(14.0087376674906,37.1790072230197,8.73397918025916));
#60917=CARTESIAN_POINT('Ctrl Pts',(14.54833839483,37.0970318665379,8.75352042409837));
#60918=CARTESIAN_POINT('Ctrl Pts',(13.7416559284244,37.4877914628441,9.13341262033751));
#60919=CARTESIAN_POINT('Ctrl Pts',(14.0323966113954,37.3261029988049,8.69597582707544));
#60920=CARTESIAN_POINT('Ctrl Pts',(14.5744838161833,37.2390121959723,8.71825715532235));
#60921=CARTESIAN_POINT('Ctrl Pts',(13.8215245864057,37.955680800248,9.01247985304086));
#60922=CARTESIAN_POINT('Ctrl Pts',(14.1090338931848,37.7625210439417,8.57154787918128));
#60923=CARTESIAN_POINT('Ctrl Pts',(14.6591929945098,37.6601125767095,8.60282133020325));
#60924=CARTESIAN_POINT('Ctrl Pts',(13.8826479129921,38.2604495486085,8.91841437366726));
#60925=CARTESIAN_POINT('Ctrl Pts',(14.1675770164119,38.045983743127,8.47485390450271));
#60926=CARTESIAN_POINT('Ctrl Pts',(14.7240207625428,37.9344044350983,8.51303155432319));
#60927=CARTESIAN_POINT('Ctrl Pts',(14.017864413363,38.8567193826118,8.7043383036793));
#60928=CARTESIAN_POINT('Ctrl Pts',(14.2964001885856,38.5986463447174,8.2557534008036));
#60929=CARTESIAN_POINT('Ctrl Pts',(14.867432194178,38.4710472548887,8.30868621311197));
#60930=CARTESIAN_POINT('Ctrl Pts',(14.0919600671857,39.1482188475984,8.58432510753208));
#60931=CARTESIAN_POINT('Ctrl Pts',(14.3668901384109,38.868224427513,8.13293860738287));
#60932=CARTESIAN_POINT('Ctrl Pts',(14.9460184901712,38.7333967582374,8.19412816209205));
#60933=CARTESIAN_POINT('Ctrl Pts',(14.1910981741539,39.5046875011412,8.41808951704303));
#60934=CARTESIAN_POINT('Ctrl Pts',(14.4602864178378,39.1952890069765,7.96429217292035));
#60935=CARTESIAN_POINT('Ctrl Pts',(15.0511649604324,39.0542185263549,8.03544873490342));
#60936=CARTESIAN_POINT('Ctrl Pts',(14.2112522061825,39.5755849617352,8.38402921489386));
#60937=CARTESIAN_POINT('Ctrl Pts',(14.4793252621244,39.2605217727158,7.92963051378782));
#60938=CARTESIAN_POINT('Ctrl Pts',(15.0725404478885,39.1180262370522,8.00293662835892));
#60939=CARTESIAN_POINT('Ctrl Pts',(14.2419443789457,39.6813410899015,8.33171225457276));
#60940=CARTESIAN_POINT('Ctrl Pts',(14.5082645353832,39.3576677969082,7.8764721428416));
#60941=CARTESIAN_POINT('Ctrl Pts',(15.1050927502537,39.2132067466253,7.9529977116705));
#60942=CARTESIAN_POINT('Ctrl Pts',(14.2522556469912,39.7165068507578,8.31406240552784));
#60943=CARTESIAN_POINT('Ctrl Pts',(14.5179878775877,39.3899757919214,7.8585332814314));
#60944=CARTESIAN_POINT('Ctrl Pts',(15.1160289430727,39.244855929495,7.93615012856782));
#60945=CARTESIAN_POINT('Ctrl Pts',(14.2729796736805,39.7864832103593,8.27843438972032));
#60946=CARTESIAN_POINT('Ctrl Pts',(14.5375184271283,39.454233053145,7.82233732493678));
#60947=CARTESIAN_POINT('Ctrl Pts',(15.1380089699858,39.3078346492803,7.90214156794191));
#60948=CARTESIAN_POINT('Ctrl Pts',(14.2833976444658,39.821312032634,8.26044739242331));
#60949=CARTESIAN_POINT('Ctrl Pts',(14.5473308926922,39.4861993542643,7.80407040917203));
#60950=CARTESIAN_POINT('Ctrl Pts',(15.1490583323553,39.3391805874545,7.88497216155336));
#60951=CARTESIAN_POINT('Ctrl Pts',(14.3357529130929,39.9946689703288,8.1696522999116));
#60952=CARTESIAN_POINT('Ctrl Pts',(14.5967120092205,39.6455467928789,7.71171681169117));
#60953=CARTESIAN_POINT('Ctrl Pts',(15.2045866440913,39.4952018220261,7.79830411842659));
#60954=CARTESIAN_POINT('Ctrl Pts',(14.3784853171976,40.1308377145353,8.09426602317428));
#60955=CARTESIAN_POINT('Ctrl Pts',(14.6368508121003,39.7702029993696,7.63528497359585));
#60956=CARTESIAN_POINT('Ctrl Pts',(15.2499088883933,39.6177536843613,7.72634449117004));
#60957=CARTESIAN_POINT('Ctrl Pts',(14.5087039436106,40.5321094868054,7.85998980656673));
#60958=CARTESIAN_POINT('Ctrl Pts',(14.7591580200955,40.1377641963223,7.39760736865633));
#60959=CARTESIAN_POINT('Ctrl Pts',(15.3880195437736,39.9788982574772,7.50271719341424));
#60960=CARTESIAN_POINT('Ctrl Pts',(14.5982023821632,40.7900005483541,7.69300623367248));
#60961=CARTESIAN_POINT('Ctrl Pts',(14.8426060415872,40.3722055486072,7.22904427170515));
#60962=CARTESIAN_POINT('Ctrl Pts',(15.4829421245151,40.2110001980916,7.34332378435791));
#60963=CARTESIAN_POINT('Ctrl Pts',(14.7800664680989,41.2876229200236,7.33753997602127));
#60964=CARTESIAN_POINT('Ctrl Pts',(15.0109560529092,40.8221747459924,6.87233168107768));
#60965=CARTESIAN_POINT('Ctrl Pts',(15.675828261863,40.6588603029792,7.00401508691933));
#60966=CARTESIAN_POINT('Ctrl Pts',(14.8724375414028,41.52735181651,7.14905700140747));
#60967=CARTESIAN_POINT('Ctrl Pts',(15.095954979395,41.0376573972687,6.68377387394993));
#60968=CARTESIAN_POINT('Ctrl Pts',(15.7737975755315,40.8746162950652,6.82409952271975));
#60969=CARTESIAN_POINT('Ctrl Pts',(15.0114481107896,41.8736142592902,6.84971015627378));
#60970=CARTESIAN_POINT('Ctrl Pts',(15.2224090930038,41.3459299263025,6.38732005887134));
#60971=CARTESIAN_POINT('Ctrl Pts',(15.9212330152907,41.1862524710463,6.53835935782291));
#60972=CARTESIAN_POINT('Ctrl Pts',(15.0578619379628,41.9868080692592,6.74715158759131));
#60973=CARTESIAN_POINT('Ctrl Pts',(15.2646135022824,41.4466957957362,6.2856493085689));
#60974=CARTESIAN_POINT('Ctrl Pts',(15.9704597981201,41.2881268926528,6.44046254412343));
#60975=CARTESIAN_POINT('Ctrl Pts',(15.1158035851444,42.1255077461633,6.61538440065119));
#60976=CARTESIAN_POINT('Ctrl Pts',(15.3169420693408,41.5694200795832,6.15578753526126));
#60977=CARTESIAN_POINT('Ctrl Pts',(16.0319130547786,41.4129565926847,6.31468477759303));
#60978=CARTESIAN_POINT('Ctrl Pts',(15.1273876432894,42.1531065685038,6.5888532043739));
#60979=CARTESIAN_POINT('Ctrl Pts',(15.3274204676051,41.5938817796405,6.12959010828534));
#60980=CARTESIAN_POINT('Ctrl Pts',(16.0441991761153,41.4377955309865,6.28935954534903));
#60981=CARTESIAN_POINT('Ctrl Pts',(15.1504884935602,42.2078934932818,6.53555979741833));
#60982=CARTESIAN_POINT('Ctrl Pts',(15.3482944605132,41.6423974913488,6.07700707977798));
#60983=CARTESIAN_POINT('Ctrl Pts',(16.0687000757785,41.4871037596636,6.23848856701855));
#60984=CARTESIAN_POINT('Ctrl Pts',(15.16201224007,42.2350982910057,6.50878184192637));
#60985=CARTESIAN_POINT('Ctrl Pts',(15.358696260029,41.6664657192515,6.05060545885006));
#60986=CARTESIAN_POINT('Ctrl Pts',(16.0809222302044,41.511588075854,6.21292779194116));
#60987=CARTESIAN_POINT('Ctrl Pts',(15.1964975395775,42.3161505365769,6.4280547185655));
#60988=CARTESIAN_POINT('Ctrl Pts',(15.3898184625834,41.7381711202028,5.97100372060078));
#60989=CARTESIAN_POINT('Ctrl Pts',(16.1174975446523,41.5845350915181,6.13587008487654));
#60990=CARTESIAN_POINT('Ctrl Pts',(15.2193731284631,42.369435949201,6.37371235824478));
#60991=CARTESIAN_POINT('Ctrl Pts',(15.4103998557409,41.785178466038,5.91754508925415));
#60992=CARTESIAN_POINT('Ctrl Pts',(16.1417595309143,41.6324919593784,6.08399783316048));
#60993=CARTESIAN_POINT('Ctrl Pts',(15.3331009005101,42.6321602692512,6.09938186690947));
#60994=CARTESIAN_POINT('Ctrl Pts',(15.5130467364772,42.0177626523262,5.64666607840681));
#60995=CARTESIAN_POINT('Ctrl Pts',(16.2623798847315,41.8689438306172,5.82213691472101));
#60996=CARTESIAN_POINT('Ctrl Pts',(15.4219981693841,42.8305241152713,5.87155766518555));
#60997=CARTESIAN_POINT('Ctrl Pts',(15.5920752292007,42.1908243853748,5.42418175931921));
#60998=CARTESIAN_POINT('Ctrl Pts',(16.3566648587587,42.0474712782004,5.60466836487157));
#60999=CARTESIAN_POINT('Ctrl Pts',(15.5937398520647,43.2042079887926,5.39893455941937));
#61000=CARTESIAN_POINT('Ctrl Pts',(15.7433940983337,42.5145580603963,4.96612969069518));
#61001=CARTESIAN_POINT('Ctrl Pts',(16.5388151099388,42.3837867376654,5.15352814195569));
#61002=CARTESIAN_POINT('Ctrl Pts',(15.6765892287066,43.3795270223867,5.1541366866717));
#61003=CARTESIAN_POINT('Ctrl Pts',(15.8155572122032,42.6648295333535,4.73048547856337));
#61004=CARTESIAN_POINT('Ctrl Pts',(16.6266856526138,42.5415738546014,4.91985745378921));
#61005=CARTESIAN_POINT('Ctrl Pts',(15.8343896714213,43.7068883556104,4.64679228744702));
#61006=CARTESIAN_POINT('Ctrl Pts',(15.9517394444224,42.9433539713678,4.24602967800665));
#61007=CARTESIAN_POINT('Ctrl Pts',(16.7940497399473,42.8361990298401,4.43557418320846));
#61008=CARTESIAN_POINT('Ctrl Pts',(15.9093461307783,43.8589341148382,4.38424982322478));
#61009=CARTESIAN_POINT('Ctrl Pts',(16.0155885969954,43.0711748346473,3.99726291403837));
#61010=CARTESIAN_POINT('Ctrl Pts',(16.8735490068819,42.9730402005446,4.18496547848737));
#61011=CARTESIAN_POINT('Ctrl Pts',(15.9968739190125,44.0337693958938,4.04412643478191));
#61012=CARTESIAN_POINT('Ctrl Pts',(16.0891131415095,43.2163723621957,3.67917462890213));
#61013=CARTESIAN_POINT('Ctrl Pts',(16.9663814979273,43.130391939171,3.86030226102062));
#61014=CARTESIAN_POINT('Ctrl Pts',(16.0140705480854,44.0679730886499,3.97550284079341));
#61015=CARTESIAN_POINT('Ctrl Pts',(16.1035854874514,43.24484060037,3.6148164769343));
#61016=CARTESIAN_POINT('Ctrl Pts',(16.9846203450266,43.1611752596937,3.79479792452804));
#61017=CARTESIAN_POINT('Ctrl Pts',(16.0393769684763,44.11811371591,3.87164771798298));
#61018=CARTESIAN_POINT('Ctrl Pts',(16.1248097475127,43.2864454847151,3.5176909846929));
#61019=CARTESIAN_POINT('Ctrl Pts',(17.0114604845068,43.2063018202117,3.6956634942118));
#61020=CARTESIAN_POINT('Ctrl Pts',(16.0477158723614,44.1346030656301,3.83693785631023));
#61021=CARTESIAN_POINT('Ctrl Pts',(16.1317988050306,43.300120944147,3.48523803964491));
#61022=CARTESIAN_POINT('Ctrl Pts',(17.0203047755308,43.2211422335718,3.66253135522116));
#61023=CARTESIAN_POINT('Ctrl Pts',(16.0641840025573,44.1671063213702,3.76739554137956));
#61024=CARTESIAN_POINT('Ctrl Pts',(16.1455826144819,43.3270461204439,3.42028257915105));
#61025=CARTESIAN_POINT('Ctrl Pts',(17.0377709720975,43.2503951610147,3.59615005800666));
#61026=CARTESIAN_POINT('Ctrl Pts',(16.0723155893667,44.1831249045866,3.73255341105548));
#61027=CARTESIAN_POINT('Ctrl Pts',(16.1523788294993,43.3402986366979,3.38777194787044));
#61028=CARTESIAN_POINT('Ctrl Pts',(17.0463953813549,43.2648118846088,3.56289166263266));
#61029=CARTESIAN_POINT('Ctrl Pts',(16.112456458332,44.2620570473186,3.55798830906263));
#61030=CARTESIAN_POINT('Ctrl Pts',(16.1859599003788,43.4056750884538,3.22467629046144));
#61031=CARTESIAN_POINT('Ctrl Pts',(17.0889690250921,43.3358508065297,3.39626134644081));
#61032=CARTESIAN_POINT('Ctrl Pts',(16.1429146628079,44.321490558741,3.41720255158772));
#61033=CARTESIAN_POINT('Ctrl Pts',(16.2112170112945,43.4545025083997,3.09399963066693));
#61034=CARTESIAN_POINT('Ctrl Pts',(17.1212731775395,43.389340961842,3.26187494898354));
#61035=CARTESIAN_POINT('Ctrl Pts',(16.229144054607,44.4887700038955,2.99144640783051));
#61036=CARTESIAN_POINT('Ctrl Pts',(16.282607511081,43.591807170456,2.6991480196057));
#61037=CARTESIAN_POINT('Ctrl Pts',(17.2127285815789,43.5398924483796,2.85547137921157));
#61038=CARTESIAN_POINT('Ctrl Pts',(16.2797738357512,44.5856221569172,2.70308430094746));
#61039=CARTESIAN_POINT('Ctrl Pts',(16.3237841620316,43.6700048185059,2.43483412170548));
#61040=CARTESIAN_POINT('Ctrl Pts',(17.2664268276358,43.6270593773696,2.58021665754872));
#61041=CARTESIAN_POINT('Ctrl Pts',(16.3662877960953,44.7499338788673,2.11715012589449));
#61042=CARTESIAN_POINT('Ctrl Pts',(16.3937978726645,43.8021685587023,1.90074237494269));
#61043=CARTESIAN_POINT('Ctrl Pts',(17.3581840457416,43.7749399125848,2.02091588916502));
#61044=CARTESIAN_POINT('Ctrl Pts',(16.402174958515,44.8173953240164,1.8195789350148));
#61045=CARTESIAN_POINT('Ctrl Pts',(16.4224358551378,43.8557423131687,1.6316735546018));
#61046=CARTESIAN_POINT('Ctrl Pts',(17.3962461828893,43.8356552065899,1.73687068039507));
#61047=CARTESIAN_POINT('Ctrl Pts',(16.4440583713838,44.8958262298579,1.36601500577945));
#61048=CARTESIAN_POINT('Ctrl Pts',(16.4557537708206,43.9178757918761,1.22353172397691));
#61049=CARTESIAN_POINT('Ctrl Pts',(17.4406679778708,43.9062430148725,1.30392332311912));
#61050=CARTESIAN_POINT('Ctrl Pts',(16.4560267904858,44.9181691585247,1.21362389233826));
#61051=CARTESIAN_POINT('Ctrl Pts',(16.465245045828,43.9355291501292,1.08657788633077));
#61052=CARTESIAN_POINT('Ctrl Pts',(17.4533617541891,43.9263516483037,1.15845908846732));
#61053=CARTESIAN_POINT('Ctrl Pts',(16.4708618799835,44.9458224158849,0.98317551882238));
#61054=CARTESIAN_POINT('Ctrl Pts',(16.476991410704,43.9573497406529,0.879856072656254));
#61055=CARTESIAN_POINT('Ctrl Pts',(17.4690959376098,43.9512395775681,0.938485656355758));
#61056=CARTESIAN_POINT('Ctrl Pts',(16.4752871841395,44.9540627945076,0.906048965804147));
#61057=CARTESIAN_POINT('Ctrl Pts',(16.4804918339109,43.9638465742228,0.810700730796114));
#61058=CARTESIAN_POINT('Ctrl Pts',(17.4737894414959,43.9586559173861,0.864864860870638));
#61059=CARTESIAN_POINT('Ctrl Pts',(16.4811281425855,44.9649323439329,0.789884978814111));
#61060=CARTESIAN_POINT('Ctrl Pts',(16.4851083683136,43.9724103538098,0.706624078649839));
#61061=CARTESIAN_POINT('Ctrl Pts',(17.4799843964452,43.9684385109803,0.753981062883885));
#61062=CARTESIAN_POINT('Ctrl Pts',(16.4829427373917,44.9683078282227,0.751074106761979));
#61063=CARTESIAN_POINT('Ctrl Pts',(16.4865420704517,43.9750690241147,0.671857267230879));
#61064=CARTESIAN_POINT('Ctrl Pts',(17.4819089664434,43.9714764465119,0.716934323975719));
#61065=CARTESIAN_POINT('Ctrl Pts',(16.4863013241423,44.9745536029427,0.673336652475124));
#61066=CARTESIAN_POINT('Ctrl Pts',(16.4891948319328,43.9799871259377,0.602238655241295));
#61067=CARTESIAN_POINT('Ctrl Pts',(17.4854711034336,43.9770976431059,0.642730395542892));
#61068=CARTESIAN_POINT('Ctrl Pts',(16.4878418236565,44.9774174003737,0.634492642641704));
#61069=CARTESIAN_POINT('Ctrl Pts',(16.4904109816433,43.9822411637506,0.567462772022506));
#61070=CARTESIAN_POINT('Ctrl Pts',(17.4871049662947,43.9796750605875,0.605652025131273));
#61071=CARTESIAN_POINT('Ctrl Pts',(16.4948535761857,44.9904491876333,0.44039544480284));
#61072=CARTESIAN_POINT('Ctrl Pts',(16.4959475121185,43.9925006421478,0.393653808714096));
#61073=CARTESIAN_POINT('Ctrl Pts',(17.4945416725464,43.9914036677432,0.420377440177512));
#61074=CARTESIAN_POINT('Ctrl Pts',(16.4982530996368,44.9967581364226,0.285510603939235));
#61075=CARTESIAN_POINT('Ctrl Pts',(16.4986230123992,43.9974523683355,0.255222110228282));
#61076=CARTESIAN_POINT('Ctrl Pts',(17.4981472271006,43.9970817212605,0.272532829876073));
#61077=CARTESIAN_POINT('Ctrl Pts',(16.5007066493061,45.0013123694504,-0.0234886818206301));
#61078=CARTESIAN_POINT('Ctrl Pts',(16.5005562753881,44.001030959175,-0.0210215393702913));
#61079=CARTESIAN_POINT('Ctrl Pts',(17.5007494764801,44.0011805303849,-0.0224210128910837));
#61080=CARTESIAN_POINT('Ctrl Pts',(16.4997606328126,44.999557489536,-0.177603113095881));
#61081=CARTESIAN_POINT('Ctrl Pts',(16.4998121438015,43.9996542479657,-0.158706164302627));
#61082=CARTESIAN_POINT('Ctrl Pts',(17.4997461257051,43.9996011387621,-0.16953023225577));
#61083=CARTESIAN_POINT('Ctrl Pts',(16.4935850865834,44.9880905305289,-0.485071950900073));
#61084=CARTESIAN_POINT('Ctrl Pts',(16.4949439253717,43.9906402228509,-0.433673029434492));
#61085=CARTESIAN_POINT('Ctrl Pts',(17.4931963049589,43.989280876643,-0.46302319302334));
#61086=CARTESIAN_POINT('Ctrl Pts',(16.4883555209821,44.9783783650866,-0.638426349728915));
#61087=CARTESIAN_POINT('Ctrl Pts',(16.4908241367169,43.983010890298,-0.570831093510023));
#61088=CARTESIAN_POINT('Ctrl Pts',(17.4876497967006,43.9805399287279,-0.609406926989948));
#61089=CARTESIAN_POINT('Ctrl Pts',(16.4736638585154,44.951044676118,-0.944380784970185));
#61090=CARTESIAN_POINT('Ctrl Pts',(16.4792132612985,43.9614766171799,-0.844947715891262));
#61091=CARTESIAN_POINT('Ctrl Pts',(17.47206773271,43.9559396112014,-0.901454321999671));
#61092=CARTESIAN_POINT('Ctrl Pts',(16.4642017308171,44.9334231368575,-1.09698081900314));
#61093=CARTESIAN_POINT('Ctrl Pts',(16.4717324138027,43.9475908096718,-0.981785275421627));
#61094=CARTESIAN_POINT('Ctrl Pts',(17.4620321440808,43.940080227518,-1.04711798067983));
#61095=CARTESIAN_POINT('Ctrl Pts',(16.441085917582,44.8902614198252,-1.40142762961972));
#61096=CARTESIAN_POINT('Ctrl Pts',(16.4533815640137,43.9134527552254,-1.25544439804365));
#61097=CARTESIAN_POINT('Ctrl Pts',(17.4375153759351,43.9012346862572,-1.33772627995896));
#61098=CARTESIAN_POINT('Ctrl Pts',(16.4274322046631,44.8647212958546,-1.55327440899518));
#61099=CARTESIAN_POINT('Ctrl Pts',(16.4425275239753,43.8932305455644,-1.39214821663313));
#61100=CARTESIAN_POINT('Ctrl Pts',(17.4230341672312,43.8782485769846,-1.48267092310701));
#61101=CARTESIAN_POINT('Ctrl Pts',(16.4038318406658,44.8204219027532,-1.78047704290001));
#61102=CARTESIAN_POINT('Ctrl Pts',(16.4236582623586,43.8579704062684,-1.59747887342057));
#61103=CARTESIAN_POINT('Ctrl Pts',(17.3980034815883,43.8383791273345,-1.69954615022252));
#61104=CARTESIAN_POINT('Ctrl Pts',(16.3954450179849,44.8046567812815,-1.85611662919189));
#61105=CARTESIAN_POINT('Ctrl Pts',(16.4169484530449,43.8454168392665,-1.66586277048818));
#61106=CARTESIAN_POINT('Ctrl Pts',(17.3891083678211,43.8241905193902,-1.77174756870095));
#61107=CARTESIAN_POINT('Ctrl Pts',(16.3820871255076,44.7795006112695,-1.96943341649774));
#61108=CARTESIAN_POINT('Ctrl Pts',(16.4062319638247,43.8253349631854,-1.768514534337));
#61109=CARTESIAN_POINT('Ctrl Pts',(17.3749409080326,43.8015499687257,-1.879913585899));
#61110=CARTESIAN_POINT('Ctrl Pts',(16.377504880929,44.770863776863,-2.00718191127611));
#61111=CARTESIAN_POINT('Ctrl Pts',(16.4025541708227,43.8184380318085,-1.80271826733453));
#61112=CARTESIAN_POINT('Ctrl Pts',(17.3700809523118,43.7937768185068,-1.91594623764296));
#61113=CARTESIAN_POINT('Ctrl Pts',(16.3680815161057,44.7530851039602,-2.08263122802109));
#61114=CARTESIAN_POINT('Ctrl Pts',(16.3949823625954,43.8042269216823,-1.87113562920749));
#61115=CARTESIAN_POINT('Ctrl Pts',(17.3600864758251,43.7777760145525,-1.98796603532164));
#61116=CARTESIAN_POINT('Ctrl Pts',(16.3632376023291,44.7439379841849,-2.12035312043325));
#61117=CARTESIAN_POINT('Ctrl Pts',(16.3910864954017,43.7969092708944,-1.90536667503487));
#61118=CARTESIAN_POINT('Ctrl Pts',(17.3549489921576,43.7695436076108,-2.02397329393255));
#61119=CARTESIAN_POINT('Ctrl Pts',(16.3384034872043,44.6969941607675,-2.30860270705501));
#61120=CARTESIAN_POINT('Ctrl Pts',(16.3711201266365,43.7593731860622,-2.0760735616022));
#61121=CARTESIAN_POINT('Ctrl Pts',(17.328609782944,43.727294170591,-2.20366606939342));
#61122=CARTESIAN_POINT('Ctrl Pts',(16.316666398052,44.6557569516807,-2.45734547442349));
#61123=CARTESIAN_POINT('Ctrl Pts',(16.3535610329279,43.7262614947939,-2.21154871046545));
#61124=CARTESIAN_POINT('Ctrl Pts',(17.3055552971597,43.6901806864659,-2.34564779295502));
#61125=CARTESIAN_POINT('Ctrl Pts',(16.2696860394868,44.566166141375,-2.75126612719684));
#61126=CARTESIAN_POINT('Ctrl Pts',(16.315383867761,43.6539391818024,-2.48026578450734));
#61127=CARTESIAN_POINT('Ctrl Pts',(17.2557276510028,43.609548964849,-2.62620839879226));
#61128=CARTESIAN_POINT('Ctrl Pts',(16.2444425920206,44.5178122627343,-2.89644386444925));
#61129=CARTESIAN_POINT('Ctrl Pts',(16.2947921426187,43.6147800923035,-2.61343081272645));
#61130=CARTESIAN_POINT('Ctrl Pts',(17.2289543007661,43.5660304785905,-2.76478713969546));
#61131=CARTESIAN_POINT('Ctrl Pts',(16.1637732673119,44.3623460870145,-3.32680665282513));
#61132=CARTESIAN_POINT('Ctrl Pts',(16.228751596228,43.4885065479902,-3.00872279958398));
#61133=CARTESIAN_POINT('Ctrl Pts',(17.1433959375855,43.4261109338679,-3.17558795847649));
#61134=CARTESIAN_POINT('Ctrl Pts',(16.1034130962697,44.2448568131152,-3.60683310989697));
#61135=CARTESIAN_POINT('Ctrl Pts',(16.1788594609402,43.3922946051711,-3.26840131996947));
#61136=CARTESIAN_POINT('Ctrl Pts',(17.0793775817667,43.3203705977857,-3.44288592546756));
#61137=CARTESIAN_POINT('Ctrl Pts',(15.971082818307,43.9829218056908,-4.15375397007533));
#61138=CARTESIAN_POINT('Ctrl Pts',(16.0678613880117,43.1749038617298,-3.78004646974489));
#61139=CARTESIAN_POINT('Ctrl Pts',(16.9390273041549,43.0846291125409,-3.96494672006258));
#61140=CARTESIAN_POINT('Ctrl Pts',(15.8991086468391,43.8384751876644,-4.42064712392545));
#61141=CARTESIAN_POINT('Ctrl Pts',(16.0069841963327,43.0542208336615,-4.03164651818705));
#61142=CARTESIAN_POINT('Ctrl Pts',(16.8626910699957,42.9546271680979,-4.2197083547663));
#61143=CARTESIAN_POINT('Ctrl Pts',(15.8027846939592,43.6409776592958,-4.74622028184776));
#61144=CARTESIAN_POINT('Ctrl Pts',(15.9239456942855,42.8862343965702,-4.3427395313841));
#61145=CARTESIAN_POINT('Ctrl Pts',(16.7605293128805,42.7768794073196,-4.53048272074057));
#61146=CARTESIAN_POINT('Ctrl Pts',(15.7832020058401,43.6006290479835,-4.81093189184897));
#61147=CARTESIAN_POINT('Ctrl Pts',(15.9071072368669,42.8520156916865,-4.40437522421748));
#61148=CARTESIAN_POINT('Ctrl Pts',(16.7397597973034,42.740565660211,-4.59225289128511));
#61149=CARTESIAN_POINT('Ctrl Pts',(15.7533680246834,43.5388242348736,-4.90739530557529));
#61150=CARTESIAN_POINT('Ctrl Pts',(15.8813574947029,42.7994203500316,-4.49651575444794));
#61151=CARTESIAN_POINT('Ctrl Pts',(16.7081176995267,42.684941333135,-4.68433160073687));
#61152=CARTESIAN_POINT('Ctrl Pts',(15.7433467070133,43.5180089530702,-4.93944909919554));
#61153=CARTESIAN_POINT('Ctrl Pts',(15.8727041546145,42.7817018827648,-4.52713625468849));
#61154=CARTESIAN_POINT('Ctrl Pts',(16.6974890303406,42.6662075810719,-4.71492840247447));
#61155=CARTESIAN_POINT('Ctrl Pts',(15.7231535893805,43.4759493179362,-5.00335528875631));
#61156=CARTESIAN_POINT('Ctrl Pts',(15.8552432110586,42.7458557749306,-4.58824457822864));
#61157=CARTESIAN_POINT('Ctrl Pts',(16.6760720897177,42.628353912667,-4.77592976284654));
#61158=CARTESIAN_POINT('Ctrl Pts',(15.7129877823714,43.4547173657021,-5.03518828987221));
#61159=CARTESIAN_POINT('Ctrl Pts',(15.8464411539109,42.7277396174676,-4.61871374081455));
#61160=CARTESIAN_POINT('Ctrl Pts',(16.6652901742407,42.6092451572783,-4.80631580816218));
#61161=CARTESIAN_POINT('Ctrl Pts',(15.6619216546864,43.3477580321763,-5.19344863237848));
#61162=CARTESIAN_POINT('Ctrl Pts',(15.8022819829115,42.6366080996778,-4.76993809467135));
#61163=CARTESIAN_POINT('Ctrl Pts',(16.6111291357615,42.512981765177,-4.95738249258125));
#61164=CARTESIAN_POINT('Ctrl Pts',(15.6202189508121,43.2594435926603,-5.31745448945332));
#61165=CARTESIAN_POINT('Ctrl Pts',(15.7659413926522,42.5608428041457,-4.88922064491253));
#61166=CARTESIAN_POINT('Ctrl Pts',(16.566898999381,42.4334987763842,-5.07575171548048));
#61167=CARTESIAN_POINT('Ctrl Pts',(15.4929526417546,42.9864272209814,-5.68195984817183));
#61168=CARTESIAN_POINT('Ctrl Pts',(15.6548243306024,42.3262950844098,-5.23984103420753));
#61169=CARTESIAN_POINT('Ctrl Pts',(16.431919595095,42.1877840621362,-5.42368863587617));
#61170=CARTESIAN_POINT('Ctrl Pts',(15.4052313951022,42.7936764333705,-5.91496728026137));
#61171=CARTESIAN_POINT('Ctrl Pts',(15.5772391839006,42.1588707010981,-5.46658244560214));
#61172=CARTESIAN_POINT('Ctrl Pts',(16.3388819173383,42.0143083672418,-5.64610481430131));
#61173=CARTESIAN_POINT('Ctrl Pts',(15.2260498958022,42.3869745661045,-6.36202772981797));
#61174=CARTESIAN_POINT('Ctrl Pts',(15.4171543510239,41.8022449748656,-5.90416869454143));
#61175=CARTESIAN_POINT('Ctrl Pts',(16.1488409510981,41.6482767143899,-6.07284432319289));
#61176=CARTESIAN_POINT('Ctrl Pts',(15.134584339902,42.1730236614296,-6.57607876549311));
#61177=CARTESIAN_POINT('Ctrl Pts',(15.3347222581386,41.6133575955481,-6.11522249445178));
#61178=CARTESIAN_POINT('Ctrl Pts',(16.051832035793,41.4557209144361,-6.27716576157246));
#61179=CARTESIAN_POINT('Ctrl Pts',(14.9961179851292,41.8358199562313,-6.88324481216384));
#61180=CARTESIAN_POINT('Ctrl Pts',(15.2084472214612,41.3122217578598,-6.42057772001959));
#61181=CARTESIAN_POINT('Ctrl Pts',(15.9049737927767,41.1522376006794,-6.57036971072575));
#61182=CARTESIAN_POINT('Ctrl Pts',(14.9497520217687,41.7206997451385,-6.98331039827688));
#61183=CARTESIAN_POINT('Ctrl Pts',(15.16614239646,41.2094392579748,-6.52001184677474));
#61184=CARTESIAN_POINT('Ctrl Pts',(15.8557977745928,41.0486294178944,-6.66588685926462));
#61185=CARTESIAN_POINT('Ctrl Pts',(14.8800931267622,41.5438354639073,-7.12991977140524));
#61186=CARTESIAN_POINT('Ctrl Pts',(15.1022410222233,41.0507224912159,-6.666282802179));
#61187=CARTESIAN_POINT('Ctrl Pts',(15.7819171342091,40.8894515756627,-6.80583216820748));
#61188=CARTESIAN_POINT('Ctrl Pts',(14.8568552878022,41.484182951149,-7.1782077589911));
#61189=CARTESIAN_POINT('Ctrl Pts',(15.0809202996962,40.9971980762009,-6.71444353496276));
#61190=CARTESIAN_POINT('Ctrl Pts',(15.7572709430864,40.8357643178049,-6.85192524646453));
#61191=CARTESIAN_POINT('Ctrl Pts',(14.8219981963677,41.3936403419064,-7.24976367789764));
#61192=CARTESIAN_POINT('Ctrl Pts',(15.0488556165099,40.9157605080403,-6.78595401277065));
#61193=CARTESIAN_POINT('Ctrl Pts',(15.720301303522,40.7542759750313,-6.92022862282764));
#61194=CARTESIAN_POINT('Ctrl Pts',(14.8103768169327,41.3632758321973,-7.27347409955783));
#61195=CARTESIAN_POINT('Ctrl Pts',(15.0381645224724,40.8884513593707,-6.80964490693201));
#61196=CARTESIAN_POINT('Ctrl Pts',(15.7079755988858,40.7269479181449,-6.94286129770825));
#61197=CARTESIAN_POINT('Ctrl Pts',(14.7871949947469,41.3023381908314,-7.32048844844451));
#61198=CARTESIAN_POINT('Ctrl Pts',(15.0168199878777,40.8336038430639,-6.85664802598089));
#61199=CARTESIAN_POINT('Ctrl Pts',(15.6833888197048,40.6721040445935,-6.98773863017686));
#61200=CARTESIAN_POINT('Ctrl Pts',(14.7756276476925,41.2717472261591,-7.34380663171041));
#61201=CARTESIAN_POINT('Ctrl Pts',(15.0061600357127,40.8060495548255,-6.8799753372946));
#61202=CARTESIAN_POINT('Ctrl Pts',(15.6711204221094,40.6445721782689,-7.00999689573379));
#61203=CARTESIAN_POINT('Ctrl Pts',(14.6717534680737,40.9953295236136,-7.551980979435));
#61204=CARTESIAN_POINT('Ctrl Pts',(14.910895023212,40.5582946685239,-7.08717243073097));
#61205=CARTESIAN_POINT('Ctrl Pts',(15.5609508466639,40.3957962636541,-7.20870876993529));
#61206=CARTESIAN_POINT('Ctrl Pts',(14.5810647211324,40.741832913012,-7.72504743234233));
#61207=CARTESIAN_POINT('Ctrl Pts',(14.8266034407128,40.3284650320611,-7.26150923309475));
#61208=CARTESIAN_POINT('Ctrl Pts',(15.4647658178036,40.1676493290605,-7.37390856444987));
#61209=CARTESIAN_POINT('Ctrl Pts',(14.4053000909514,40.2189658652342,-8.04805166012557));
#61210=CARTESIAN_POINT('Ctrl Pts',(14.6624713147881,39.8520942263093,-7.58761069327075));
#61211=CARTESIAN_POINT('Ctrl Pts',(15.2783487987737,39.6970690159146,-7.68223078049221));
#61212=CARTESIAN_POINT('Ctrl Pts',(14.3202196741063,39.9495964563036,-8.19798859025269));
#61213=CARTESIAN_POINT('Ctrl Pts',(14.5824821731141,39.6054725337204,-7.73982483051287));
#61214=CARTESIAN_POINT('Ctrl Pts',(15.1881119978371,39.4546365627441,-7.82535239493351));
#61215=CARTESIAN_POINT('Ctrl Pts',(14.1987070119549,39.5329899966079,-8.40554259396074));
#61216=CARTESIAN_POINT('Ctrl Pts',(14.4675712776125,39.2216395207323,-7.95135792883057));
#61217=CARTESIAN_POINT('Ctrl Pts',(15.0592349397921,39.0796907709945,-8.02347212656833));
#61218=CARTESIAN_POINT('Ctrl Pts',(14.1592228767318,39.3920245639935,-8.47182899757806));
#61219=CARTESIAN_POINT('Ctrl Pts',(14.4302307228589,39.0918382370354,-8.01887552296388));
#61220=CARTESIAN_POINT('Ctrl Pts',(15.0173578287548,38.9528218891227,-8.08674551157961));
#61221=CARTESIAN_POINT('Ctrl Pts',(14.0826436992676,39.1057333760433,-8.59852461046018));
#61222=CARTESIAN_POINT('Ctrl Pts',(14.3576897375667,38.8277840539175,-8.14804214154577));
#61223=CARTESIAN_POINT('Ctrl Pts',(14.9361374939208,38.6951598352862,-8.20768223360701));
#61224=CARTESIAN_POINT('Ctrl Pts',(14.0455484751751,38.9604078024459,-8.65893401842002));
#61225=CARTESIAN_POINT('Ctrl Pts',(14.3224658365587,38.6935038701764,-8.20974266782632));
#61226=CARTESIAN_POINT('Ctrl Pts',(14.8967940762729,38.564366826571,-8.26534575917441));
#61227=CARTESIAN_POINT('Ctrl Pts',(13.9741231020615,38.6651847931096,-8.77373659465044));
#61228=CARTESIAN_POINT('Ctrl Pts',(14.2545506255991,38.4203292745446,-8.32708424104715));
#61229=CARTESIAN_POINT('Ctrl Pts',(14.8210398970475,38.2986661336681,-8.37493003741839));
#61230=CARTESIAN_POINT('Ctrl Pts',(13.9397927396565,38.5152876114838,-8.82813006373624));
#61231=CARTESIAN_POINT('Ctrl Pts',(14.2218349017627,38.2814009529421,-8.38277478959687));
#61232=CARTESIAN_POINT('Ctrl Pts',(14.7846289082318,38.1637586777924,-8.42685107588136));
#61233=CARTESIAN_POINT('Ctrl Pts',(13.8906779238092,38.2868159369556,-8.90505431363061));
#61234=CARTESIAN_POINT('Ctrl Pts',(14.1749330362927,38.0691860959213,-8.46165291031302));
#61235=CARTESIAN_POINT('Ctrl Pts',(14.7325374397322,37.9581341823412,-8.50027876989112));
#61236=CARTESIAN_POINT('Ctrl Pts',(13.8747711745264,38.2103676139026,-8.92981141108521));
#61237=CARTESIAN_POINT('Ctrl Pts',(14.1597438957798,37.9981958667913,-8.48703108097704));
#61238=CARTESIAN_POINT('Ctrl Pts',(14.7156666457513,37.8893306954536,-8.5239105447298));
#61239=CARTESIAN_POINT('Ctrl Pts',(13.8439407534612,38.0569848263093,-8.977533703511));
#61240=CARTESIAN_POINT('Ctrl Pts',(14.1302874730393,37.855684813066,-8.53596677843347));
#61241=CARTESIAN_POINT('Ctrl Pts',(14.6829677161225,37.7512861943861,-8.569463642424));
#61242=CARTESIAN_POINT('Ctrl Pts',(13.8290135932356,37.9800341471073,-9.00050435994528));
#61243=CARTESIAN_POINT('Ctrl Pts',(14.1160133673981,37.7841410413401,-8.5595362357428));
#61244=CARTESIAN_POINT('Ctrl Pts',(14.6671358801619,37.6820305869951,-8.59139017821769));
#61245=CARTESIAN_POINT('Ctrl Pts',(13.7568984117905,37.5939762225734,-9.11092076643811));
#61246=CARTESIAN_POINT('Ctrl Pts',(14.0471914590982,37.4259317837796,-8.67257888611769));
#61247=CARTESIAN_POINT('Ctrl Pts',(14.5906500859663,37.3345784750488,-8.6967876579279));
#61248=CARTESIAN_POINT('Ctrl Pts',(13.7072727192612,37.2809629485317,-9.185091616072));
#61249=CARTESIAN_POINT('Ctrl Pts',(13.9994761483249,37.1338465170385,-8.74902077756027));
#61250=CARTESIAN_POINT('Ctrl Pts',(14.5380167776266,37.0528665436847,-8.76758710574609));
#61251=CARTESIAN_POINT('Ctrl Pts',(13.6262054933649,36.6462732759949,-9.30493187769102));
#61252=CARTESIAN_POINT('Ctrl Pts',(13.921580734334,36.5412824787765,-8.8723756821566));
#61253=CARTESIAN_POINT('Ctrl Pts',(14.4520363909247,36.481645869576,-8.881980084429));
#61254=CARTESIAN_POINT('Ctrl Pts',(13.5947644787342,36.3245972840291,-9.35060353862456));
#61255=CARTESIAN_POINT('Ctrl Pts',(13.8912417590967,36.2402098290348,-8.91955632269035));
#61256=CARTESIAN_POINT('Ctrl Pts',(14.4186898613794,36.192137492116,-8.92557576079275));
#61257=CARTESIAN_POINT('Ctrl Pts',(13.5680981899448,35.9167592473805,-9.38918524120016));
#61258=CARTESIAN_POINT('Ctrl Pts',(13.8655300244092,35.8582683652265,-8.95937275428701));
#61259=CARTESIAN_POINT('Ctrl Pts',(14.3904074352514,35.8250832785829,-8.96240375051597));
#61260=CARTESIAN_POINT('Ctrl Pts',(13.563396609019,35.8349039817843,-9.39597376806161));
#61261=CARTESIAN_POINT('Ctrl Pts',(13.8609990456103,35.781659697871,-8.96637441288284));
#61262=CARTESIAN_POINT('Ctrl Pts',(14.3854209101992,35.7514135434756,-8.96888370787827));
#61263=CARTESIAN_POINT('Ctrl Pts',(13.5573153151024,35.7116818529589,-9.40474423377933));
#61264=CARTESIAN_POINT('Ctrl Pts',(13.8551377884079,35.6663146218422,-8.97542077741386));
#61265=CARTESIAN_POINT('Ctrl Pts',(14.3789710533313,35.6405136334663,-8.97725551630533));
#61266=CARTESIAN_POINT('Ctrl Pts',(13.5554500621166,35.670534598073,-9.40743230188023));
#61267=CARTESIAN_POINT('Ctrl Pts',(13.8533400041568,35.6277987228642,-8.97819335621356));
#61268=CARTESIAN_POINT('Ctrl Pts',(14.376992754778,35.6034811060435,-8.97982139943131));
#61269=CARTESIAN_POINT('Ctrl Pts',(13.5520471598156,35.5880922883365,-9.41233375306736));
#61270=CARTESIAN_POINT('Ctrl Pts',(13.8500601058613,35.5506254644722,-8.98324892780074));
#61271=CARTESIAN_POINT('Ctrl Pts',(14.3733836161508,35.5292830312532,-8.98450005753594));
#61272=CARTESIAN_POINT('Ctrl Pts',(13.5505083952296,35.546760927592,-9.41454874069695));
#61273=CARTESIAN_POINT('Ctrl Pts',(13.8485767969778,35.5119327236365,-8.98553376080348));
#61274=CARTESIAN_POINT('Ctrl Pts',(14.3717515931607,35.4920848085696,-8.98661436391861));
#61275=CARTESIAN_POINT('Ctrl Pts',(13.5436599334148,35.3402581736772,-9.4244027805627));
#61276=CARTESIAN_POINT('Ctrl Pts',(13.8419765765307,35.3186517971435,-8.99569616213354));
#61277=CARTESIAN_POINT('Ctrl Pts',(14.3644880734125,35.3062323400024,-8.99602049284851));
#61278=CARTESIAN_POINT('Ctrl Pts',(13.5408828403502,35.1756098619451,-9.42838755837681));
#61279=CARTESIAN_POINT('Ctrl Pts',(13.8392970574126,35.1644357229371,-8.99980993277378));
#61280=CARTESIAN_POINT('Ctrl Pts',(14.3615426717746,35.1580488673189,-8.99982414466763));
#61281=CARTESIAN_POINT('Ctrl Pts',(13.5405110292838,34.6832904888057,-9.4289215318621));
#61282=CARTESIAN_POINT('Ctrl Pts',(13.8389385644398,34.7034489893202,-9.0003608189815));
#61283=CARTESIAN_POINT('Ctrl Pts',(14.3611483267235,34.7149614551366,-9.00033384633901));
#61284=CARTESIAN_POINT('Ctrl Pts',(13.5508830762733,34.3572427818775,-9.41407821971699));
#61285=CARTESIAN_POINT('Ctrl Pts',(13.8489658444416,34.3977979636559,-8.98500808730318));
#61286=CARTESIAN_POINT('Ctrl Pts',(14.3721489822692,34.4215185342681,-8.98616523030746));
#61287=CARTESIAN_POINT('Ctrl Pts',(13.5919101658448,33.7093421596287,-9.3547463310013));
#61288=CARTESIAN_POINT('Ctrl Pts',(13.8884912540378,33.7915493337399,-8.92382970966888));
#61289=CARTESIAN_POINT('Ctrl Pts',(14.4156625599663,33.8384080055227,-8.92953024469643));
#61290=CARTESIAN_POINT('Ctrl Pts',(13.6225642332904,33.3874892491063,-9.31025704675605));
#61291=CARTESIAN_POINT('Ctrl Pts',(13.918075940792,33.4902694887766,-8.87786426091058));
#61292=CARTESIAN_POINT('Ctrl Pts',(14.4481744486006,33.5487404014116,-8.88706320021167));
#61293=CARTESIAN_POINT('Ctrl Pts',(13.6728215061252,32.9877546659562,-9.23603126196882));
#61294=CARTESIAN_POINT('Ctrl Pts',(13.9662896916563,33.1176686895628,-8.80158654504113));
#61295=CARTESIAN_POINT('Ctrl Pts',(14.5014776139512,33.1889792966578,-8.81621131403715));
#61296=CARTESIAN_POINT('Ctrl Pts',(13.6834694495751,32.9079370045103,-9.22025322157322));
#61297=CARTESIAN_POINT('Ctrl Pts',(13.9765194353422,33.04316387348,-8.78534664166924));
#61298=CARTESIAN_POINT('Ctrl Pts',(14.512770886892,33.1171434052856,-8.8011504571503));
#61299=CARTESIAN_POINT('Ctrl Pts',(13.7003208658972,32.7884041875066,-9.19517860529697));
#61300=CARTESIAN_POINT('Ctrl Pts',(13.9926934407437,32.9316762091749,-8.75955865151019));
#61301=CARTESIAN_POINT('Ctrl Pts',(14.5306436002406,33.0095638758911,-8.77721559591971));
#61302=CARTESIAN_POINT('Ctrl Pts',(13.7060845825789,32.7485921967665,-9.18658577875371));
#61303=CARTESIAN_POINT('Ctrl Pts',(13.9982261245286,32.8945388634974,-8.75071959428219));
#61304=CARTESIAN_POINT('Ctrl Pts',(14.5367566328563,32.9737330861968,-8.76901335232183));
#61305=CARTESIAN_POINT('Ctrl Pts',(13.7179025671362,32.6690327731066,-9.1689291639627));
#61306=CARTESIAN_POINT('Ctrl Pts',(14.0095670511447,32.8203417227802,-8.73256083164095));
#61307=CARTESIAN_POINT('Ctrl Pts',(14.5492908582467,32.9021296088266,-8.75215931076496));
#61308=CARTESIAN_POINT('Ctrl Pts',(13.7239585686921,32.6292758377139,-9.15986274004417));
#61309=CARTESIAN_POINT('Ctrl Pts',(14.0153773261073,32.7832719182194,-8.7232377974293));
#61310=CARTESIAN_POINT('Ctrl Pts',(14.5557138899543,32.866348368934,-8.74350499700366));
#61311=CARTESIAN_POINT('Ctrl Pts',(13.7548626759315,32.431249484037,-9.11349220398879));
#61312=CARTESIAN_POINT('Ctrl Pts',(14.0450499694982,32.5984782080405,-8.67551437811789));
#61313=CARTESIAN_POINT('Ctrl Pts',(14.5884909717086,32.68812466034,-8.69924221182081));
#61314=CARTESIAN_POINT('Ctrl Pts',(13.7816505762543,32.2747815938857,-9.07297363099581));
#61315=CARTESIAN_POINT('Ctrl Pts',(14.0707296805897,32.4527267404774,-8.63386437079738));
#61316=CARTESIAN_POINT('Ctrl Pts',(14.6169023800244,32.5473035669041,-8.66056539224569));
#61317=CARTESIAN_POINT('Ctrl Pts',(13.8676321749174,31.81095992879,-8.94146242624562));
#61318=CARTESIAN_POINT('Ctrl Pts',(14.1531401560041,32.0205075798369,-8.49864781023208));
#61319=CARTESIAN_POINT('Ctrl Pts',(14.7080949798849,32.1298640911792,-8.53503196772206));
#61320=CARTESIAN_POINT('Ctrl Pts',(13.9324346139195,31.5091733617932,-8.84054425749788));
#61321=CARTESIAN_POINT('Ctrl Pts',(14.2151101095553,31.7401896155852,-8.39501754289617));
#61322=CARTESIAN_POINT('Ctrl Pts',(14.7768248366031,31.858256196006,-8.43870098837303));
#61323=CARTESIAN_POINT('Ctrl Pts',(14.0741833838855,30.9193680769779,-8.61308998655124));
#61324=CARTESIAN_POINT('Ctrl Pts',(14.3499236459374,31.1943251121412,-8.16249577569527));
#61325=CARTESIAN_POINT('Ctrl Pts',(14.927164432396,31.3274314704435,-8.22158554640244));
#61326=CARTESIAN_POINT('Ctrl Pts',(14.1511326299876,30.6313511296127,-8.48655143147596));
#61327=CARTESIAN_POINT('Ctrl Pts',(14.4229773435497,30.9284342184197,-8.03318226008555));
#61328=CARTESIAN_POINT('Ctrl Pts',(15.0087772653985,31.0682162329507,-8.10079874377953));
#61329=CARTESIAN_POINT('Ctrl Pts',(14.2533131033264,30.2795421476305,-8.31232202503868));
#61330=CARTESIAN_POINT('Ctrl Pts',(14.5190087190408,30.6063167166278,-7.85672407191655));
#61331=CARTESIAN_POINT('Ctrl Pts',(15.1171504874915,30.7515881692275,-7.93448885616022));
#61332=CARTESIAN_POINT('Ctrl Pts',(14.2740494070183,30.2095920172121,-8.27667110983962));
#61333=CARTESIAN_POINT('Ctrl Pts',(14.5385522750191,30.5420833308275,-7.82050094551189));
#61334=CARTESIAN_POINT('Ctrl Pts',(15.1391435357377,30.6886330556848,-7.9004584371993));
#61335=CARTESIAN_POINT('Ctrl Pts',(14.3055755882552,30.1052800677474,-8.2219796808514));
#61336=CARTESIAN_POINT('Ctrl Pts',(14.5682064898189,30.4464618904594,-7.76502157216377));
#61337=CARTESIAN_POINT('Ctrl Pts',(15.1725803924368,30.5947523069326,-7.84825298230988));
#61338=CARTESIAN_POINT('Ctrl Pts',(14.3161507193771,30.0706249144069,-8.20355330284792));
#61339=CARTESIAN_POINT('Ctrl Pts',(14.5781545712646,30.4146890015269,-7.74632436847072));
#61340=CARTESIAN_POINT('Ctrl Pts',(15.1837964400011,30.5635626708233,-7.83066416704026));
#61341=CARTESIAN_POINT('Ctrl Pts',(14.3373878813408,30.0016749048532,-8.16638028459182));
#61342=CARTESIAN_POINT('Ctrl Pts',(14.5981197517123,30.3515071790422,-7.70862194354184));
#61343=CARTESIAN_POINT('Ctrl Pts',(15.2063207012272,30.5015076660714,-7.79518083140264));
#61344=CARTESIAN_POINT('Ctrl Pts',(14.3480555521587,29.9673613219152,-8.14762387652105));
#61345=CARTESIAN_POINT('Ctrl Pts',(14.6081424657647,30.3200808943631,-7.68960598698859));
#61346=CARTESIAN_POINT('Ctrl Pts',(15.2176348969313,30.4706254432956,-7.77727698747795));
#61347=CARTESIAN_POINT('Ctrl Pts',(14.4016253212505,29.796591116269,-8.05299667723724));
#61348=CARTESIAN_POINT('Ctrl Pts',(14.6585457278825,30.1634387265338,-7.59351316959592));
#61349=CARTESIAN_POINT('Ctrl Pts',(15.2744513150548,30.3169322675397,-7.68695102437855));
#61350=CARTESIAN_POINT('Ctrl Pts',(14.4452205721895,29.6625254514556,-7.97459247489173));
#61351=CARTESIAN_POINT('Ctrl Pts',(14.6993851879577,30.0409902873586,-7.51416748480995));
#61352=CARTESIAN_POINT('Ctrl Pts',(15.3206886998058,30.1962731766416,-7.61211065004841));
#61353=CARTESIAN_POINT('Ctrl Pts',(14.5777133703464,29.2676726547534,-7.73138816583178));
#61354=CARTESIAN_POINT('Ctrl Pts',(14.8234915893807,29.6801465523773,-7.26788478492355));
#61355=CARTESIAN_POINT('Ctrl Pts',(15.4612113551328,29.8409056814626,-7.37996108259175));
#61356=CARTESIAN_POINT('Ctrl Pts',(14.668309347519,29.0142068836985,-7.55861955891375));
#61357=CARTESIAN_POINT('Ctrl Pts',(14.907692286347,29.4503611487385,-7.09386429377839));
#61358=CARTESIAN_POINT('Ctrl Pts',(15.5572979917242,29.6127865022682,-7.21504559587684));
#61359=CARTESIAN_POINT('Ctrl Pts',(14.8515808217713,28.5257802291976,-7.19184092179889));
#61360=CARTESIAN_POINT('Ctrl Pts',(15.0767699379545,29.009999766832,-6.72666722324951));
#61361=CARTESIAN_POINT('Ctrl Pts',(15.7516768131561,29.1732025427066,-6.86493871876546));
#61362=CARTESIAN_POINT('Ctrl Pts',(14.9442617876913,28.2908215774306,-6.99783092564266));
#61363=CARTESIAN_POINT('Ctrl Pts',(15.1617270035886,28.7995023384666,-6.53309448498094));
#61364=CARTESIAN_POINT('Ctrl Pts',(15.8499748005742,28.9617397708295,-6.67974736165878));
#61365=CARTESIAN_POINT('Ctrl Pts',(15.0831691896633,27.9520228746188,-6.6903405523582));
#61366=CARTESIAN_POINT('Ctrl Pts',(15.2875727332987,28.4989406174798,-6.2294513637031));
#61367=CARTESIAN_POINT('Ctrl Pts',(15.997300820026,28.656820960667,-6.38623382970425));
#61368=CARTESIAN_POINT('Ctrl Pts',(15.1294538068838,27.8413684918233,-6.58509205486735));
#61369=CARTESIAN_POINT('Ctrl Pts',(15.3294819925269,28.4007955047577,-6.12542316901587));
#61370=CARTESIAN_POINT('Ctrl Pts',(16.0463905618979,28.5572320234826,-6.28576935691975));
#61371=CARTESIAN_POINT('Ctrl Pts',(15.1871165528599,27.7059137885866,-6.44998867645945));
#61372=CARTESIAN_POINT('Ctrl Pts',(15.3813309114973,28.2813976823567,-5.99268560044396));
#61373=CARTESIAN_POINT('Ctrl Pts',(16.1075480141302,28.4353227996728,-6.15680704431937));
#61374=CARTESIAN_POINT('Ctrl Pts',(15.1986427411563,27.6789586010782,-6.4227826599171));
#61375=CARTESIAN_POINT('Ctrl Pts',(15.3917112172421,28.2575974144608,-5.96590506721411));
#61376=CARTESIAN_POINT('Ctrl Pts',(16.1197727583312,28.4110631327084,-6.13083766552066));
#61377=CARTESIAN_POINT('Ctrl Pts',(15.22161650098,27.6254631882903,-6.36814489211147));
#61378=CARTESIAN_POINT('Ctrl Pts',(15.4123784799737,28.2104073796915,-5.91216422792328));
#61379=CARTESIAN_POINT('Ctrl Pts',(16.1441388650521,28.3629172647956,-6.07868343378511));
#61380=CARTESIAN_POINT('Ctrl Pts',(15.2330706037456,27.5989075417468,-6.34069797064005));
#61381=CARTESIAN_POINT('Ctrl Pts',(15.4226712022193,28.1870046176015,-5.88518855411238));
#61382=CARTESIAN_POINT('Ctrl Pts',(16.1562871548775,28.3390171846542,-6.05248410033579));
#61383=CARTESIAN_POINT('Ctrl Pts',(15.2673288583536,27.5198130564946,-6.25797352384566));
#61384=CARTESIAN_POINT('Ctrl Pts',(15.4534493940906,28.1173044903271,-5.80387679627119));
#61385=CARTESIAN_POINT('Ctrl Pts',(16.1926216640663,28.2678321532352,-5.97351985746979));
#61386=CARTESIAN_POINT('Ctrl Pts',(15.290028934829,27.4678465591937,-6.20231237797931));
#61387=CARTESIAN_POINT('Ctrl Pts',(15.4737789443219,28.0716437659571,-5.7492990645817));
#61388=CARTESIAN_POINT('Ctrl Pts',(16.2166975007587,28.2210623091367,-5.92038876513649));
#61389=CARTESIAN_POINT('Ctrl Pts',(15.4027606748132,27.2117871716814,-5.92145102020388));
#61390=CARTESIAN_POINT('Ctrl Pts',(15.5750557618011,27.8458706821111,-5.47287876127004));
#61391=CARTESIAN_POINT('Ctrl Pts',(16.336261456746,27.9906088770429,-5.65229383850497));
#61392=CARTESIAN_POINT('Ctrl Pts',(15.4904827104974,27.0189801350607,-5.68860317193879));
#61393=CARTESIAN_POINT('Ctrl Pts',(15.6526357170028,27.6784129519233,-5.24631783516924));
#61394=CARTESIAN_POINT('Ctrl Pts',(16.429299971196,27.8170825577775,-5.43002999028148));
#61395=CARTESIAN_POINT('Ctrl Pts',(15.6591637426249,26.656905604576,-5.20632802772958));
#61396=CARTESIAN_POINT('Ctrl Pts',(15.8004769809526,27.3661724733035,-4.7806667702281));
#61397=CARTESIAN_POINT('Ctrl Pts',(16.6082040777263,27.4912155066444,-4.96967645923575));
#61398=CARTESIAN_POINT('Ctrl Pts',(15.740127626065,26.4876389347608,-4.95690180582163));
#61399=CARTESIAN_POINT('Ctrl Pts',(15.8705932694381,27.2218129160782,-4.54154452839877));
#61400=CARTESIAN_POINT('Ctrl Pts',(16.6940748548538,27.3388755168911,-4.73158780209777));
#61401=CARTESIAN_POINT('Ctrl Pts',(15.8934770180544,26.1729335212289,-4.44070731669338));
#61402=CARTESIAN_POINT('Ctrl Pts',(16.0021812140351,26.9553860849679,-4.05065590845588));
#61403=CARTESIAN_POINT('Ctrl Pts',(16.8567181309159,27.0556406687916,-4.2388567198354));
#61404=CARTESIAN_POINT('Ctrl Pts',(15.9658678958422,26.0274910774788,-4.17394304589581));
#61405=CARTESIAN_POINT('Ctrl Pts',(16.063469476959,26.8337655896831,-3.79898706599225));
#61406=CARTESIAN_POINT('Ctrl Pts',(16.9334963265846,26.9247424816998,-3.9842181095779));
#61407=CARTESIAN_POINT('Ctrl Pts',(16.0497732597612,25.8612989242681,-3.82881501888285));
#61408=CARTESIAN_POINT('Ctrl Pts',(16.1335491117151,26.6964316563818,-3.4775371624284));
#61409=CARTESIAN_POINT('Ctrl Pts',(17.022486852709,26.7751695575831,-3.65477773800455));
#61410=CARTESIAN_POINT('Ctrl Pts',(16.0662245959121,25.8288433557414,-3.75920417681785));
#61411=CARTESIAN_POINT('Ctrl Pts',(16.1473132271782,26.6695565389256,-3.41252921961847));
#61412=CARTESIAN_POINT('Ctrl Pts',(17.0399352376671,26.745959548768,-3.58833102853059));
#61413=CARTESIAN_POINT('Ctrl Pts',(16.0903819375245,25.7813551666353,-3.65388920287835));
#61414=CARTESIAN_POINT('Ctrl Pts',(16.1674564707937,26.6303518394139,-3.314450412959));
#61415=CARTESIAN_POINT('Ctrl Pts',(17.0655566573174,26.7032201824222,-3.48780310422709));
#61416=CARTESIAN_POINT('Ctrl Pts',(16.098345616361,25.7657292707521,-3.61864269610625));
#61417=CARTESIAN_POINT('Ctrl Pts',(16.1740922821313,26.6174582718761,-3.28163420148606));
#61418=CARTESIAN_POINT('Ctrl Pts',(17.0740029824056,26.6891568774627,-3.45415871318928));
#61419=CARTESIAN_POINT('Ctrl Pts',(16.1140455830658,25.7349771707284,-3.54807574507184));
#61420=CARTESIAN_POINT('Ctrl Pts',(16.187157008452,26.5921127531103,-3.21599816456815));
#61421=CARTESIAN_POINT('Ctrl Pts',(17.0906544601812,26.6614799900588,-3.38679935442564));
#61422=CARTESIAN_POINT('Ctrl Pts',(16.1217882988379,25.7198383195558,-3.51272748888179));
#61423=CARTESIAN_POINT('Ctrl Pts',(16.1935907787688,26.5796514011833,-3.183153417088));
#61424=CARTESIAN_POINT('Ctrl Pts',(17.0988664304859,26.6478550252466,-3.35305783899775));
#61425=CARTESIAN_POINT('Ctrl Pts',(16.1599613732448,25.6453253627483,-3.33566278782528));
#61426=CARTESIAN_POINT('Ctrl Pts',(16.2253388524004,26.518251457348,-3.01842711386761));
#61427=CARTESIAN_POINT('Ctrl Pts',(17.1393530195516,26.5807933703941,-3.18404154235054));
#61428=CARTESIAN_POINT('Ctrl Pts',(16.1887703626542,25.5894928519857,-3.19297659606595));
#61429=CARTESIAN_POINT('Ctrl Pts',(16.2490907879542,26.4726133412268,-2.88653753270067));
#61430=CARTESIAN_POINT('Ctrl Pts',(17.1699080046339,26.5305441154266,-3.04784109434391));
#61431=CARTESIAN_POINT('Ctrl Pts',(16.2698459579849,25.4332047189377,-2.76182079317166));
#61432=CARTESIAN_POINT('Ctrl Pts',(16.3158320106216,26.3449718406617,-2.48834572470189));
#61433=CARTESIAN_POINT('Ctrl Pts',(17.255897261409,26.3898848090645,-2.63628330557435));
#61434=CARTESIAN_POINT('Ctrl Pts',(16.316765145617,25.3439309463016,-2.47026039537153));
#61435=CARTESIAN_POINT('Ctrl Pts',(16.3537805742651,26.2732399080745,-2.22215610964296));
#61436=CARTESIAN_POINT('Ctrl Pts',(17.3056600298758,26.3095384218259,-2.35797567052832));
#61437=CARTESIAN_POINT('Ctrl Pts',(16.3954028639435,25.1952391193477,-1.87876985450263));
#61438=CARTESIAN_POINT('Ctrl Pts',(16.417121596869,26.154131014951,-1.68483850356858));
#61439=CARTESIAN_POINT('Ctrl Pts',(17.3890636589622,26.1757157908581,-1.79337109958107));
#61440=CARTESIAN_POINT('Ctrl Pts',(16.4271241236573,25.1358193426336,-1.57884042903499));
#61441=CARTESIAN_POINT('Ctrl Pts',(16.4423268469724,26.1071199172671,-1.41447090107595));
#61442=CARTESIAN_POINT('Ctrl Pts',(17.4227074149731,26.1222379977279,-1.50707484923427));
#61443=CARTESIAN_POINT('Ctrl Pts',(16.4624867292185,25.0697740909849,-1.12241556867003));
#61444=CARTESIAN_POINT('Ctrl Pts',(16.4703739907714,26.0549329007231,-1.00461697464686));
#61445=CARTESIAN_POINT('Ctrl Pts',(17.4602132031594,26.0627972771039,-1.07139660369267));
#61446=CARTESIAN_POINT('Ctrl Pts',(16.472236231715,25.0516136052353,-0.96918375449722));
#61447=CARTESIAN_POINT('Ctrl Pts',(16.4780841724723,26.0406189166,-0.867184356346633));
#61448=CARTESIAN_POINT('Ctrl Pts',(17.4705535833765,26.0464528419075,-0.925129882160084));
#61449=CARTESIAN_POINT('Ctrl Pts',(16.483684081477,25.0303119318585,-0.737651684679333));
#61450=CARTESIAN_POINT('Ctrl Pts',(16.4871294638992,26.0238409108057,-0.65980157630425));
#61451=CARTESIAN_POINT('Ctrl Pts',(17.4826952403163,26.0272813376459,-0.704122012867659));
#61452=CARTESIAN_POINT('Ctrl Pts',(16.4869704992073,25.0242017345862,-0.660193474939691));
#61453=CARTESIAN_POINT('Ctrl Pts',(16.4897239001879,26.0190318513568,-0.590448368527771));
#61454=CARTESIAN_POINT('Ctrl Pts',(17.4861808345135,26.0217821608405,-0.630184636034853));
#61455=CARTESIAN_POINT('Ctrl Pts',(16.4904030883612,25.0178224283329,-0.563013510054482));
#61456=CARTESIAN_POINT('Ctrl Pts',(16.49243229442,26.0140133058613,-0.50348874580496));
#61457=CARTESIAN_POINT('Ctrl Pts',(17.4898214587776,26.0160407857062,-0.537421948832318));
#61458=CARTESIAN_POINT('Ctrl Pts',(16.4910558314609,25.0166095003478,-0.543559654133235));
#61459=CARTESIAN_POINT('Ctrl Pts',(16.4929473390123,26.0130590575589,-0.486079274150305));
#61460=CARTESIAN_POINT('Ctrl Pts',(17.4905137619999,26.0149491506782,-0.518852360396683));
#61461=CARTESIAN_POINT('Ctrl Pts',(16.4922934176736,25.0143100694522,-0.504616051390933));
#61462=CARTESIAN_POINT('Ctrl Pts',(16.4939237271056,26.0112502223663,-0.451231779951065));
#61463=CARTESIAN_POINT('Ctrl Pts',(17.4918263532193,26.0128796630442,-0.481678924038814));
#61464=CARTESIAN_POINT('Ctrl Pts',(16.492878650155,25.0132228433094,-0.485110633925368));
#61465=CARTESIAN_POINT('Ctrl Pts',(16.4943853634874,26.0103950931405,-0.433779992803541));
#61466=CARTESIAN_POINT('Ctrl Pts',(17.4924470542556,26.0119011596235,-0.463060117772013));
#61467=CARTESIAN_POINT('Ctrl Pts',(16.4945258261512,25.0101630686332,-0.4267689702364));
#61468=CARTESIAN_POINT('Ctrl Pts',(16.495684601932,26.00798859576,-0.381582487394922));
#61469=CARTESIAN_POINT('Ctrl Pts',(17.4941940588796,26.0091473627552,-0.407370351815588));
#61470=CARTESIAN_POINT('Ctrl Pts',(16.4954853336232,25.0083811132544,-0.387907202711105));
#61471=CARTESIAN_POINT('Ctrl Pts',(16.4964411138925,26.0065876292943,-0.346823188777901));
#61472=CARTESIAN_POINT('Ctrl Pts',(17.4952117181403,26.0075436030163,-0.370275030893979));
#61473=CARTESIAN_POINT('Ctrl Pts',(16.4995936624279,25.0007522824497,-0.193760702128921));
#61474=CARTESIAN_POINT('Ctrl Pts',(16.4996807717234,26.0005888276808,-0.173146702174422));
#61475=CARTESIAN_POINT('Ctrl Pts',(17.4995690360396,26.0006776561714,-0.184953384322929));
#61476=CARTESIAN_POINT('Ctrl Pts',(16.5006753927425,24.9987456794828,-0.0389627034907101));
#61477=CARTESIAN_POINT('Ctrl Pts',(16.5005316011594,25.9990147346703,-0.0348510197095155));
#61478=CARTESIAN_POINT('Ctrl Pts',(17.5007163254734,25.9988717134746,-0.037191668888471));
#61479=CARTESIAN_POINT('Ctrl Pts',(16.4985185160909,25.0027491746321,0.269616919228709));
#61480=CARTESIAN_POINT('Ctrl Pts',(16.4988321329034,26.0021605183102,0.241013621938643));
#61481=CARTESIAN_POINT('Ctrl Pts',(17.498428729471,26.0024748589104,0.257361586454653));
#61482=CARTESIAN_POINT('Ctrl Pts',(16.4952798552968,25.0087594435861,0.42339852392335));
#61483=CARTESIAN_POINT('Ctrl Pts',(16.4962832364797,26.0068778358239,0.378456519338701));
#61484=CARTESIAN_POINT('Ctrl Pts',(17.4949937865805,26.0078841002541,0.404153107768947));
#61485=CARTESIAN_POINT('Ctrl Pts',(16.4845588751127,25.0286833763451,0.729960620582834));
#61486=CARTESIAN_POINT('Ctrl Pts',(16.4878225611123,26.0225547920612,0.65283101053216));
#61487=CARTESIAN_POINT('Ctrl Pts',(17.4836230517336,26.0258156379645,0.696780543053585));
#61488=CARTESIAN_POINT('Ctrl Pts',(16.4770765097712,25.042597132783,0.882741101116753));
#61489=CARTESIAN_POINT('Ctrl Pts',(16.4819182165634,26.0335005894375,0.789640705789399));
#61490=CARTESIAN_POINT('Ctrl Pts',(17.4756872107313,26.0383380173717,0.842616446032084));
#61491=CARTESIAN_POINT('Ctrl Pts',(16.457933564706,25.0782732358425,1.18730995963222));
#61492=CARTESIAN_POINT('Ctrl Pts',(16.4667568417188,26.0616602772347,1.06294377615386));
#61493=CARTESIAN_POINT('Ctrl Pts',(17.4553840901105,26.0704465068189,1.1333412453569));
#61494=CARTESIAN_POINT('Ctrl Pts',(16.4462729445412,25.1000356045573,1.33909833326507));
#61495=CARTESIAN_POINT('Ctrl Pts',(16.457512962125,26.0788495239333,1.19931940286108));
#61496=CARTESIAN_POINT('Ctrl Pts',(17.4430167673428,26.0900326366225,1.27823013746166));
#61497=CARTESIAN_POINT('Ctrl Pts',(16.4188289862862,25.1514109395644,1.64168597230913));
#61498=CARTESIAN_POINT('Ctrl Pts',(16.4356580866948,26.1195950064352,1.4719247367756));
#61499=CARTESIAN_POINT('Ctrl Pts',(17.4139095429865,26.1362704333346,1.56706377336382));
#61500=CARTESIAN_POINT('Ctrl Pts',(16.4030456111901,25.1810238589603,1.7924852401837));
#61501=CARTESIAN_POINT('Ctrl Pts',(16.4230656732971,26.1431161224906,1.60804089841558));
#61502=CARTESIAN_POINT('Ctrl Pts',(17.3971696019414,26.1629220581204,1.7110085193938));
#61503=CARTESIAN_POINT('Ctrl Pts',(16.3763135366034,25.231375580585,2.01794006740895));
#61504=CARTESIAN_POINT('Ctrl Pts',(16.4016055889564,26.1833366410978,1.81239942992283));
#61505=CARTESIAN_POINT('Ctrl Pts',(17.3688174054951,26.2082386029367,1.92621538597846));
#61506=CARTESIAN_POINT('Ctrl Pts',(16.3668932777758,25.2491486628916,2.09296761713974));
#61507=CARTESIAN_POINT('Ctrl Pts',(16.3940375747528,26.1975406923544,1.88043508573692));
#61508=CARTESIAN_POINT('Ctrl Pts',(17.3588262232113,26.2242343754568,1.99783258786826));
#61509=CARTESIAN_POINT('Ctrl Pts',(16.3520023700009,25.2773017719863,2.20532214078148));
#61510=CARTESIAN_POINT('Ctrl Pts',(16.3820388971085,26.2201011771275,1.98254008226397));
#61511=CARTESIAN_POINT('Ctrl Pts',(17.3430328383105,26.2495721710511,2.10508008086908));
#61512=CARTESIAN_POINT('Ctrl Pts',(16.3469119771516,25.2869350853555,2.24274251216562));
#61513=CARTESIAN_POINT('Ctrl Pts',(16.3779351975318,26.2278235718406,2.01655526539809));
#61514=CARTESIAN_POINT('Ctrl Pts',(17.3376339375129,26.2582421522511,2.1407995239869));
#61515=CARTESIAN_POINT('Ctrl Pts',(16.3364782736115,25.3067015799831,2.31752082632262));
#61516=CARTESIAN_POINT('Ctrl Pts',(16.369513853826,26.2436857621179,2.0845855843958));
#61517=CARTESIAN_POINT('Ctrl Pts',(17.3265678897919,26.2760319955966,2.21217881933827));
#61518=CARTESIAN_POINT('Ctrl Pts',(16.3311312276683,25.3168418552601,2.35490405296875));
#61519=CARTESIAN_POINT('Ctrl Pts',(16.3651936132304,26.2518304450527,2.11862215055674));
#61520=CARTESIAN_POINT('Ctrl Pts',(17.3208967811602,26.285158242412,2.24786280615268));
#61521=CARTESIAN_POINT('Ctrl Pts',(16.2819566384181,25.4102034773501,2.69049912871399));
#61522=CARTESIAN_POINT('Ctrl Pts',(16.3255665769557,26.3266105865415,2.42325772140721));
#61523=CARTESIAN_POINT('Ctrl Pts',(17.2687419212362,26.3691836940896,2.56820353924912));
#61524=CARTESIAN_POINT('Ctrl Pts',(16.2309920113021,25.5076777154244,2.9814187974019));
#61525=CARTESIAN_POINT('Ctrl Pts',(16.2841214219777,26.4053051020533,2.6899166416278));
#61526=CARTESIAN_POINT('Ctrl Pts',(17.2146886258162,26.4569103521462,2.84589917037985));
#61527=CARTESIAN_POINT('Ctrl Pts',(16.1736472161052,25.6188908313694,3.26544571674037));
#61528=CARTESIAN_POINT('Ctrl Pts',(16.2365230528882,26.4968270314871,2.95402066052848));
#61529=CARTESIAN_POINT('Ctrl Pts',(17.1538683056082,26.5570022944821,3.11701616046811));
#61530=CARTESIAN_POINT('Ctrl Pts',(16.4590359785375,20.1091944935103,0.023011592823693));
#61531=CARTESIAN_POINT('Ctrl Pts',(16.4271965341628,20.1902603108686,1.05278036905647));
#61532=CARTESIAN_POINT('Ctrl Pts',(17.3953642409772,20.5502649459156,1.02026723798077));
#61533=CARTESIAN_POINT('Ctrl Pts',(16.5316577284859,19.9154749454276,0.0395707565384078));
#61534=CARTESIAN_POINT('Ctrl Pts',(16.4879246572657,20.0254557281703,1.07950524961033));
#61535=CARTESIAN_POINT('Ctrl Pts',(17.4679845765535,20.3888322238513,1.03484672596902));
#61536=CARTESIAN_POINT('Ctrl Pts',(16.6034030152266,19.724010227151,0.0649122476643638));
#61537=CARTESIAN_POINT('Ctrl Pts',(16.5465862722544,19.8645616579358,1.1140637205542));
#61538=CARTESIAN_POINT('Ctrl Pts',(17.5397268922733,20.2292780573011,1.05715075962855));
#61539=CARTESIAN_POINT('Ctrl Pts',(16.744970961061,19.3454312478812,0.132696775849498));
#61540=CARTESIAN_POINT('Ctrl Pts',(16.6602111583784,19.5489225084427,1.19790262588923));
#61541=CARTESIAN_POINT('Ctrl Pts',(17.6812725629732,19.9137955745397,1.11677044650688));
#61542=CARTESIAN_POINT('Ctrl Pts',(16.8147959023614,19.15831105953,0.175140612617222));
#61543=CARTESIAN_POINT('Ctrl Pts',(16.7151746590028,19.3941162803857,1.24743104684572));
#61544=CARTESIAN_POINT('Ctrl Pts',(17.7510782956021,19.757862084349,1.15408688832136));
#61545=CARTESIAN_POINT('Ctrl Pts',(16.9521986924116,18.78829106961,0.277198432090005));
#61546=CARTESIAN_POINT('Ctrl Pts',(16.8209509865544,19.0909503211262,1.36068099990159));
#61547=CARTESIAN_POINT('Ctrl Pts',(17.8884066526975,19.4495120925816,1.24376538253356));
#61548=CARTESIAN_POINT('Ctrl Pts',(17.0197775730774,18.6053910460792,0.33681026323465));
#61549=CARTESIAN_POINT('Ctrl Pts',(16.871742873146,18.9425660229543,1.42466616590782));
#61550=CARTESIAN_POINT('Ctrl Pts',(17.9559303491669,19.2970954065821,1.29612559894816));
#61551=CARTESIAN_POINT('Ctrl Pts',(17.1190709679907,18.3341847189676,0.439566509587872));
#61552=CARTESIAN_POINT('Ctrl Pts',(16.9440617016846,18.7260133044026,1.53064143694302));
#61553=CARTESIAN_POINT('Ctrl Pts',(18.0550933334177,19.0710901337005,1.38633699361548));
#61554=CARTESIAN_POINT('Ctrl Pts',(17.1518213623139,18.2443072781152,0.476046143457168));
#61555=CARTESIAN_POINT('Ctrl Pts',(16.9676606711903,18.6543970536208,1.5678998215709));
#61556=CARTESIAN_POINT('Ctrl Pts',(18.0877922559576,18.9961922665532,1.41835657614485));
#61557=CARTESIAN_POINT('Ctrl Pts',(17.2003606779556,18.1102824927287,0.53420980976954));
#61558=CARTESIAN_POINT('Ctrl Pts',(17.002019006833,18.5485258471271,1.62629031883017));
#61559=CARTESIAN_POINT('Ctrl Pts',(18.1362391230538,18.8845049451975,1.46939781628312));
#61560=CARTESIAN_POINT('Ctrl Pts',(17.2164426130913,18.0657395120991,0.554172071041801));
#61561=CARTESIAN_POINT('Ctrl Pts',(17.0133328640638,18.5133846587384,1.64623854105085));
#61562=CARTESIAN_POINT('Ctrl Pts',(18.1522876971816,18.8473857948172,1.48691383709229));
#61563=CARTESIAN_POINT('Ctrl Pts',(17.2483983308808,17.9769188381794,0.595266832712274));
#61564=CARTESIAN_POINT('Ctrl Pts',(17.0356241199857,18.4435548304955,1.6870145481646));
#61565=CARTESIAN_POINT('Ctrl Pts',(18.1841709974958,18.7733685663955,1.5229689425839));
#61566=CARTESIAN_POINT('Ctrl Pts',(17.2642156130721,17.9327979927603,0.616327327634305));
#61567=CARTESIAN_POINT('Ctrl Pts',(17.0465605940939,18.408991549976,1.70777441346281));
#61568=CARTESIAN_POINT('Ctrl Pts',(18.199949347906,18.7366011952906,1.54144485057487));
#61569=CARTESIAN_POINT('Ctrl Pts',(17.3423810485448,17.7139016011755,0.724053234204549));
#61570=CARTESIAN_POINT('Ctrl Pts',(17.1004716187916,18.2370235580736,1.81391718075492));
#61571=CARTESIAN_POINT('Ctrl Pts',(18.2779055045962,18.5541875356366,1.63594086850669));
#61572=CARTESIAN_POINT('Ctrl Pts',(17.4020798909505,17.543948296683,0.818101992014677));
#61573=CARTESIAN_POINT('Ctrl Pts',(17.1397482995283,18.1064705157127,1.90384392042449));
#61574=CARTESIAN_POINT('Ctrl Pts',(18.3373901375251,18.4125597820159,1.71840946033613));
#61575=CARTESIAN_POINT('Ctrl Pts',(17.5151946090821,17.2141267403257,1.02191071411103));
#61576=CARTESIAN_POINT('Ctrl Pts',(17.2111122741965,17.8569602745908,2.09328504050278));
#61577=CARTESIAN_POINT('Ctrl Pts',(18.4499480234508,18.1377084848054,1.89705572630751));
#61578=CARTESIAN_POINT('Ctrl Pts',(17.5686124281954,17.0542582812458,1.13166952369181));
#61579=CARTESIAN_POINT('Ctrl Pts',(17.2430573179698,17.7382644719926,2.19292283456572));
#61580=CARTESIAN_POINT('Ctrl Pts',(18.5030233178418,18.0044847693226,1.99323241936555));
#61581=CARTESIAN_POINT('Ctrl Pts',(17.6682752987396,16.7446855460758,1.36740039352683));
#61582=CARTESIAN_POINT('Ctrl Pts',(17.2994473380135,17.5122427624059,2.4008695734411));
#61583=CARTESIAN_POINT('Ctrl Pts',(18.6018307891431,17.7465074894261,2.19972574330706));
#61584=CARTESIAN_POINT('Ctrl Pts',(17.7145243522751,16.594979202804,1.49336803899043));
#61585=CARTESIAN_POINT('Ctrl Pts',(17.3237386272113,17.4052155445271,2.50922972451975));
#61586=CARTESIAN_POINT('Ctrl Pts',(18.6475671361265,17.6217522041873,2.31003851895677));
#61587=CARTESIAN_POINT('Ctrl Pts',(17.7670709494956,16.4144680486652,1.66165226591233));
#61588=CARTESIAN_POINT('Ctrl Pts',(17.3490690346078,17.2791176138107,2.64887744438743));
#61589=CARTESIAN_POINT('Ctrl Pts',(18.6993332924172,17.4713262417462,2.45736893303087));
#61590=CARTESIAN_POINT('Ctrl Pts',(17.7773159546806,16.3786978765719,1.69585204953799));
#61591=CARTESIAN_POINT('Ctrl Pts',(17.3539160552592,17.2541015552392,2.6772316437113));
#61592=CARTESIAN_POINT('Ctrl Pts',(18.7094151971177,17.4415177652829,2.48730848910089));
#61593=CARTESIAN_POINT('Ctrl Pts',(17.7922687108733,16.325548896176,1.74798467850413));
#61594=CARTESIAN_POINT('Ctrl Pts',(17.3608049212334,17.2171380154186,2.72009853858696));
#61595=CARTESIAN_POINT('Ctrl Pts',(18.7241120427853,17.3972269480623,2.53294423139505));
#61596=CARTESIAN_POINT('Ctrl Pts',(17.7971838211124,16.3079169628778,1.76550107196727));
#61597=CARTESIAN_POINT('Ctrl Pts',(17.36304058461,17.2048927323774,2.73446477736455));
#61598=CARTESIAN_POINT('Ctrl Pts',(18.7289399725856,17.3825336704678,2.54827723569099));
#61599=CARTESIAN_POINT('Ctrl Pts',(17.8068724998976,16.2728234255862,1.80081496910026));
#61600=CARTESIAN_POINT('Ctrl Pts',(17.3673860983665,17.1805763928498,2.76332308063254));
#61601=CARTESIAN_POINT('Ctrl Pts',(18.7384504053793,17.3532890558995,2.57918840373732));
#61602=CARTESIAN_POINT('Ctrl Pts',(17.8116492768538,16.2553497222102,1.81862527130614));
#61603=CARTESIAN_POINT('Ctrl Pts',(17.369496984659,17.1684977611069,2.77782524857301));
#61604=CARTESIAN_POINT('Ctrl Pts',(18.7431360490359,17.338727636486,2.59477776943123));
#61605=CARTESIAN_POINT('Ctrl Pts',(17.835091711741,16.1687058794947,1.90808130716663));
#61606=CARTESIAN_POINT('Ctrl Pts',(17.3797315284296,17.1085643067264,2.85061578024528));
#61607=CARTESIAN_POINT('Ctrl Pts',(18.7661143769998,17.2665244342873,2.67307644354688));
#61608=CARTESIAN_POINT('Ctrl Pts',(17.8524871153197,16.1015191310896,1.9811249412165));
#61609=CARTESIAN_POINT('Ctrl Pts',(17.3867870687763,17.0626954637632,2.90902060208184));
#61610=CARTESIAN_POINT('Ctrl Pts',(18.7831105947819,17.2105354772255,2.73700263540102));
#61611=CARTESIAN_POINT('Ctrl Pts',(17.9004839498672,15.9062454260188,2.20464101652785));
#61612=CARTESIAN_POINT('Ctrl Pts',(17.4049013625984,16.9298674264324,3.08585335220375));
#61613=CARTESIAN_POINT('Ctrl Pts',(18.8298189469103,17.047807389685,2.93259943046952));
#61614=CARTESIAN_POINT('Ctrl Pts',(17.9269071636239,15.7844281968184,2.35948710426806));
#61615=CARTESIAN_POINT('Ctrl Pts',(17.4126737657556,16.8489775129713,3.2043514593929));
#61616=CARTESIAN_POINT('Ctrl Pts',(18.8552622062664,16.9462930322008,3.06807804330981));
#61617=CARTESIAN_POINT('Ctrl Pts',(17.9575346714358,15.614170143894,2.60051765040973));
#61618=CARTESIAN_POINT('Ctrl Pts',(17.4186455070294,16.7368756953305,3.38350954430276));
#61619=CARTESIAN_POINT('Ctrl Pts',(18.8842055180459,16.8044113211377,3.27893177721889));
#61620=CARTESIAN_POINT('Ctrl Pts',(17.9662399299004,15.5594996501156,2.68232428765808));
#61621=CARTESIAN_POINT('Ctrl Pts',(17.4196743615776,16.7009605910879,3.44366696183719));
#61622=CARTESIAN_POINT('Ctrl Pts',(18.8923136078949,16.7588525765766,3.35049154672856));
#61623=CARTESIAN_POINT('Ctrl Pts',(17.9804993640783,15.4543610677294,2.8489005711619));
#61624=CARTESIAN_POINT('Ctrl Pts',(17.4198882444818,16.6319204969828,3.5646923241279));
#61625=CARTESIAN_POINT('Ctrl Pts',(18.9053007953748,16.6712370909416,3.49619525754758));
#61626=CARTESIAN_POINT('Ctrl Pts',(17.986053674335,15.4038928976034,2.93367015391985));
#61627=CARTESIAN_POINT('Ctrl Pts',(17.4190642517473,16.5988418210516,3.625506476283));
#61628=CARTESIAN_POINT('Ctrl Pts',(18.9101800346347,16.629180282881,3.57033914248333));
#61629=CARTESIAN_POINT('Ctrl Pts',(17.993840269328,15.3072328393525,3.10623404351813));
#61630=CARTESIAN_POINT('Ctrl Pts',(17.4156152191415,16.5352552788028,3.74801297800127));
#61631=CARTESIAN_POINT('Ctrl Pts',(18.9165314277074,16.5486302338962,3.7212669995102));
#61632=CARTESIAN_POINT('Ctrl Pts',(17.9960727385546,15.2610408122494,3.19402824639033));
#61633=CARTESIAN_POINT('Ctrl Pts',(17.4129850963717,16.5047904497612,3.80964503225668));
#61634=CARTESIAN_POINT('Ctrl Pts',(18.9180037747939,16.5101368784898,3.79805087941676));
#61635=CARTESIAN_POINT('Ctrl Pts',(17.9967772718942,15.1950447530921,3.32805498011324));
#61636=CARTESIAN_POINT('Ctrl Pts',(17.4076993677159,16.4609072677679,3.90287558319925));
#61637=CARTESIAN_POINT('Ctrl Pts',(18.9174982244806,16.4551401620879,3.91526698385196));
#61638=CARTESIAN_POINT('Ctrl Pts',(17.996571056543,15.1735921344216,3.37312636457799));
#61639=CARTESIAN_POINT('Ctrl Pts',(17.4057109865791,16.4465714494365,3.93411056442095));
#61640=CARTESIAN_POINT('Ctrl Pts',(18.916876930227,16.4372629798948,3.95468481362002));
#61641=CARTESIAN_POINT('Ctrl Pts',(17.9952480179863,15.131814858786,3.46403649967884));
#61642=CARTESIAN_POINT('Ctrl Pts',(17.4012829714188,16.4184858944737,3.99688191374779));
#61643=CARTESIAN_POINT('Ctrl Pts',(18.9146995251255,16.4024485837588,4.03419118394147));
#61644=CARTESIAN_POINT('Ctrl Pts',(17.9941350799946,15.1116102126343,3.50961367764491));
#61645=CARTESIAN_POINT('Ctrl Pts',(17.3988562915068,16.4048217541979,4.02822857708018));
#61646=CARTESIAN_POINT('Ctrl Pts',(18.9131497582954,16.3856113784195,4.07405096435664));
#61647=CARTESIAN_POINT('Ctrl Pts',(17.9894447446815,15.0530145947759,3.64670240077642));
#61648=CARTESIAN_POINT('Ctrl Pts',(17.3909482301197,16.3648708917027,4.12228170075606));
#61649=CARTESIAN_POINT('Ctrl Pts',(18.907119450644,16.3367816971689,4.19394263224871));
#61650=CARTESIAN_POINT('Ctrl Pts',(17.98451648757,15.0166405335387,3.73857085294315));
#61651=CARTESIAN_POINT('Ctrl Pts',(17.3848513030829,16.3396865216089,4.18485667628148));
#61652=CARTESIAN_POINT('Ctrl Pts',(18.9012585754435,16.3064699791306,4.27428659583135));
#61653=CARTESIAN_POINT('Ctrl Pts',(17.9710553602389,14.9491283812115,3.92321824386789));
#61654=CARTESIAN_POINT('Ctrl Pts',(17.3710242878969,16.2918598145745,4.31030626208985));
#61655=CARTESIAN_POINT('Ctrl Pts',(18.8858504484229,16.2502098524752,4.4357735571199));
#61656=CARTESIAN_POINT('Ctrl Pts',(17.9625224589627,14.9179904470399,4.01599722125423));
#61657=CARTESIAN_POINT('Ctrl Pts',(17.3633020844883,16.2692492133529,4.37310190417037));
#61658=CARTESIAN_POINT('Ctrl Pts',(18.8763031679861,16.2242615737717,4.51691658730071));
#61659=CARTESIAN_POINT('Ctrl Pts',(17.9418292246949,14.860850901726,4.20243289837371));
#61660=CARTESIAN_POINT('Ctrl Pts',(17.3461928936806,16.2263988612261,4.49936190571207));
#61661=CARTESIAN_POINT('Ctrl Pts',(18.8534959064239,16.1766452861806,4.67997604966665));
#61662=CARTESIAN_POINT('Ctrl Pts',(17.9296688867409,14.8348493881004,4.29608962464074));
#61663=CARTESIAN_POINT('Ctrl Pts',(17.3368180429497,16.2061847160273,4.56274563312786));
#61664=CARTESIAN_POINT('Ctrl Pts',(18.8402359231131,16.1549773580455,4.76189250375669));
#61665=CARTESIAN_POINT('Ctrl Pts',(17.9016776590665,14.7879225853875,4.48425565734379));
#61666=CARTESIAN_POINT('Ctrl Pts',(17.3163113352066,16.1680417453508,4.69056595942866));
#61667=CARTESIAN_POINT('Ctrl Pts',(18.8099562188662,16.1158716891751,4.92647998774823));
#61668=CARTESIAN_POINT('Ctrl Pts',(17.8858467886268,14.7669973432221,4.57876498035805));
#61669=CARTESIAN_POINT('Ctrl Pts',(17.3051961155725,16.1501327045764,4.75491912530884));
#61670=CARTESIAN_POINT('Ctrl Pts',(18.7929365204291,16.0984339873699,5.00915103077204));
#61671=CARTESIAN_POINT('Ctrl Pts',(17.8504508492249,14.7302004084719,4.76861805064328));
#61672=CARTESIAN_POINT('Ctrl Pts',(17.2810567878328,16.1165998124299,4.88506415276689));
#61673=CARTESIAN_POINT('Ctrl Pts',(18.7550693416422,16.0677698750224,5.17523515457135));
#61674=CARTESIAN_POINT('Ctrl Pts',(17.8308858240908,14.7143287162555,4.86396180571914));
#61675=CARTESIAN_POINT('Ctrl Pts',(17.2680543324973,16.1009898507806,4.95076863804019));
#61676=CARTESIAN_POINT('Ctrl Pts',(18.7342219089113,16.0545434649538,5.25864824062171));
#61677=CARTESIAN_POINT('Ctrl Pts',(17.8040424705567,14.697656351034,4.98365580793276));
#61678=CARTESIAN_POINT('Ctrl Pts',(17.2504475689671,16.0829273849491,5.03417381304885));
#61679=CARTESIAN_POINT('Ctrl Pts',(18.7057139554211,16.0406498271644,5.3633742964716));
#61680=CARTESIAN_POINT('Ctrl Pts',(17.7985497183264,14.6944778990153,5.00764015025094));
#61681=CARTESIAN_POINT('Ctrl Pts',(17.2468638075045,16.0793928106346,5.05089349630703));
#61682=CARTESIAN_POINT('Ctrl Pts',(18.6998849211899,16.0380011170706,5.38435984131314));
#61683=CARTESIAN_POINT('Ctrl Pts',(17.7873487605497,14.6884515573287,5.05555431987132));
#61684=CARTESIAN_POINT('Ctrl Pts',(17.2395772081921,16.0724898364934,5.08437341715332));
#61685=CARTESIAN_POINT('Ctrl Pts',(18.6880066539913,16.0329791658634,5.42628425816146));
#61686=CARTESIAN_POINT('Ctrl Pts',(17.7816428554264,14.6856044510824,5.07947529630174));
#61687=CARTESIAN_POINT('Ctrl Pts',(17.2358762620874,16.0691226166571,5.10112607282942));
#61688=CARTESIAN_POINT('Ctrl Pts',(18.6819598521156,16.0306065771309,5.44721538470061));
#61689=CARTESIAN_POINT('Ctrl Pts',(17.7642114493362,14.677554866839,5.15113069843371));
#61690=CARTESIAN_POINT('Ctrl Pts',(17.2246034389948,16.0592795749159,5.15140072438751));
#61691=CARTESIAN_POINT('Ctrl Pts',(18.6634990155104,16.0238985905457,5.50991628113862));
#61692=CARTESIAN_POINT('Ctrl Pts',(17.7521723027935,14.6728440185356,5.19875761220163));
#61693=CARTESIAN_POINT('Ctrl Pts',(17.2168497938318,16.0530497158324,5.18499631250327));
#61694=CARTESIAN_POINT('Ctrl Pts',(18.650764595348,16.0199728832643,5.55159358109326));
#61695=CARTESIAN_POINT('Ctrl Pts',(17.7148192143042,14.6606304582502,5.34121409400244));
#61696=CARTESIAN_POINT('Ctrl Pts',(17.1928855233917,16.0353963778912,5.28589380831356));
#61697=CARTESIAN_POINT('Ctrl Pts',(18.6112985955892,16.009794916877,5.67626117295854));
#61698=CARTESIAN_POINT('Ctrl Pts',(17.6882702666085,14.6550452532322,5.43561962007091));
#61699=CARTESIAN_POINT('Ctrl Pts',(17.1759265998257,16.0249547390621,5.35353548466019));
#61700=CARTESIAN_POINT('Ctrl Pts',(18.5833049272282,16.0051405787367,5.75888734807405));
#61701=CARTESIAN_POINT('Ctrl Pts',(17.6319631314318,14.6487737552932,5.62332507276344));
#61702=CARTESIAN_POINT('Ctrl Pts',(17.1398746928238,16.0068264974026,5.48975029904835));
#61703=CARTESIAN_POINT('Ctrl Pts',(18.5240352467465,15.9999143310151,5.92319341230171));
#61704=CARTESIAN_POINT('Ctrl Pts',(17.6022048520147,14.6480876974245,5.71662496962117));
#61705=CARTESIAN_POINT('Ctrl Pts',(17.1208140006137,15.9991314162458,5.55824749460516));
#61706=CARTESIAN_POINT('Ctrl Pts',(18.4927591427342,15.9993426156233,6.0048732741055));
#61707=CARTESIAN_POINT('Ctrl Pts',(17.5082133108841,14.6531225803452,5.99489420103241));
#61708=CARTESIAN_POINT('Ctrl Pts',(17.0604058020015,15.9804134812741,5.76457570444654));
#61709=CARTESIAN_POINT('Ctrl Pts',(18.3941027932187,16.0035383520529,6.24852182898731));
#61710=CARTESIAN_POINT('Ctrl Pts',(17.4392709397385,14.6659198618794,6.17823569450356));
#61711=CARTESIAN_POINT('Ctrl Pts',(17.0156031963545,15.9734934665474,5.90440046372606));
#61712=CARTESIAN_POINT('Ctrl Pts',(18.3219022319539,16.0142027526621,6.40910175786889));
#61713=CARTESIAN_POINT('Ctrl Pts',(17.345440413842,14.6931450787676,6.40474884759392));
#61714=CARTESIAN_POINT('Ctrl Pts',(16.9524570790435,15.9727945398665,6.08359523647655));
#61715=CARTESIAN_POINT('Ctrl Pts',(18.2238061082988,16.0368904336869,6.60756858482206));
#61716=CARTESIAN_POINT('Ctrl Pts',(17.3262910773468,14.6991528841241,6.44991808472345));
#61717=CARTESIAN_POINT('Ctrl Pts',(16.9395918709281,15.9730468738618,6.11932400679305));
#61718=CARTESIAN_POINT('Ctrl Pts',(18.2037939992296,16.0418969380489,6.64714886601801));
#61719=CARTESIAN_POINT('Ctrl Pts',(17.2969942022215,14.7090018589149,6.51747218845496));
#61720=CARTESIAN_POINT('Ctrl Pts',(16.91976284683,15.9740345866775,6.17319709455581));
#61721=CARTESIAN_POINT('Ctrl Pts',(18.1731883149322,16.0501044171085,6.70635021441229));
#61722=CARTESIAN_POINT('Ctrl Pts',(17.2871349117687,14.7124239673732,6.53995233222814));
#61723=CARTESIAN_POINT('Ctrl Pts',(16.9130785924152,15.9744641578401,6.19116453544277));
#61724=CARTESIAN_POINT('Ctrl Pts',(18.1628903970445,16.0529561740322,6.72605178979342));
#61725=CARTESIAN_POINT('Ctrl Pts',(17.2672775991108,14.7195269072644,6.58473078371382));
#61726=CARTESIAN_POINT('Ctrl Pts',(16.8995745934923,15.9755246869321,6.22707698730837));
#61727=CARTESIAN_POINT('Ctrl Pts',(18.142153205609,16.0588752908132,6.76529760601478));
#61728=CARTESIAN_POINT('Ctrl Pts',(17.2572733605126,14.7232097949335,6.6070435056052));
#61729=CARTESIAN_POINT('Ctrl Pts',(16.8927512736487,15.9761553190149,6.24503272312702));
#61730=CARTESIAN_POINT('Ctrl Pts',(18.1317074372765,16.0619443636701,6.78485447850158));
#61731=CARTESIAN_POINT('Ctrl Pts',(17.2068788594663,14.7422717582395,6.7182295014901));
#61732=CARTESIAN_POINT('Ctrl Pts',(16.8583978923929,15.9798004972284,6.33448629417914));
#61733=CARTESIAN_POINT('Ctrl Pts',(18.0790973420651,16.0778293335824,6.88231301093151));
#61734=CARTESIAN_POINT('Ctrl Pts',(17.1653693899747,14.7595916588526,6.80597077954413));
#61735=CARTESIAN_POINT('Ctrl Pts',(16.8296806545478,15.9843227083645,6.40628853128631));
#61736=CARTESIAN_POINT('Ctrl Pts',(18.0357899748907,16.0922625833738,6.95923792167927));
#61737=CARTESIAN_POINT('Ctrl Pts',(17.0374181157849,14.8174391690287,7.06573918620837));
#61738=CARTESIAN_POINT('Ctrl Pts',(16.7403906073823,16.0027254972849,6.62060912535184));
#61739=CARTESIAN_POINT('Ctrl Pts',(17.9023688442237,16.1404688428348,7.18703525486854));
#61740=CARTESIAN_POINT('Ctrl Pts',(16.9475600453929,14.8638381887821,7.2343187616815));
#61741=CARTESIAN_POINT('Ctrl Pts',(16.676004214839,16.0214069152903,6.76401708988705));
#61742=CARTESIAN_POINT('Ctrl Pts',(17.8087626986413,16.1791346915417,7.33493716527047));
#61743=CARTESIAN_POINT('Ctrl Pts',(16.7593871717187,14.9710453070472,7.56294675844479));
#61744=CARTESIAN_POINT('Ctrl Pts',(16.5372832254195,16.072302724032,7.05030038222382));
#61745=CARTESIAN_POINT('Ctrl Pts',(17.6128899340039,16.2684739576301,7.62341025865086));
#61746=CARTESIAN_POINT('Ctrl Pts',(16.66107044624,15.0318575828356,7.72299307498027));
#61747=CARTESIAN_POINT('Ctrl Pts',(16.4632621472069,16.1041974200547,7.19296322794295));
#61748=CARTESIAN_POINT('Ctrl Pts',(17.5106213830702,16.3191508534299,7.76397957999253));
#61749=CARTESIAN_POINT('Ctrl Pts',(16.5331785751374,15.1163977359375,7.91798996938649));
#61750=CARTESIAN_POINT('Ctrl Pts',(16.363683758477,16.1530692164372,7.37184321612237));
#61751=CARTESIAN_POINT('Ctrl Pts',(17.3776610168937,16.3896009813358,7.93535376144086));
#61752=CARTESIAN_POINT('Ctrl Pts',(16.5073425396225,15.1337381226983,7.95674682628607));
#61753=CARTESIAN_POINT('Ctrl Pts',(16.3436274615726,16.1631828364744,7.40728149352596));
#61754=CARTESIAN_POINT('Ctrl Pts',(17.350804549412,16.404051303446,7.9694209838363));
#61755=CARTESIAN_POINT('Ctrl Pts',(16.4552077605916,15.1692434747578,8.03371146916027));
#61756=CARTESIAN_POINT('Ctrl Pts',(16.3029316796438,16.1842453845366,7.47800110793882));
#61757=CARTESIAN_POINT('Ctrl Pts',(17.2966172371086,16.4336390970814,8.0370840771131));
#61758=CARTESIAN_POINT('Ctrl Pts',(16.4289470322599,15.1873823884683,8.07186353228385));
#61759=CARTESIAN_POINT('Ctrl Pts',(16.2823261097163,16.1951736804993,7.51323025737201));
#61760=CARTESIAN_POINT('Ctrl Pts',(17.2693259015807,16.4487548582664,8.07063095624813));
#61761=CARTESIAN_POINT('Ctrl Pts',(16.3495983042681,15.2429346767302,8.18534944533382));
#61762=CARTESIAN_POINT('Ctrl Pts',(16.2199066334893,16.2290620068468,7.61822283696024));
#61763=CARTESIAN_POINT('Ctrl Pts',(17.1868723597951,16.4950484321605,8.17043566131922));
#61764=CARTESIAN_POINT('Ctrl Pts',(16.2959440226898,15.2814828159527,8.25971358276904));
#61765=CARTESIAN_POINT('Ctrl Pts',(16.1771667951557,16.2532836890568,7.68787236799991));
#61766=CARTESIAN_POINT('Ctrl Pts',(17.1311308780761,16.5271718810999,8.23585804734006));
#61767=CARTESIAN_POINT('Ctrl Pts',(16.187190221159,15.3615021794163,8.4059503498022));
#61768=CARTESIAN_POINT('Ctrl Pts',(16.0896613076013,16.3048931839763,7.82601148582257));
#61769=CARTESIAN_POINT('Ctrl Pts',(17.0181681919347,16.5938546843548,8.36455831953807));
#61770=CARTESIAN_POINT('Ctrl Pts',(16.132090655261,15.402973497386,8.47782290206415));
#61771=CARTESIAN_POINT('Ctrl Pts',(16.0449229247606,16.3322434767155,7.89450537829078));
#61772=CARTESIAN_POINT('Ctrl Pts',(16.9609469407587,16.6284141156668,8.42783613794276));
#61773=CARTESIAN_POINT('Ctrl Pts',(16.0623486088442,15.4565900493871,8.56615478270282));
#61774=CARTESIAN_POINT('Ctrl Pts',(15.9875357110085,16.3685339437292,7.97969610658542));
#61775=CARTESIAN_POINT('Ctrl Pts',(16.8885313500831,16.6730945758492,8.5056359305583));
#61776=CARTESIAN_POINT('Ctrl Pts',(16.0483568027876,15.467402285272,8.58374567928398));
#61777=CARTESIAN_POINT('Ctrl Pts',(15.9760448258777,16.3758585928759,7.99662595730545));
#61778=CARTESIAN_POINT('Ctrl Pts',(16.8740037632898,16.6821047723497,8.52113098104961));
#61779=CARTESIAN_POINT('Ctrl Pts',(16.0202872238867,15.489203582786,8.61877757332335));
#61780=CARTESIAN_POINT('Ctrl Pts',(15.9529421275418,16.3907011442425,8.0304074025005));
#61781=CARTESIAN_POINT('Ctrl Pts',(16.8448604825399,16.700272520346,8.55199220635214));
#61782=CARTESIAN_POINT('Ctrl Pts',(16.0062070274775,15.5001945865296,8.63622145671916));
#61783=CARTESIAN_POINT('Ctrl Pts',(15.9413286401597,16.3982198710585,8.04726199906429));
#61784=CARTESIAN_POINT('Ctrl Pts',(16.8302422728064,16.7094316900326,8.56736092530544));
#61785=CARTESIAN_POINT('Ctrl Pts',(15.9639006261601,15.5333825933383,8.68825415449347));
#61786=CARTESIAN_POINT('Ctrl Pts',(15.9064068601577,16.4210005179534,8.09756496571628));
#61787=CARTESIAN_POINT('Ctrl Pts',(16.7863209876344,16.7370883625705,8.61320847706342));
#61788=CARTESIAN_POINT('Ctrl Pts',(15.9355891535234,15.5558095777463,8.72256856997844));
#61789=CARTESIAN_POINT('Ctrl Pts',(15.8829080015083,16.4365560576359,8.13091450103497));
#61790=CARTESIAN_POINT('Ctrl Pts',(16.7569310542553,16.7557775159922,8.64345033245158));
#61791=CARTESIAN_POINT('Ctrl Pts',(15.7935142727831,15.6694196676398,8.89231733959516));
#61792=CARTESIAN_POINT('Ctrl Pts',(15.7654460880884,16.5154266792196,8.29516673757843));
#61793=CARTESIAN_POINT('Ctrl Pts',(16.6094545692347,16.8504525915035,8.79308481198999));
#61794=CARTESIAN_POINT('Ctrl Pts',(15.6782012682718,15.7650152188631,9.02229598142049));
#61795=CARTESIAN_POINT('Ctrl Pts',(15.6678545169391,16.584423347777,8.42399806744112));
#61796=CARTESIAN_POINT('Ctrl Pts',(16.4897904267136,16.9301155500535,8.90776544283607));
#61797=CARTESIAN_POINT('Ctrl Pts',(15.4446903454091,15.9649971701379,9.27157003213102));
#61798=CARTESIAN_POINT('Ctrl Pts',(15.4674094595755,16.7329835035073,8.67390873536768));
#61799=CARTESIAN_POINT('Ctrl Pts',(16.2475203695942,17.0967671767613,9.12791189678674));
#61800=CARTESIAN_POINT('Ctrl Pts',(15.3264914165494,16.0693856149141,9.39086266707201));
#61801=CARTESIAN_POINT('Ctrl Pts',(15.3646387505612,16.8123502221316,8.79517433817847));
#61802=CARTESIAN_POINT('Ctrl Pts',(16.1249134348094,17.1837575468854,9.23337528956514));
#61803=CARTESIAN_POINT('Ctrl Pts',(15.0875705659347,16.2866280399274,9.6194053126835));
#61804=CARTESIAN_POINT('Ctrl Pts',(15.1544604762242,16.9811904583532,9.02980769972348));
#61805=CARTESIAN_POINT('Ctrl Pts',(15.8771249439364,17.3647929014631,9.43565009494142));
#61806=CARTESIAN_POINT('Ctrl Pts',(14.9668478732092,16.3994827876149,9.72865388709201));
#61807=CARTESIAN_POINT('Ctrl Pts',(15.0471084939148,17.0704945862062,9.14336691901707));
#61808=CARTESIAN_POINT('Ctrl Pts',(15.7519425954886,17.4588385242348,9.53246024421486));
#61809=CARTESIAN_POINT('Ctrl Pts',(14.7232109117986,16.6335833330052,9.93750238929769));
#61810=CARTESIAN_POINT('Ctrl Pts',(14.8283473457646,17.258954975949,9.36240017693102));
#61811=CARTESIAN_POINT('Ctrl Pts',(15.4993427309287,17.6539223122627,9.71777676602946));
#61812=CARTESIAN_POINT('Ctrl Pts',(14.6002959559604,16.7548288643997,10.0371018524143));
#61813=CARTESIAN_POINT('Ctrl Pts',(14.7169704858705,17.357964069225,9.46806699747123));
#61814=CARTESIAN_POINT('Ctrl Pts',(15.3719244916505,17.7549602549693,9.80628272069675));
#61815=CARTESIAN_POINT('Ctrl Pts',(14.4145215062612,16.9431175621098,10.1793956077188));
#61816=CARTESIAN_POINT('Ctrl Pts',(14.5465177883743,17.5145354439133,9.62099020379824));
#61817=CARTESIAN_POINT('Ctrl Pts',(15.1793711691479,17.9118675030923,9.93293217024121));
#61818=CARTESIAN_POINT('Ctrl Pts',(14.3523630102681,17.006952463114,10.2256409441351));
#61819=CARTESIAN_POINT('Ctrl Pts',(14.4895201839198,17.5676954028143,9.6707281909746));
#61820=CARTESIAN_POINT('Ctrl Pts',(15.114949088864,17.9650632539259,9.97412895232606));
#61821=CARTESIAN_POINT('Ctrl Pts',(14.2588056678938,17.1043472732383,10.2932311994171));
#61822=CARTESIAN_POINT('Ctrl Pts',(14.4032304693875,17.6494581641149,9.74391620886052));
#61823=CARTESIAN_POINT('Ctrl Pts',(15.0179918642274,18.0462255956853,10.0343961461429));
#61824=CARTESIAN_POINT('Ctrl Pts',(14.2275428962468,17.1371113569171,10.3154811859238));
#61825=CARTESIAN_POINT('Ctrl Pts',(14.3744069573424,17.6769793096807,9.76801833846068));
#61826=CARTESIAN_POINT('Ctrl Pts',(14.9855941905893,18.0735289987137,10.0542450128963));
#61827=CARTESIAN_POINT('Ctrl Pts',(14.1651063844055,17.2029930321826,10.3592551672391));
#61828=CARTESIAN_POINT('Ctrl Pts',(14.3167427850065,17.7324684434336,9.81554948650699));
#61829=CARTESIAN_POINT('Ctrl Pts',(14.9208935457682,18.12843039485,10.0933144453783));
#61830=CARTESIAN_POINT('Ctrl Pts',(14.1339177282514,17.2361258045806,10.380790467117));
#61831=CARTESIAN_POINT('Ctrl Pts',(14.2878875452418,17.7604480955151,9.8389943174788));
#61832=CARTESIAN_POINT('Ctrl Pts',(14.8885751144014,18.1560410384386,10.1125450762014));
#61833=CARTESIAN_POINT('Ctrl Pts',(13.9781364881385,17.4027525271718,10.4867280999607));
#61834=CARTESIAN_POINT('Ctrl Pts',(14.144431831079,17.9006324325898,9.95387647546919));
#61835=CARTESIAN_POINT('Ctrl Pts',(14.7271571232573,18.2948966407755,10.2071949179051));
#61836=CARTESIAN_POINT('Ctrl Pts',(13.8540272655431,17.5391270979538,10.5659251844625));
#61837=CARTESIAN_POINT('Ctrl Pts',(14.028608363573,18.0172146350274,10.0413506176408));
#61838=CARTESIAN_POINT('Ctrl Pts',(14.5985769926317,18.4085421162159,10.2781140808652));
#61839=CARTESIAN_POINT('Ctrl Pts',(13.6072409325253,17.8182304543897,10.713529670147));
#61840=CARTESIAN_POINT('Ctrl Pts',(13.7971283710368,18.2578118922052,10.2058308444696));
#61841=CARTESIAN_POINT('Ctrl Pts',(14.3429475819855,18.6411282467177,10.4106278582409));
#61842=CARTESIAN_POINT('Ctrl Pts',(13.4845627999781,17.9609582798185,10.781937133576));
#61843=CARTESIAN_POINT('Ctrl Pts',(13.68137490276,18.3818077707664,10.2830660507971));
#61844=CARTESIAN_POINT('Ctrl Pts',(14.2158972008177,18.7600681011593,10.4722225230956));
#61845=CARTESIAN_POINT('Ctrl Pts',(13.2411241058063,18.253191261943,10.9079911532372));
#61846=CARTESIAN_POINT('Ctrl Pts',(13.4507300765943,18.6373898413164,10.4269274198646));
#61847=CARTESIAN_POINT('Ctrl Pts',(13.9638433346872,19.0035955862893,10.5861136733016));
#61848=CARTESIAN_POINT('Ctrl Pts',(13.1203620303411,18.4026943555333,10.9656391301105));
#61849=CARTESIAN_POINT('Ctrl Pts',(13.3357311395337,18.7689688605621,10.4937660511775));
#61850=CARTESIAN_POINT('Ctrl Pts',(13.8388382058427,19.1281814976295,10.6384113937824));
#61851=CARTESIAN_POINT('Ctrl Pts',(12.8813643765524,18.709160598925,11.0698962741953));
#61852=CARTESIAN_POINT('Ctrl Pts',(13.1073841447931,19.0401383352438,10.6164410863953));
#61853=CARTESIAN_POINT('Ctrl Pts',(13.5915263050113,19.3835700337331,10.7334679599571));
#61854=CARTESIAN_POINT('Ctrl Pts',(12.7631264212453,18.8661199837945,11.1165087586551));
#61855=CARTESIAN_POINT('Ctrl Pts',(12.9939167896628,19.1797318608651,10.6724778564328));
#61856=CARTESIAN_POINT('Ctrl Pts',(13.4692169404985,19.514369521206,10.7762296953549));
#61857=CARTESIAN_POINT('Ctrl Pts',(12.588256130994,19.107924240872,11.1776586988793));
#61858=CARTESIAN_POINT('Ctrl Pts',(12.8251498460236,19.396355589634,10.7479663558257));
#61859=CARTESIAN_POINT('Ctrl Pts',(13.288413035126,19.7158730686902,10.8327926739995));
#61860=CARTESIAN_POINT('Ctrl Pts',(12.5303820948896,19.1895895478315,11.1965773236667));
#61861=CARTESIAN_POINT('Ctrl Pts',(12.7693698581218,19.4694425906221,10.7716181429504));
#61862=CARTESIAN_POINT('Ctrl Pts',(13.228590194886,19.7839274912126,10.8503809199751));
#61863=CARTESIAN_POINT('Ctrl Pts',(12.4442875600793,19.3138133318091,11.2226618407279));
#61864=CARTESIAN_POINT('Ctrl Pts',(12.6861620401978,19.5809868737173,10.8048576816646));
#61865=CARTESIAN_POINT('Ctrl Pts',(13.1396233538652,19.8874473111499,10.8747803405286));
#61866=CARTESIAN_POINT('Ctrl Pts',(12.4156897929966,19.3555382597294,11.2309788997662));
#61867=CARTESIAN_POINT('Ctrl Pts',(12.6585422539374,19.6184329070213,10.8155506477599));
#61868=CARTESIAN_POINT('Ctrl Pts',(13.110076023704,19.9222180844219,10.8825872590395));
#61869=CARTESIAN_POINT('Ctrl Pts',(12.3589724361245,19.4392584338625,11.2467690565977));
#61870=CARTESIAN_POINT('Ctrl Pts',(12.6037297739884,19.6936318051644,10.8360783405224));
#61871=CARTESIAN_POINT('Ctrl Pts',(13.0514852202568,19.9919848962186,10.8974664623896));
#61872=CARTESIAN_POINT('Ctrl Pts',(12.3308287601266,19.4812877976075,11.254249927555));
#61873=CARTESIAN_POINT('Ctrl Pts',(12.5765109676552,19.7314166631751,10.8459258664003));
#61874=CARTESIAN_POINT('Ctrl Pts',(13.022416850563,20.0270093659881,10.9045459804305));
#61875=CARTESIAN_POINT('Ctrl Pts',(12.1912269576885,19.6923091894597,11.289563129842));
#61876=CARTESIAN_POINT('Ctrl Pts',(12.4419749171144,19.9204932765277,10.892849759858));
#61877=CARTESIAN_POINT('Ctrl Pts',(12.8782548607845,20.2028605259071,10.9381252948214));
#61878=CARTESIAN_POINT('Ctrl Pts',(12.0831043807717,19.8639143262306,11.3111434004142));
#61879=CARTESIAN_POINT('Ctrl Pts',(12.3369629663802,20.0754427469213,10.9238985178924));
#61880=CARTESIAN_POINT('Ctrl Pts',(12.7666864057961,20.3458635515731,10.9591889337323));
#61881=CARTESIAN_POINT('Ctrl Pts',(11.9791786279775,20.0387490638529,11.3256333545128));
#61882=CARTESIAN_POINT('Ctrl Pts',(12.235442756324,20.2343859095505,10.9477939369723));
#61883=CARTESIAN_POINT('Ctrl Pts',(12.659562935147,20.491560421201,10.974081743871));
#61884=CARTESIAN_POINT('Ctrl Pts',(16.5375680855082,20.0478523191736,0.351922770622401));
#61885=CARTESIAN_POINT('Ctrl Pts',(16.5498686081438,19.9784919885108,0.320595854365059));
#61886=CARTESIAN_POINT('Ctrl Pts',(16.5645008101836,19.909569989448,0.289650387375635));
#61887=CARTESIAN_POINT('Ctrl Pts',(16.5814951892386,19.8410460986085,0.259194053810624));
#61888=CARTESIAN_POINT('Ctrl Pts',(16.5876276939095,19.8163189179756,0.248203737115972));
#61889=CARTESIAN_POINT('Ctrl Pts',(16.5940682683641,19.7916436939745,0.237277153603447));
#61890=CARTESIAN_POINT('Ctrl Pts',(16.6008199371749,19.7670190220225,0.226419498601689));
#61891=CARTESIAN_POINT('Ctrl Pts',(16.6135508792567,19.7205867574685,0.205946311772581));
#61892=CARTESIAN_POINT('Ctrl Pts',(16.6273872562386,19.6743339367231,0.185717894040129));
#61893=CARTESIAN_POINT('Ctrl Pts',(16.6423581815811,19.6282521577127,0.165770386909323));
#61894=CARTESIAN_POINT('Ctrl Pts',(16.6498436442524,19.6052112682075,0.15579663334392));
#61895=CARTESIAN_POINT('Ctrl Pts',(16.6576148736858,19.5822076576934,0.145890788161576));
#61896=CARTESIAN_POINT('Ctrl Pts',(16.6656701975499,19.5592586752321,0.136065467307112));
#61897=CARTESIAN_POINT('Ctrl Pts',(16.6696978594819,19.5477841840015,0.131152806879879));
#61898=CARTESIAN_POINT('Ctrl Pts',(16.6737956214272,19.5363259044026,0.126261367078692));
#61899=CARTESIAN_POINT('Ctrl Pts',(16.6779639213557,19.5248837445505,0.121391733564308));
#61900=CARTESIAN_POINT('Ctrl Pts',(16.68004807132,19.5191626646244,0.118956916807116));
#61901=CARTESIAN_POINT('Ctrl Pts',(16.6821498564429,19.5134456148765,0.116527551626322));
#61902=CARTESIAN_POINT('Ctrl Pts',(16.6842693357308,19.5077325845678,0.114103713065847));
#61903=CARTESIAN_POINT('Ctrl Pts',(16.6853290753747,19.5048760694135,0.112891793785614));
#61904=CARTESIAN_POINT('Ctrl Pts',(16.6863950302563,19.5020157956128,0.111678464240845));
#61905=CARTESIAN_POINT('Ctrl Pts',(16.6874607163255,19.4991690245389,0.110473990584703));
#61906=CARTESIAN_POINT('Ctrl Pts',(16.6885264023947,19.496322253465,0.109269516928562));
#61907=CARTESIAN_POINT('Ctrl Pts',(16.68959629266,19.4934770520699,0.108065067624267));
#61908=CARTESIAN_POINT('Ctrl Pts',(16.6906703875662,19.4906334205523,0.106860642655115));
#61909=CARTESIAN_POINT('Origin',(0.,0.,0.));
#61910=CARTESIAN_POINT('Origin',(6.61325378140121E-15,20.5440037453176,
8.67361737988404E-16));
#61911=CARTESIAN_POINT('Ctrl Pts',(-13.7129564349448,20.6615335048059,9.85952349485951));
#61912=CARTESIAN_POINT('Ctrl Pts',(-13.2371163881454,20.6161954472713,9.8616439740488));
#61913=CARTESIAN_POINT('Ctrl Pts',(-12.9440892692056,20.5440037453176,10.2323288156136));
#61914=CARTESIAN_POINT('Ctrl Pts',(-13.7008624134648,20.7562745931684,9.87092777877101));
#61915=CARTESIAN_POINT('Ctrl Pts',(-13.2264454758027,20.7233778620598,9.87599115017895));
#61916=CARTESIAN_POINT('Ctrl Pts',(-12.9326863129145,20.6716508716995,10.2467537707557));
#61917=CARTESIAN_POINT('Ctrl Pts',(-13.6938907193449,20.8508740411617,9.87747041407926));
#61918=CARTESIAN_POINT('Ctrl Pts',(-13.2202702521004,20.8307764858601,9.88425338309928));
#61919=CARTESIAN_POINT('Ctrl Pts',(-12.9261130230882,20.7990969574018,10.2550285610119));
#61920=CARTESIAN_POINT('Ctrl Pts',(-13.6900072944242,21.0397796008549,9.88111811705835));
#61921=CARTESIAN_POINT('Ctrl Pts',(-13.2168370418637,21.0451161585058,9.88885105592462));
#61922=CARTESIAN_POINT('Ctrl Pts',(-12.9224515081237,21.0535913718615,10.2596420840599));
#61923=CARTESIAN_POINT('Ctrl Pts',(-13.6930958642434,21.1340866197803,9.87822261515375));
#61924=CARTESIAN_POINT('Ctrl Pts',(-13.2195733682617,21.1522378018448,9.88519381277553));
#61925=CARTESIAN_POINT('Ctrl Pts',(-12.9253635881698,21.1806406639321,10.2559800621746));
#61926=CARTESIAN_POINT('Ctrl Pts',(-13.7052327444816,21.2753200907549,9.86680289931835));
#61927=CARTESIAN_POINT('Ctrl Pts',(-13.2302950439844,21.3122978585196,9.87081048784163));
#61928=CARTESIAN_POINT('Ctrl Pts',(-12.9368069325275,21.3709184052818,10.2415362188021));
#61929=CARTESIAN_POINT('Ctrl Pts',(-13.7105300124574,21.3223600206349,9.86181478306048));
#61930=CARTESIAN_POINT('Ctrl Pts',(-13.2349772513254,21.3656075188109,9.86452423850202));
#61931=CARTESIAN_POINT('Ctrl Pts',(-12.9418014993605,21.4342948826322,10.2352270743557));
#61932=CARTESIAN_POINT('Ctrl Pts',(-13.720357190954,21.3928615448091,9.85254095225805));
#61933=CARTESIAN_POINT('Ctrl Pts',(-13.2436527129957,21.4453947467137,9.85285084207422));
#61934=CARTESIAN_POINT('Ctrl Pts',(-12.9510671249071,21.5292848798817,10.2234967185532));
#61935=CARTESIAN_POINT('Ctrl Pts',(-13.7239465270711,21.4163523209677,9.8491509266678));
#61936=CARTESIAN_POINT('Ctrl Pts',(-13.2468219311174,21.4719759498813,9.84858285770261));
#61937=CARTESIAN_POINT('Ctrl Pts',(-12.9544513560252,21.5609357545812,10.2192086490361));
#61938=CARTESIAN_POINT('Ctrl Pts',(-13.7298020217399,21.4515736639483,9.84361405487951));
#61939=CARTESIAN_POINT('Ctrl Pts',(-13.25198915428,21.511800561518,9.84161579593135));
#61940=CARTESIAN_POINT('Ctrl Pts',(-12.9599722510621,21.6083932667593,10.212204859321));
#61941=CARTESIAN_POINT('Ctrl Pts',(-13.7318308096277,21.4633010512971,9.84169465498939));
#61942=CARTESIAN_POINT('Ctrl Pts',(-13.2537795725195,21.5250593212155,9.83920044919479));
#61943=CARTESIAN_POINT('Ctrl Pts',(-12.9618851081689,21.6241950353554,10.2097769165122));
#61944=CARTESIAN_POINT('Ctrl Pts',(-13.7360304150215,21.4866713806995,9.83771906460812));
#61945=CARTESIAN_POINT('Ctrl Pts',(-13.2574850933722,21.5514732332995,9.83419845061536));
#61946=CARTESIAN_POINT('Ctrl Pts',(-12.9658447361586,21.6556852063039,10.2047479400592));
#61947=CARTESIAN_POINT('Ctrl Pts',(-13.7382026582792,21.4983229897648,9.83566152684288));
#61948=CARTESIAN_POINT('Ctrl Pts',(-13.2594015448338,21.5646384856195,9.83160997938521));
#61949=CARTESIAN_POINT('Ctrl Pts',(-12.9678928511819,21.6713852864878,10.2021452014677));
#61950=CARTESIAN_POINT('Ctrl Pts',(-13.7583954816181,21.6028889555656,9.81652257225709));
#61951=CARTESIAN_POINT('Ctrl Pts',(-13.2772366388668,21.6829047947831,9.80750493402147));
#61952=CARTESIAN_POINT('Ctrl Pts',(-12.9869317991238,21.8122857656886,10.177934563794));
#61953=CARTESIAN_POINT('Ctrl Pts',(-13.7809040295564,21.693719602389,9.79510721646933));
#61954=CARTESIAN_POINT('Ctrl Pts',(-13.2971007311209,21.7852988934574,9.78055185957662));
#61955=CARTESIAN_POINT('Ctrl Pts',(-13.0081541438556,21.9346925203426,10.1508423296431));
#61956=CARTESIAN_POINT('Ctrl Pts',(-13.8341301723179,21.8714587721286,9.7440196442469));
#61957=CARTESIAN_POINT('Ctrl Pts',(-13.3439003310147,21.9847542762144,9.71648353832225));
#61958=CARTESIAN_POINT('Ctrl Pts',(-13.0583387932841,22.1742604353913,10.0862015740016));
#61959=CARTESIAN_POINT('Ctrl Pts',(-13.8648496341611,21.9583663972777,9.7143454568808));
#61960=CARTESIAN_POINT('Ctrl Pts',(-13.3709025718912,22.0819353397743,9.67927384763397));
#61961=CARTESIAN_POINT('Ctrl Pts',(-13.0873028567095,22.2914203627217,10.0486505478074));
#61962=CARTESIAN_POINT('Ctrl Pts',(-13.9165696229565,22.0859247227897,9.66382831234646));
#61963=CARTESIAN_POINT('Ctrl Pts',(-13.4161030564968,22.2235043007119,9.6162866335379));
#61964=CARTESIAN_POINT('Ctrl Pts',(-13.1360674180666,22.4634190171285,9.98471087522344));
#61965=CARTESIAN_POINT('Ctrl Pts',(-13.9347512757793,22.1279760891408,9.64598616900946));
#61966=CARTESIAN_POINT('Ctrl Pts',(-13.4320016960487,22.2701169401881,9.59402578243727));
#61967=CARTESIAN_POINT('Ctrl Pts',(-13.1532101189578,22.520127147885,9.96212609982419));
#61968=CARTESIAN_POINT('Ctrl Pts',(-13.9586119850529,22.1799633981706,9.62243408712692));
#61969=CARTESIAN_POINT('Ctrl Pts',(-13.4528007586469,22.327479415284,9.56473185020972));
#61970=CARTESIAN_POINT('Ctrl Pts',(-13.1757073593519,22.5902429783183,9.93231047564518));
#61971=CARTESIAN_POINT('Ctrl Pts',(-13.9634401862198,22.1903303348201,9.61766179084814));
#61972=CARTESIAN_POINT('Ctrl Pts',(-13.4570131842341,22.3389231592103,9.5587907059358));
#61973=CARTESIAN_POINT('Ctrl Pts',(-13.1802596632253,22.6042254120874,9.92626886445875));
#61974=CARTESIAN_POINT('Ctrl Pts',(-13.9731827903011,22.2109522681602,9.60801815535573));
#61975=CARTESIAN_POINT('Ctrl Pts',(-13.4655097721022,22.361667873411,9.5467898447481));
#61976=CARTESIAN_POINT('Ctrl Pts',(-13.1894455471525,22.6320401834821,9.91405994122819));
#61977=CARTESIAN_POINT('Ctrl Pts',(-13.9781003259087,22.2212141419427,9.60314372718884));
#61978=CARTESIAN_POINT('Ctrl Pts',(-13.4697968130973,22.3729765457423,9.5407260615401));
#61979=CARTESIAN_POINT('Ctrl Pts',(-13.194082080646,22.645881795839,9.90788871798151));
#61980=CARTESIAN_POINT('Ctrl Pts',(-13.9929886664845,22.2518545078711,9.58836426018849));
#61981=CARTESIAN_POINT('Ctrl Pts',(-13.4827764946496,22.4067278212097,9.52233984264939));
#61982=CARTESIAN_POINT('Ctrl Pts',(-13.2081196590227,22.6872120460856,9.8891768245822));
#61983=CARTESIAN_POINT('Ctrl Pts',(-14.0030951729371,22.2720877777252,9.57830307479199));
#61984=CARTESIAN_POINT('Ctrl Pts',(-13.4915772298429,22.4289668826426,9.50983726183198));
#61985=CARTESIAN_POINT('Ctrl Pts',(-13.2176486506602,22.7145061408827,9.87643797357817));
#61986=CARTESIAN_POINT('Ctrl Pts',(-14.0544950872555,22.3723107632432,9.52697587647896));
#61987=CARTESIAN_POINT('Ctrl Pts',(-13.5364171985493,22.5392216393244,9.4459384887215));
#61988=CARTESIAN_POINT('Ctrl Pts',(-13.2661114274225,22.8497131272088,9.81144708832414));
#61989=CARTESIAN_POINT('Ctrl Pts',(-14.0983814638585,22.4494795558663,9.48265575102692));
#61990=CARTESIAN_POINT('Ctrl Pts',(-13.5745151620739,22.623246501772,9.39101851350584));
#61991=CARTESIAN_POINT('Ctrl Pts',(-13.307490010411,22.9538479586332,9.7553174356521));
#61992=CARTESIAN_POINT('Ctrl Pts',(-14.1908900778254,22.5982767086274,9.38783947033386));
#61993=CARTESIAN_POINT('Ctrl Pts',(-13.6544084086815,22.7837809574408,9.2741414794923));
#61994=CARTESIAN_POINT('Ctrl Pts',(-13.3947124185492,23.1547019112495,9.63520564761807));
#61995=CARTESIAN_POINT('Ctrl Pts',(-14.2395143208195,22.6699034777907,9.33734184539398));
#61996=CARTESIAN_POINT('Ctrl Pts',(-13.6962759549276,22.8603048839474,9.2120652177674));
#61997=CARTESIAN_POINT('Ctrl Pts',(-13.4405581326707,23.2514188762212,9.57122165649343));
#61998=CARTESIAN_POINT('Ctrl Pts',(-14.3028824235611,22.7561439383135,9.27043394448135));
#61999=CARTESIAN_POINT('Ctrl Pts',(-13.7503320008934,22.9510684986001,9.1305999395379));
#62000=CARTESIAN_POINT('Ctrl Pts',(-13.5003052014195,23.3679086709528,9.48642134320106));
#62001=CARTESIAN_POINT('Ctrl Pts',(-14.3156858423305,22.7732269395806,9.25686258744708));
#62002=CARTESIAN_POINT('Ctrl Pts',(-13.7612800093358,22.9690563554823,9.1140363510689));
#62003=CARTESIAN_POINT('Ctrl Pts',(-13.5123769960781,23.3909857126619,9.46921965085858));
#62004=CARTESIAN_POINT('Ctrl Pts',(-14.3415444610434,22.8070653424621,9.22934032392019));
#62005=CARTESIAN_POINT('Ctrl Pts',(-13.7833625282499,23.0045755462846,9.08049093073045));
#62006=CARTESIAN_POINT('Ctrl Pts',(-13.5367579796183,23.4367014225698,9.434332847721));
#62007=CARTESIAN_POINT('Ctrl Pts',(-14.3546119847482,22.8238361574984,9.21537617557595));
#62008=CARTESIAN_POINT('Ctrl Pts',(-13.7945085636611,23.0221227644561,9.06349111287955));
#62009=CARTESIAN_POINT('Ctrl Pts',(-13.5490787875207,23.4593609186655,9.41663094852836));
#62010=CARTESIAN_POINT('Ctrl Pts',(-14.3940884280465,22.8735437111473,9.17301313642827));
#62011=CARTESIAN_POINT('Ctrl Pts',(-13.8281767258758,23.0740233932832,9.01192667725968));
#62012=CARTESIAN_POINT('Ctrl Pts',(-13.5862994342721,23.5265284425343,9.36292504120361));
#62013=CARTESIAN_POINT('Ctrl Pts',(-14.4207294531298,22.9058268139983,9.14418892615148));
#62014=CARTESIAN_POINT('Ctrl Pts',(-13.8508147344641,23.1074533359785,8.97697022835382));
#62015=CARTESIAN_POINT('Ctrl Pts',(-13.6114181147807,23.5701596174622,9.32637822598396));
#62016=CARTESIAN_POINT('Ctrl Pts',(-14.5015145230641,23.0002161807818,9.0560103250754));
#62017=CARTESIAN_POINT('Ctrl Pts',(-13.9194392503705,23.2047432403349,8.87008512211998));
#62018=CARTESIAN_POINT('Ctrl Pts',(-13.687586895431,23.6977533801126,9.21455916568862));
#62019=CARTESIAN_POINT('Ctrl Pts',(-14.5565167428664,23.0598693881876,8.9949541376985));
#62020=CARTESIAN_POINT('Ctrl Pts',(-13.9658098008849,23.2650693985997,8.7966275351461));
#62021=CARTESIAN_POINT('Ctrl Pts',(-13.7394461306717,23.7784254927315,9.13711358232858));
#62022=CARTESIAN_POINT('Ctrl Pts',(-14.668344609763,23.1730054700806,8.86840507942585));
#62023=CARTESIAN_POINT('Ctrl Pts',(-14.0594549219421,23.3775022338952,8.6455112590186));
#62024=CARTESIAN_POINT('Ctrl Pts',(-13.8448838343227,23.9314901957697,8.97654812319932));
#62025=CARTESIAN_POINT('Ctrl Pts',(-14.7251713842222,23.2264870910406,8.80291165328951));
#62026=CARTESIAN_POINT('Ctrl Pts',(-14.1067652302453,23.4295449273,8.56776497327688));
#62027=CARTESIAN_POINT('Ctrl Pts',(-13.8984633639411,24.0038810977667,8.89342755183832));
#62028=CARTESIAN_POINT('Ctrl Pts',(-14.8115128374888,23.3022059813901,8.70132522573414));
#62029=CARTESIAN_POINT('Ctrl Pts',(-14.177907529371,23.501375403437,8.44854965801709));
#62030=CARTESIAN_POINT('Ctrl Pts',(-13.9798710203244,24.106421055664,8.76446179920621));
#62031=CARTESIAN_POINT('Ctrl Pts',(-14.8404776247069,23.3266935233931,8.66690442430847));
#62032=CARTESIAN_POINT('Ctrl Pts',(-14.201761297046,23.5243702015138,8.40818786835522));
#62033=CARTESIAN_POINT('Ctrl Pts',(-14.0071806765434,24.1395912869237,8.72075786856021));
#62034=CARTESIAN_POINT('Ctrl Pts',(-14.8841738662445,23.3622994228145,8.61442455050914));
#62035=CARTESIAN_POINT('Ctrl Pts',(-14.2375569630117,23.5573031545392,8.34701137746259));
#62036=CARTESIAN_POINT('Ctrl Pts',(-14.0483799902215,24.1878351113527,8.65411472810432));
#62037=CARTESIAN_POINT('Ctrl Pts',(-14.898780829388,23.3739803985349,8.59678975566993));
#62038=CARTESIAN_POINT('Ctrl Pts',(-14.2495188731664,23.5680437684686,8.32646567239338));
#62039=CARTESIAN_POINT('Ctrl Pts',(-14.0621522696036,24.2036643463797,8.63171906640857));
#62040=CARTESIAN_POINT('Ctrl Pts',(-14.9280737343777,23.3969664267311,8.56123466719224));
#62041=CARTESIAN_POINT('Ctrl Pts',(-14.2734612706719,23.5890201048075,8.28513372834998));
#62042=CARTESIAN_POINT('Ctrl Pts',(-14.0897712944622,24.2348178206969,8.58656190594739));
#62043=CARTESIAN_POINT('Ctrl Pts',(-14.9427728434619,23.4082813558474,8.54329819094064));
#62044=CARTESIAN_POINT('Ctrl Pts',(-14.2854527847599,23.5992633548238,8.2643275981937));
#62045=CARTESIAN_POINT('Ctrl Pts',(-14.1036304543349,24.2501554507848,8.5637798506607));
#62046=CARTESIAN_POINT('Ctrl Pts',(-15.0162918057908,23.463789382512,8.45309665896628));
#62047=CARTESIAN_POINT('Ctrl Pts',(-14.345589788043,23.6493359864249,8.15945005612194));
#62048=CARTESIAN_POINT('Ctrl Pts',(-14.1729483333222,24.3254089672111,8.4492018977763));
#62049=CARTESIAN_POINT('Ctrl Pts',(-15.0749937583277,23.5046581308708,8.37950805432951));
#62050=CARTESIAN_POINT('Ctrl Pts',(-14.3930063388903,23.6846359402687,8.07502243760036));
#62051=CARTESIAN_POINT('Ctrl Pts',(-14.2282958882168,24.3808520221291,8.35570011884672));
#62052=CARTESIAN_POINT('Ctrl Pts',(-15.1919438181211,23.5795869273186,8.22948916349949));
#62053=CARTESIAN_POINT('Ctrl Pts',(-14.486695680729,23.7467356064268,7.90470339609567));
#62054=CARTESIAN_POINT('Ctrl Pts',(-14.3385630878073,24.482570276287,8.1650313493404));
#62055=CARTESIAN_POINT('Ctrl Pts',(-15.2501924267091,23.613646051469,8.15305871293753));
#62056=CARTESIAN_POINT('Ctrl Pts',(-14.5329550676768,23.7734255231783,7.81879172377405));
#62057=CARTESIAN_POINT('Ctrl Pts',(-14.3934832041134,24.5288442366298,8.06786415465658));
#62058=CARTESIAN_POINT('Ctrl Pts',(-15.3660549813521,23.6750199888892,7.99730768353786));
#62059=CARTESIAN_POINT('Ctrl Pts',(-14.6241723132235,23.8185526248242,7.64575731456955));
#62060=CARTESIAN_POINT('Ctrl Pts',(-14.5027250417167,24.6123032785761,7.86980032335321));
#62061=CARTESIAN_POINT('Ctrl Pts',(-15.4236692333466,23.7023347223222,7.91798719626487));
#62062=CARTESIAN_POINT('Ctrl Pts',(-14.669110374985,23.8368802777693,7.55862491601526));
#62063=CARTESIAN_POINT('Ctrl Pts',(-14.5570470503623,24.6494882615742,7.76890380790145));
#62064=CARTESIAN_POINT('Ctrl Pts',(-15.5381155519261,23.7501002878386,7.7563480148621));
#62065=CARTESIAN_POINT('Ctrl Pts',(-14.7575757640514,23.8653814929517,7.38336094784725));
#62066=CARTESIAN_POINT('Ctrl Pts',(-14.6649535796959,24.7146000317624,7.56324148155097));
#62067=CARTESIAN_POINT('Ctrl Pts',(-15.5949477885535,23.7705518456696,7.67402967710675));
#62068=CARTESIAN_POINT('Ctrl Pts',(-14.8010775596278,23.8754457720047,7.29523076675808));
#62069=CARTESIAN_POINT('Ctrl Pts',(-14.7185382595438,24.7425278102842,7.45847612910266));
#62070=CARTESIAN_POINT('Ctrl Pts',(-15.6583759290202,23.7895227363621,7.57963700695744));
#62071=CARTESIAN_POINT('Ctrl Pts',(-14.848915766986,23.8821191585875,7.19618114873475));
#62072=CARTESIAN_POINT('Ctrl Pts',(-14.778341935074,24.7684964697845,7.33831261712725));
#62073=CARTESIAN_POINT('Ctrl Pts',(-15.6654185515291,23.7915749374926,7.56912092241342));
#62074=CARTESIAN_POINT('Ctrl Pts',(-14.8542511805829,23.8827998732592,7.18510330732812));
#62075=CARTESIAN_POINT('Ctrl Pts',(-14.7849821219855,24.7713067262627,7.32492503082377));
#62076=CARTESIAN_POINT('Ctrl Pts',(-15.6794568481,23.7955570617443,7.54808774958257));
#62077=CARTESIAN_POINT('Ctrl Pts',(-14.8648739978814,23.8840287355543,7.16298628917305));
#62078=CARTESIAN_POINT('Ctrl Pts',(-14.7982182301801,24.7767619627578,7.29814772847103));
#62079=CARTESIAN_POINT('Ctrl Pts',(-15.6864563544083,23.7974881670599,7.53756498179427));
#62080=CARTESIAN_POINT('Ctrl Pts',(-14.8701642040516,23.8845771129149,7.15194123209345));
#62081=CARTESIAN_POINT('Ctrl Pts',(-14.8048177647002,24.7794085602713,7.2847507825764));
#62082=CARTESIAN_POINT('Ctrl Pts',(-15.7073959645382,23.8031021002813,7.50597813481449));
#62083=CARTESIAN_POINT('Ctrl Pts',(-14.885984729689,23.8860275669589,7.11881961059018));
#62084=CARTESIAN_POINT('Ctrl Pts',(-14.8245608256785,24.787105926226,7.24453506904895));
#62085=CARTESIAN_POINT('Ctrl Pts',(-15.7212771599653,23.8066055693578,7.48489551226781));
#62086=CARTESIAN_POINT('Ctrl Pts',(-14.8964386686442,23.8867313559105,7.09681104447996));
#62087=CARTESIAN_POINT('Ctrl Pts',(-14.8376488099401,24.7919142997836,7.2176914258036));
#62088=CARTESIAN_POINT('Ctrl Pts',(-15.7626852346004,23.8164015449187,7.42157346868287));
#62089=CARTESIAN_POINT('Ctrl Pts',(-14.9276026898393,23.8880752497196,7.0308431001553));
#62090=CARTESIAN_POINT('Ctrl Pts',(-14.8766907088792,24.8053737133838,7.13706105153195));
#62091=CARTESIAN_POINT('Ctrl Pts',(-15.7899766087168,23.8219799870563,7.37925987478814));
#62092=CARTESIAN_POINT('Ctrl Pts',(-14.9480092475861,23.8879340460042,6.98716073149568));
#62093=CARTESIAN_POINT('Ctrl Pts',(-14.9024225759064,24.8130595406911,7.08317487963834));
#62094=CARTESIAN_POINT('Ctrl Pts',(-15.8709094466626,23.835869380065,7.2520222729819));
#62095=CARTESIAN_POINT('Ctrl Pts',(-15.0084598442621,23.8845192115295,6.8563707129466));
#62096=CARTESIAN_POINT('Ctrl Pts',(-14.9787306802509,24.8322686771154,6.92111892934993));
#62097=CARTESIAN_POINT('Ctrl Pts',(-15.9236097319743,23.841340127962,7.16680149302588));
#62098=CARTESIAN_POINT('Ctrl Pts',(-15.0473075053422,23.8782090354518,6.77041081593507));
#62099=CARTESIAN_POINT('Ctrl Pts',(-15.0284195206932,24.8399513694313,6.81255177500307));
#62100=CARTESIAN_POINT('Ctrl Pts',(-16.0265018511833,23.8446215600908,6.99556668801121));
#62101=CARTESIAN_POINT('Ctrl Pts',(-15.1226269240625,23.8580414080585,6.6003226406466));
#62102=CARTESIAN_POINT('Ctrl Pts',(-15.1254320902278,24.8449513768056,6.59435812349903));
#62103=CARTESIAN_POINT('Ctrl Pts',(-16.0766936861889,23.8424326922463,6.9095526644017));
#62104=CARTESIAN_POINT('Ctrl Pts',(-15.1590388789855,23.8441003828677,6.51628678808945));
#62105=CARTESIAN_POINT('Ctrl Pts',(-15.1727558203807,24.8422693073838,6.48473162798369));
#62106=CARTESIAN_POINT('Ctrl Pts',(-16.1745669329239,23.8301237547381,6.73672799807676));
#62107=CARTESIAN_POINT('Ctrl Pts',(-15.2296669338826,23.8088460726592,6.35006678355624));
#62108=CARTESIAN_POINT('Ctrl Pts',(-15.2650363101553,24.8261665177154,6.26441776396718));
#62109=CARTESIAN_POINT('Ctrl Pts',(-16.2222483460131,23.8200050092142,6.64991735889322));
#62110=CARTESIAN_POINT('Ctrl Pts',(-15.2638253783645,23.7874652737709,6.26798066443082));
#62111=CARTESIAN_POINT('Ctrl Pts',(-15.3099930710717,24.8127475992357,6.1537303994777));
#62112=CARTESIAN_POINT('Ctrl Pts',(-16.2802777157372,23.802096340301,6.54090305034875));
#62113=CARTESIAN_POINT('Ctrl Pts',(-15.3051135819173,23.7562469286197,6.16689903262489));
#62114=CARTESIAN_POINT('Ctrl Pts',(-15.3647064768095,24.7888483010614,6.01470595587148));
#62115=CARTESIAN_POINT('Ctrl Pts',(-16.29180496139,23.7982510047644,6.51907513414521));
#62116=CARTESIAN_POINT('Ctrl Pts',(-15.3133397276194,23.7497446711847,6.14666201036101));
#62117=CARTESIAN_POINT('Ctrl Pts',(-15.3755750227115,24.7837113625475,5.9868678002244));
#62118=CARTESIAN_POINT('Ctrl Pts',(-16.3089777985448,23.7920800113923,6.48629560658751));
#62119=CARTESIAN_POINT('Ctrl Pts',(-15.3255783192788,23.7396466784538,6.11641210641516));
#62120=CARTESIAN_POINT('Ctrl Pts',(-15.3917665548854,24.7754600011086,5.9450606097844));
#62121=CARTESIAN_POINT('Ctrl Pts',(-16.3146864551117,23.7899542488098,6.47535501215315));
#62122=CARTESIAN_POINT('Ctrl Pts',(-15.3296477791819,23.7362172980268,6.10632970857785));
#62123=CARTESIAN_POINT('Ctrl Pts',(-15.3971490025393,24.772616414018,5.93110659229477));
#62124=CARTESIAN_POINT('Ctrl Pts',(-16.326041455245,23.7855759764293,6.45350549629898));
#62125=CARTESIAN_POINT('Ctrl Pts',(-15.3377398062802,23.7292551260036,6.08623411212909));
#62126=CARTESIAN_POINT('Ctrl Pts',(-15.4078551454552,24.766757373037,5.90323831741779));
#62127=CARTESIAN_POINT('Ctrl Pts',(-16.3316870562881,23.7833238896394,6.44259808404498));
#62128=CARTESIAN_POINT('Ctrl Pts',(-15.3417617125046,23.725722850175,6.07622253802155));
#62129=CARTESIAN_POINT('Ctrl Pts',(-15.4131781407913,24.7637424872307,5.88932598557243));
#62130=CARTESIAN_POINT('Ctrl Pts',(-16.3597569709651,23.7717494556004,6.38814778227077));
#62131=CARTESIAN_POINT('Ctrl Pts',(-15.3617917351086,23.7077741903901,6.02624731012122));
#62132=CARTESIAN_POINT('Ctrl Pts',(-15.4396440601767,24.7482422328457,5.81987342823877));
#62133=CARTESIAN_POINT('Ctrl Pts',(-16.3817071352546,23.7614855762067,6.34486501522732));
#62134=CARTESIAN_POINT('Ctrl Pts',(-15.3774035575898,23.6926313283501,5.98692345337671));
#62135=CARTESIAN_POINT('Ctrl Pts',(-15.4603399296305,24.7344800177032,5.76466031221647));
#62136=CARTESIAN_POINT('Ctrl Pts',(-16.4460911353826,23.7276985047866,6.21585408598055));
#62137=CARTESIAN_POINT('Ctrl Pts',(-15.4233108987322,23.6447437182896,5.87028450901762));
#62138=CARTESIAN_POINT('Ctrl Pts',(-15.5210448436385,24.6891304564638,5.60007535499672));
#62139=CARTESIAN_POINT('Ctrl Pts',(-16.4870597369203,23.7011856762767,6.1309612979369));
#62140=CARTESIAN_POINT('Ctrl Pts',(-15.4524120750771,23.6097680793461,5.79496554732097));
#62141=CARTESIAN_POINT('Ctrl Pts',(-15.5596723827607,24.6534880145847,5.49175537508767));
#62142=CARTESIAN_POINT('Ctrl Pts',(-16.5653255738427,23.6401365395015,5.96347878929924));
#62143=CARTESIAN_POINT('Ctrl Pts',(-15.5082624063114,23.5338042852298,5.64817282485189));
#62144=CARTESIAN_POINT('Ctrl Pts',(-15.6334658856169,24.5713175830139,5.27802294063828));
#62145=CARTESIAN_POINT('Ctrl Pts',(-16.6026225537566,23.6056007131115,5.88088881453209));
#62146=CARTESIAN_POINT('Ctrl Pts',(-15.5349528356564,23.4928190256182,5.57683272933565));
#62147=CARTESIAN_POINT('Ctrl Pts',(-15.6686316100636,24.5247902538067,5.17261015704771));
#62148=CARTESIAN_POINT('Ctrl Pts',(-16.6737438347713,23.528267073217,5.71815276175897));
#62149=CARTESIAN_POINT('Ctrl Pts',(-15.5862895968411,23.404767618473,5.43765450767667));
#62150=CARTESIAN_POINT('Ctrl Pts',(-15.7356888173493,24.42052518513,4.96487762308654));
#62151=CARTESIAN_POINT('Ctrl Pts',(-16.7075680164773,23.4854706778622,5.63800609123987));
#62152=CARTESIAN_POINT('Ctrl Pts',(-15.6108864909551,23.3577197606882,5.36993478547871));
#62153=CARTESIAN_POINT('Ctrl Pts',(-15.7675801892024,24.3627893738512,4.86255711166091));
#62154=CARTESIAN_POINT('Ctrl Pts',(-16.7477821629421,23.4265259278568,5.53948762297091));
#62155=CARTESIAN_POINT('Ctrl Pts',(-15.640442194244,23.2950078236853,5.28746967965312));
#62156=CARTESIAN_POINT('Ctrl Pts',(-15.805496384108,24.2832257277335,4.73676835721291));
#62157=CARTESIAN_POINT('Ctrl Pts',(-16.7557216137502,23.4144639098627,5.51986739539677));
#62158=CARTESIAN_POINT('Ctrl Pts',(-15.6463076234428,23.2822371150873,5.27104653838932));
#62159=CARTESIAN_POINT('Ctrl Pts',(-15.8129821521461,24.2669424871855,4.71171648335875));
#62160=CARTESIAN_POINT('Ctrl Pts',(-16.7674774596505,23.395953969424,5.49056555479367));
#62161=CARTESIAN_POINT('Ctrl Pts',(-15.6550187536544,23.2627774898914,5.24657215146652));
#62162=CARTESIAN_POINT('Ctrl Pts',(-15.8240662353233,24.2419519469095,4.67430176293868));
#62163=CARTESIAN_POINT('Ctrl Pts',(-16.7713692055763,23.3897163634963,5.4808228929721));
#62164=CARTESIAN_POINT('Ctrl Pts',(-15.6579083290139,23.2562391945131,5.238439653045));
#62165=CARTESIAN_POINT('Ctrl Pts',(-15.827735595861,24.2335299973296,4.66186145875231));
#62166=CARTESIAN_POINT('Ctrl Pts',(-16.7790786053942,23.3771398737448,5.46143989175872));
#62167=CARTESIAN_POINT('Ctrl Pts',(-15.6636423926354,23.2430985419099,5.2222741523105));
#62168=CARTESIAN_POINT('Ctrl Pts',(-15.8350044584265,24.2165484323211,4.63711118636381));
#62169=CARTESIAN_POINT('Ctrl Pts',(-16.7828991720825,23.370796439779,5.45179230525798));
#62170=CARTESIAN_POINT('Ctrl Pts',(-15.6664889482879,23.236491490482,5.21423532879162));
#62171=CARTESIAN_POINT('Ctrl Pts',(-15.8386067071377,24.2079826737511,4.62479196472651));
#62172=CARTESIAN_POINT('Ctrl Pts',(-16.8018339398215,23.3388043651893,5.40377346815184));
#62173=CARTESIAN_POINT('Ctrl Pts',(-15.6806350337464,23.2032407115738,5.17421892820013));
#62174=CARTESIAN_POINT('Ctrl Pts',(-15.8564594878516,24.1647804218777,4.5634748554483));
#62175=CARTESIAN_POINT('Ctrl Pts',(-16.8164442132578,23.3123314605357,5.36605914410303));
#62176=CARTESIAN_POINT('Ctrl Pts',(-15.6916183434728,23.176080065211,5.14293310352819));
#62177=CARTESIAN_POINT('Ctrl Pts',(-15.8702348889878,24.1290241585185,4.51531351117569));
#62178=CARTESIAN_POINT('Ctrl Pts',(-16.8587554207317,23.2303040332693,5.25500886580051));
#62179=CARTESIAN_POINT('Ctrl Pts',(-15.7237160931746,23.0927127886327,5.05092031300736));
#62180=CARTESIAN_POINT('Ctrl Pts',(-15.9101283124877,24.0182117167204,4.37349553830628));
#62181=CARTESIAN_POINT('Ctrl Pts',(-16.8849395653287,23.1721462959427,5.18376112194714));
#62182=CARTESIAN_POINT('Ctrl Pts',(-15.7438852600433,23.0348480228381,4.99230333775579));
#62183=CARTESIAN_POINT('Ctrl Pts',(-15.9348162211413,23.9396193270414,4.28249928149494));
#62184=CARTESIAN_POINT('Ctrl Pts',(-16.9336814227243,23.0489054189936,5.04689481422135));
#62185=CARTESIAN_POINT('Ctrl Pts',(-15.7821317178199,22.9140451735304,4.87983224864429));
#62186=CARTESIAN_POINT('Ctrl Pts',(-15.9807728286811,23.7730294410803,4.10768400630364));
#62187=CARTESIAN_POINT('Ctrl Pts',(-16.9562386866201,22.9838226934723,4.98127579196471));
#62188=CARTESIAN_POINT('Ctrl Pts',(-15.8001793820112,22.8511599414675,4.82605841813765));
#62189=CARTESIAN_POINT('Ctrl Pts',(-16.0020411069034,23.6850325081959,4.02386439271881));
#62190=CARTESIAN_POINT('Ctrl Pts',(-16.987604927613,22.8808838764127,4.88722396565768));
#62191=CARTESIAN_POINT('Ctrl Pts',(-15.8257672390934,22.7527257626976,4.74893958754407));
#62192=CARTESIAN_POINT('Ctrl Pts',(-16.0316149906622,23.5458217813753,3.90371897690907));
#62193=CARTESIAN_POINT('Ctrl Pts',(-16.9976481065494,22.8456837005479,4.85660401111989));
#62194=CARTESIAN_POINT('Ctrl Pts',(-15.8340508273298,22.7192129009951,4.72381778995871));
#62195=CARTESIAN_POINT('Ctrl Pts',(-16.0410842740568,23.4982136910247,3.86460270090459));
#62196=CARTESIAN_POINT('Ctrl Pts',(-17.0121203952898,22.7915232573147,4.81180137192049));
#62197=CARTESIAN_POINT('Ctrl Pts',(-15.8461085603811,22.6678599797178,4.68703657852857));
#62198=CARTESIAN_POINT('Ctrl Pts',(-16.0547295745761,23.4249553174748,3.80736693372734));
#62199=CARTESIAN_POINT('Ctrl Pts',(-17.0168457071942,22.7732429751389,4.79705512920603));
#62200=CARTESIAN_POINT('Ctrl Pts',(-15.8500672783871,22.6505576473008,4.6749240778692));
#62201=CARTESIAN_POINT('Ctrl Pts',(-16.0591848688511,23.4002280123538,3.7885282309321));
#62202=CARTESIAN_POINT('Ctrl Pts',(-17.0237883943477,22.7454776880105,4.77522247845058));
#62203=CARTESIAN_POINT('Ctrl Pts',(-15.8559136123358,22.6243253288571,4.65698351812611));
#62204=CARTESIAN_POINT('Ctrl Pts',(-16.0657308308803,23.3626690002606,3.76063612595374));
#62205=CARTESIAN_POINT('Ctrl Pts',(-17.0260800299871,22.7361583484969,4.76798756875114));
#62206=CARTESIAN_POINT('Ctrl Pts',(-15.8578486816174,22.6155273689921,4.65103648873815));
#62207=CARTESIAN_POINT('Ctrl Pts',(-16.0678915160203,23.3500621669768,3.7513931759135));
#62208=CARTESIAN_POINT('Ctrl Pts',(-17.0306066910047,22.7174397302962,4.75364159618235));
#62209=CARTESIAN_POINT('Ctrl Pts',(-15.8616810873489,22.5978702503389,4.63924108014801));
#62210=CARTESIAN_POINT('Ctrl Pts',(-16.0721595105729,23.3247398553012,3.73306538887138));
#62211=CARTESIAN_POINT('Ctrl Pts',(-17.0328409840293,22.7080437567381,4.7465329043636));
#62212=CARTESIAN_POINT('Ctrl Pts',(-15.8635777645221,22.5890142967341,4.63339474291903));
#62213=CARTESIAN_POINT('Ctrl Pts',(-16.0742661298305,23.3120288483462,3.72398358138302));
#62214=CARTESIAN_POINT('Ctrl Pts',(-17.0526933776313,22.6231517872467,4.68313072942519));
#62215=CARTESIAN_POINT('Ctrl Pts',(-15.8804833690792,22.5090194337291,4.58120893371147));
#62216=CARTESIAN_POINT('Ctrl Pts',(-16.0929841004056,23.1971835740226,3.64298279899934));
#62217=CARTESIAN_POINT('Ctrl Pts',(-17.0685242872246,22.5453639920906,4.63085999071918));
#62218=CARTESIAN_POINT('Ctrl Pts',(-15.894267957528,22.4362044579173,4.53811448983722));
#62219=CARTESIAN_POINT('Ctrl Pts',(-16.1079103874777,23.0919335002713,3.57619999707222));
#62220=CARTESIAN_POINT('Ctrl Pts',(-17.0970409468598,22.3852544776922,4.53433068617298));
#62221=CARTESIAN_POINT('Ctrl Pts',(-15.9195637292118,22.2867607205428,4.4582405737583));
#62222=CARTESIAN_POINT('Ctrl Pts',(-16.1347975228886,22.8752733800206,3.45286726728094));
#62223=CARTESIAN_POINT('Ctrl Pts',(-17.1097258727485,22.3029325841582,4.4900723356221));
#62224=CARTESIAN_POINT('Ctrl Pts',(-15.9310656586748,22.2101710019765,4.42148888099321));
#62225=CARTESIAN_POINT('Ctrl Pts',(-16.1467575966226,22.7638630897231,3.39631760321678));
#62226=CARTESIAN_POINT('Ctrl Pts',(-17.1322932109451,22.1337448915264,4.40963331225656));
#62227=CARTESIAN_POINT('Ctrl Pts',(-15.9518657706561,22.0529296192241,4.35443896699023));
#62228=CARTESIAN_POINT('Ctrl Pts',(-16.1680353719467,22.5348731855549,3.29353705876987));
#62229=CARTESIAN_POINT('Ctrl Pts',(-17.1421754383553,22.0468795660126,4.37345174155353));
#62230=CARTESIAN_POINT('Ctrl Pts',(-15.9611598177471,21.9723049166285,4.32415374113437));
#62231=CARTESIAN_POINT('Ctrl Pts',(-16.1773529012751,22.4172942062458,3.2473050216081));
#62232=CARTESIAN_POINT('Ctrl Pts',(-17.1518385746547,21.9465183910894,4.33745974767627));
#62233=CARTESIAN_POINT('Ctrl Pts',(-15.9703702643961,21.8791492254028,4.29392263795542));
#62234=CARTESIAN_POINT('Ctrl Pts',(-16.1864638580397,22.2814390641004,3.20131455964727));
#62235=CARTESIAN_POINT('Ctrl Pts',(-17.1528919760102,21.9353304202433,4.33352625030006));
#62236=CARTESIAN_POINT('Ctrl Pts',(-15.971376200346,21.8687654542568,4.29061743074886));
#62237=CARTESIAN_POINT('Ctrl Pts',(-16.1874570651016,22.266294214612,3.19628833747367));
#62238=CARTESIAN_POINT('Ctrl Pts',(-17.1549585027494,21.9128805671971,4.32579136175763));
#62239=CARTESIAN_POINT('Ctrl Pts',(-15.9733532131519,21.8479295159697,4.28411514135217));
#62240=CARTESIAN_POINT('Ctrl Pts',(-16.1894055045299,22.2359042417173,3.18640467936431));
#62241=CARTESIAN_POINT('Ctrl Pts',(-17.1559725748067,21.9016073705072,4.32198639190832));
#62242=CARTESIAN_POINT('Ctrl Pts',(-15.9743252013516,21.8374668715494,4.28091504945802));
#62243=CARTESIAN_POINT('Ctrl Pts',(-16.1903616296819,22.2206438017773,3.1815426702273));
#62244=CARTESIAN_POINT('Ctrl Pts',(-17.1589399035528,21.8678484081765,4.31082703161848));
#62245=CARTESIAN_POINT('Ctrl Pts',(-15.9771743658607,21.8061355673508,4.27152575218795));
#62246=CARTESIAN_POINT('Ctrl Pts',(-16.1931593966801,22.1749442360078,3.16728315802819));
#62247=CARTESIAN_POINT('Ctrl Pts',(-17.160830065973,21.8452936463181,4.30368403020251));
#62248=CARTESIAN_POINT('Ctrl Pts',(-15.9789960926506,21.7852025809683,4.26551018369033));
#62249=CARTESIAN_POINT('Ctrl Pts',(-16.1949415499539,22.1444113936572,3.15815574296063));
#62250=CARTESIAN_POINT('Ctrl Pts',(-17.1662452354044,21.7774846198971,4.28313524343019));
#62251=CARTESIAN_POINT('Ctrl Pts',(-15.9842317551839,21.7222686670546,4.24819136151219));
#62252=CARTESIAN_POINT('Ctrl Pts',(-16.2000472809384,22.0526157783281,3.13189816377041));
#62253=CARTESIAN_POINT('Ctrl Pts',(-17.1695152559525,21.7320857415583,4.27060912258618));
#62254=CARTESIAN_POINT('Ctrl Pts',(-15.9874166448608,21.6801299212902,4.23761463613163));
#62255=CARTESIAN_POINT('Ctrl Pts',(-16.2031304438779,21.9911560722748,3.11589195795755));
#62256=CARTESIAN_POINT('Ctrl Pts',(-17.1724645676383,21.6864970381169,4.25923772206483));
#62257=CARTESIAN_POINT('Ctrl Pts',(-15.9903039058086,21.6378054978787,4.22799974991249));
#62258=CARTESIAN_POINT('Ctrl Pts',(-16.2059112228881,21.9294381812241,3.10136122305517));
#62259=CARTESIAN_POINT('Origin',(-13.7285795279453,20.5440037453176,10.8524699559538));
#62260=CARTESIAN_POINT('Ctrl Pts',(-12.9440892692056,20.5440037453176,10.2323288156136));
#62261=CARTESIAN_POINT('Ctrl Pts',(-13.2371163881454,20.6161954472713,9.8616439740488));
#62262=CARTESIAN_POINT('Ctrl Pts',(-13.7129564349448,20.6615335048059,9.85952349485951));
#62263=CARTESIAN_POINT('Ctrl Pts',(-12.9499039917696,20.44636701263,10.2249730817137));
#62264=CARTESIAN_POINT('Ctrl Pts',(-13.241415803247,20.541538390444,9.85197635982406));
#62265=CARTESIAN_POINT('Ctrl Pts',(-13.71912369608,20.6132210786213,9.8537079753423));
#62266=CARTESIAN_POINT('Ctrl Pts',(-12.9620352057415,20.3514474462748,10.2172624474079));
#62267=CARTESIAN_POINT('Ctrl Pts',(-13.2507379167627,20.4690074406104,9.83990414196894));
#62268=CARTESIAN_POINT('Ctrl Pts',(-13.73052511494,20.5662589469414,9.84673198254351));
#62269=CARTESIAN_POINT('Ctrl Pts',(-12.9971745343112,20.1663051389932,10.2011795440461));
#62270=CARTESIAN_POINT('Ctrl Pts',(-13.2778281273366,20.3275502669037,9.81157043613493));
#62271=CARTESIAN_POINT('Ctrl Pts',(-13.7623139834302,20.4746690904462,9.83075639181578));
#62272=CARTESIAN_POINT('Ctrl Pts',(-13.0201906855957,20.0760819079927,10.1928069593359));
#62273=CARTESIAN_POINT('Ctrl Pts',(-13.2957015322063,20.2584188213895,9.79523255295137));
#62274=CARTESIAN_POINT('Ctrl Pts',(-13.7827076838172,20.4300420744267,9.82175563922042));
#62275=CARTESIAN_POINT('Ctrl Pts',(-13.0619887611901,19.943864781223,10.1797878662283));
#62276=CARTESIAN_POINT('Ctrl Pts',(-13.3279845155654,20.1571560277764,9.76790383700773));
#62277=CARTESIAN_POINT('Ctrl Pts',(-13.8192667855096,20.3646560151673,9.80690367763832));
#62278=CARTESIAN_POINT('Ctrl Pts',(-13.0771373948911,19.9003134539564,10.1753714795664));
#62279=CARTESIAN_POINT('Ctrl Pts',(-13.3397248017635,20.1236498181765,9.75827221102949));
#62280=CARTESIAN_POINT('Ctrl Pts',(-13.8324507812609,20.3431204394681,9.80172742386782));
#62281=CARTESIAN_POINT('Ctrl Pts',(-13.1097549160981,19.8142002694475,10.1663917888589));
#62282=CARTESIAN_POINT('Ctrl Pts',(-13.3649782408832,20.0572725875454,9.73806010509094));
#62283=CARTESIAN_POINT('Ctrl Pts',(-13.8607136480924,20.3005431616034,9.79094716660411));
#62284=CARTESIAN_POINT('Ctrl Pts',(-13.1271023780073,19.7719591983959,10.1618619296081));
#62285=CARTESIAN_POINT('Ctrl Pts',(-13.378414869638,20.0246324390144,9.72754343587429));
#62286=CARTESIAN_POINT('Ctrl Pts',(-13.8756872686222,20.2796600689745,9.7853833256429));
#62287=CARTESIAN_POINT('Ctrl Pts',(-13.1819446233167,19.6476137998266,10.1481790406719));
#62288=CARTESIAN_POINT('Ctrl Pts',(-13.4209825632648,19.9280025133646,9.69479688704902));
#62289=CARTESIAN_POINT('Ctrl Pts',(-13.9228611331578,20.2181935537061,9.76823863621524));
#62290=CARTESIAN_POINT('Ctrl Pts',(-13.2222530148998,19.5678087202178,10.1389253299632));
#62291=CARTESIAN_POINT('Ctrl Pts',(-13.4522143245307,19.8657922607512,9.67150098704121));
#62292=CARTESIAN_POINT('Ctrl Pts',(-13.9573288153533,20.1787520795032,9.75619699835315));
#62293=CARTESIAN_POINT('Ctrl Pts',(-13.2658111744658,19.4906334205523,10.1295681579593));
#62294=CARTESIAN_POINT('Ctrl Pts',(-13.4855881182943,19.805690718136,9.64706941350936));
#62295=CARTESIAN_POINT('Ctrl Pts',(-13.9943709817605,20.1406244663728,9.74364801533399));
#62296=CARTESIAN_POINT('Origin',(-14.0099940747611,19.8417568621407,10.6978147062773));
#62297=CARTESIAN_POINT('Ctrl Pts',(-13.2658111744658,19.4906334205524,10.1295681579593));
#62298=CARTESIAN_POINT('Ctrl Pts',(-13.4855881182943,19.805690718136,9.64706941350936));
#62299=CARTESIAN_POINT('Ctrl Pts',(-13.9943709817605,20.1406244663728,9.74364801533399));
#62300=CARTESIAN_POINT('Ctrl Pts',(-13.3330814724857,19.3942003585853,10.1010567716054));
#62301=CARTESIAN_POINT('Ctrl Pts',(-13.5481243107023,19.7256553494083,9.61136837775977));
#62302=CARTESIAN_POINT('Ctrl Pts',(-14.0638031593701,20.0691577022518,9.72012608131962));
#62303=CARTESIAN_POINT('Ctrl Pts',(-13.4011178460067,19.3003908944215,10.0693235708264));
#62304=CARTESIAN_POINT('Ctrl Pts',(-13.6107780087442,19.6487795554127,9.57278594043353));
#62305=CARTESIAN_POINT('Ctrl Pts',(-14.134073189902,19.9996605572184,9.69412178028956));
#62306=CARTESIAN_POINT('Ctrl Pts',(-13.5384187734267,19.1175030228593,9.99981903770995));
#62307=CARTESIAN_POINT('Ctrl Pts',(-13.7365209035852,19.5001155576116,9.49010774169617));
#62308=CARTESIAN_POINT('Ctrl Pts',(-14.2759620462211,19.864217269711,9.63746756082801));
#62309=CARTESIAN_POINT('Ctrl Pts',(-13.6076846066159,19.0284254449248,9.96204590686114));
#62310=CARTESIAN_POINT('Ctrl Pts',(-13.7996545986511,19.4283439661347,9.44591917852276));
#62311=CARTESIAN_POINT('Ctrl Pts',(-14.3475817493338,19.7982722534542,9.6068163939335));
#62312=CARTESIAN_POINT('Ctrl Pts',(-13.7472084791682,18.8546463637298,9.88068555234443));
#62313=CARTESIAN_POINT('Ctrl Pts',(-13.9260237622311,19.2896983531623,9.35234401028892));
#62314=CARTESIAN_POINT('Ctrl Pts',(-14.4919140997087,19.6696686338088,9.54104741527293));
#62315=CARTESIAN_POINT('Ctrl Pts',(-13.8174669907381,18.7699457923012,9.83709751132101));
#62316=CARTESIAN_POINT('Ctrl Pts',(-13.989298667415,19.2228465000766,9.3028621243836));
#62317=CARTESIAN_POINT('Ctrl Pts',(-14.5646272658253,19.6070107231862,9.50592896453078));
#62318=CARTESIAN_POINT('Ctrl Pts',(-13.9587830475483,18.6046925960041,9.74419189541089));
#62319=CARTESIAN_POINT('Ctrl Pts',(-14.1156416099841,19.0939700992305,9.19891658502328));
#62320=CARTESIAN_POINT('Ctrl Pts',(-14.7109393570737,19.4848097716012,9.43129554138823));
#62321=CARTESIAN_POINT('Ctrl Pts',(-14.0298409119678,18.5241404513239,9.69487401464713));
#62322=CARTESIAN_POINT('Ctrl Pts',(-14.1787445834152,19.0319737530083,9.14435360774552));
#62323=CARTESIAN_POINT('Ctrl Pts',(-14.7845386303077,19.4252670888976,9.39178032763476));
#62324=CARTESIAN_POINT('Ctrl Pts',(-14.172594896334,18.3670608910262,9.59046937668944));
#62325=CARTESIAN_POINT('Ctrl Pts',(-14.3044456978952,18.9128418187715,9.03038842549872));
#62326=CARTESIAN_POINT('Ctrl Pts',(-14.9324519926951,19.3092027818523,9.30832722037077));
#62327=CARTESIAN_POINT('Ctrl Pts',(-14.2442912388678,18.290533610001,9.53538273635831));
#62328=CARTESIAN_POINT('Ctrl Pts',(-14.3670741811423,18.8557416967525,8.97088159072191));
#62329=CARTESIAN_POINT('Ctrl Pts',(-15.0067663210554,19.2526812602515,9.26438941351549));
#62330=CARTESIAN_POINT('Ctrl Pts',(-14.3342253809499,18.1973729705646,9.4628184729282));
#62331=CARTESIAN_POINT('Ctrl Pts',(-14.4444128857855,18.7878761408221,8.89396908392269));
#62332=CARTESIAN_POINT('Ctrl Pts',(-15.1000164536366,19.183903311546,9.2066277940443));
#62333=CARTESIAN_POINT('Ctrl Pts',(-14.3522279465606,18.1788659986889,9.44812001590431));
#62334=CARTESIAN_POINT('Ctrl Pts',(-14.4599444650823,18.7743836756288,8.87834625763803));
#62335=CARTESIAN_POINT('Ctrl Pts',(-15.1186844003074,19.1702415919389,9.19493326466006));
#62336=CARTESIAN_POINT('Ctrl Pts',(-14.3882626111411,18.1421028768693,9.41834812676606));
#62337=CARTESIAN_POINT('Ctrl Pts',(-14.4909537332673,18.7477161457633,8.84679920366087));
#62338=CARTESIAN_POINT('Ctrl Pts',(-15.1560541122317,19.1431062284371,9.17125694190101));
#62339=CARTESIAN_POINT('Ctrl Pts',(-14.4062921839539,18.1238495975253,9.40327640825083));
#62340=CARTESIAN_POINT('Ctrl Pts',(-14.506429325642,18.734544214775,8.83087535507227));
#62341=CARTESIAN_POINT('Ctrl Pts',(-15.1747532613805,19.1296347066541,9.15927652287954));
#62342=CARTESIAN_POINT('Ctrl Pts',(-14.4602437915794,18.0696447756957,9.35764595009415));
#62343=CARTESIAN_POINT('Ctrl Pts',(-14.552706703401,18.6955593831637,8.78271897853221));
#62344=CARTESIAN_POINT('Ctrl Pts',(-15.2307132513,19.0896341081692,9.1230214409286));
#62345=CARTESIAN_POINT('Ctrl Pts',(-14.4960880148582,18.0341872413021,9.32662342484023));
#62346=CARTESIAN_POINT('Ctrl Pts',(-14.5832283257351,18.6703926017591,8.75023077828758));
#62347=CARTESIAN_POINT('Ctrl Pts',(-15.2678981242241,19.0634739638261,9.09839438287258));
#62348=CARTESIAN_POINT('Ctrl Pts',(-14.6032291315409,17.9298203314146,9.23175293631501));
#62349=CARTESIAN_POINT('Ctrl Pts',(-14.6743100165152,18.5968732851352,8.6511117608008));
#62350=CARTESIAN_POINT('Ctrl Pts',(-15.379065193414,18.9864901941371,9.02314519607624));
#62351=CARTESIAN_POINT('Ctrl Pts',(-14.6741346420556,17.8629129481122,9.16610483335341));
#62352=CARTESIAN_POINT('Ctrl Pts',(-14.7336451616916,18.551149480899,8.58356324766789));
#62353=CARTESIAN_POINT('Ctrl Pts',(-15.4526599555671,18.9371604904354,8.97115719890328));
#62354=CARTESIAN_POINT('Ctrl Pts',(-14.8147873839916,17.7343652083541,9.02995827635105));
#62355=CARTESIAN_POINT('Ctrl Pts',(-14.8498233491032,18.465729859472,8.44542324423527));
#62356=CARTESIAN_POINT('Ctrl Pts',(-15.5986969684513,18.8424271750069,8.8635008260648));
#62357=CARTESIAN_POINT('Ctrl Pts',(-14.8845347880239,17.6727249346549,8.95945991700377));
#62358=CARTESIAN_POINT('Ctrl Pts',(-14.9066386172608,18.4261260159142,8.37476291962935));
#62359=CARTESIAN_POINT('Ctrl Pts',(-15.6711394016455,18.7970236297136,8.80783252485449));
#62360=CARTESIAN_POINT('Ctrl Pts',(-15.0227496766711,17.554755527474,8.81347462073762));
#62361=CARTESIAN_POINT('Ctrl Pts',(-15.017521019286,18.3530371598327,8.23067374372871));
#62362=CARTESIAN_POINT('Ctrl Pts',(-15.8147470349955,18.710170616878,8.69270927527942));
#62363=CARTESIAN_POINT('Ctrl Pts',(-15.0912173674794,17.4984260829599,8.73798808677873));
#62364=CARTESIAN_POINT('Ctrl Pts',(-15.0715513182918,18.3196525669407,8.15718105412623));
#62365=CARTESIAN_POINT('Ctrl Pts',(-15.8859124457149,18.6687209251363,8.6332546393608));
#62366=CARTESIAN_POINT('Ctrl Pts',(-15.2267381193355,17.3912430464634,8.58179117703503));
#62367=CARTESIAN_POINT('Ctrl Pts',(-15.1765900387789,18.2591644871512,8.00772044998079));
#62368=CARTESIAN_POINT('Ctrl Pts',(-16.0268297452482,18.5898927447856,8.51037741448558));
#62369=CARTESIAN_POINT('Ctrl Pts',(-15.293791452939,17.3403886748865,8.501081594441));
#62370=CARTESIAN_POINT('Ctrl Pts',(-15.2275513509012,18.2321712357141,7.93169574084797));
#62371=CARTESIAN_POINT('Ctrl Pts',(-16.096581905656,18.5525136868114,8.44695543962988));
#62372=CARTESIAN_POINT('Ctrl Pts',(-15.3931943675008,17.2684399247589,8.37583698834224));
#62373=CARTESIAN_POINT('Ctrl Pts',(-15.3011653770819,18.1967256137164,7.81658549406654));
#62374=CARTESIAN_POINT('Ctrl Pts',(-16.2000338179115,18.4996619197496,8.34864407946271));
#62375=CARTESIAN_POINT('Ctrl Pts',(-15.4261323093676,17.2451802795294,8.3333911142032));
#62376=CARTESIAN_POINT('Ctrl Pts',(-15.3253918923598,18.1856916248434,7.77776130742633));
#62377=CARTESIAN_POINT('Ctrl Pts',(-16.2343215641098,18.4825816407125,8.3153431447716));
#62378=CARTESIAN_POINT('Ctrl Pts',(-15.4752281274295,17.2114155910319,8.2686329570956));
#62379=CARTESIAN_POINT('Ctrl Pts',(-15.3609931745526,18.1704326848487,7.71929023227925));
#62380=CARTESIAN_POINT('Ctrl Pts',(-16.2854423994633,18.4577956901338,8.26456294500476));
#62381=CARTESIAN_POINT('Ctrl Pts',(-15.4915424610904,17.2003476249094,8.24686402229588));
#62382=CARTESIAN_POINT('Ctrl Pts',(-15.3727782070634,18.1655464655944,7.69968995222783));
#62383=CARTESIAN_POINT('Ctrl Pts',(-16.3024318301415,18.4496723941997,8.24749704105937));
#62384=CARTESIAN_POINT('Ctrl Pts',(-15.5240607039472,17.1785970420959,8.20295981544979));
#62385=CARTESIAN_POINT('Ctrl Pts',(-15.3961216670957,18.1562002365569,7.66037502911479));
#62386=CARTESIAN_POINT('Ctrl Pts',(-16.3363002450403,18.4337115689635,8.21308653597584));
#62387=CARTESIAN_POINT('Ctrl Pts',(-15.540218113459,17.167945517914,8.1808873369451));
#62388=CARTESIAN_POINT('Ctrl Pts',(-15.4076453357983,18.1517557131201,7.64071660882628));
#62389=CARTESIAN_POINT('Ctrl Pts',(-16.3531307989921,18.4258968558046,8.19579114970188));
#62390=CARTESIAN_POINT('Ctrl Pts',(-15.6204924118291,17.1158115451059,8.06991972797963));
#62391=CARTESIAN_POINT('Ctrl Pts',(-15.4649374078242,18.130506147785,7.5417338527351));
#62392=CARTESIAN_POINT('Ctrl Pts',(-16.4367611376568,18.387655095655,8.10886079937315));
#62393=CARTESIAN_POINT('Ctrl Pts',(-15.6830729216002,17.0776936936504,7.97921160142153));
#62394=CARTESIAN_POINT('Ctrl Pts',(-15.5080251086504,18.117315035564,7.46318153823152));
#62395=CARTESIAN_POINT('Ctrl Pts',(-16.5019954870926,18.3597187740705,8.03786762531124));
#62396=CARTESIAN_POINT('Ctrl Pts',(-15.8048218294665,17.0088582451554,7.79379764598993));
#62397=CARTESIAN_POINT('Ctrl Pts',(-15.589527127849,18.0978396117853,7.30672177657495));
#62398=CARTESIAN_POINT('Ctrl Pts',(-16.6289910393939,18.3093178392552,7.89287905000511));
#62399=CARTESIAN_POINT('Ctrl Pts',(-15.8639905947732,16.9781397369617,7.6990922607597));
#62400=CARTESIAN_POINT('Ctrl Pts',(-15.6278243988214,18.0916954466089,7.22887816643367));
#62401=CARTESIAN_POINT('Ctrl Pts',(-16.6907526087972,18.2868525602906,7.81888399718693));
#62402=CARTESIAN_POINT('Ctrl Pts',(-15.9787302986795,16.9244976836848,7.50547883953967));
#62403=CARTESIAN_POINT('Ctrl Pts',(-15.6997459333507,18.0861054933015,7.07442364118823));
#62404=CARTESIAN_POINT('Ctrl Pts',(-16.8106182005044,18.2476791889588,7.66772898825296));
#62405=CARTESIAN_POINT('Ctrl Pts',(-16.0343018499712,16.9015724052595,7.40657160377054));
#62406=CARTESIAN_POINT('Ctrl Pts',(-15.7332497211822,18.0867900683191,6.99790376875797));
#62407=CARTESIAN_POINT('Ctrl Pts',(-16.8687228322341,18.2309698251075,7.59056965666333));
#62408=CARTESIAN_POINT('Ctrl Pts',(-16.1147718948553,16.8734859053583,7.25483467642257));
#62409=CARTESIAN_POINT('Ctrl Pts',(-15.7798484592268,18.092614771922,6.88499408884766));
#62410=CARTESIAN_POINT('Ctrl Pts',(-16.9529490202363,18.2105552719868,7.4722804229554));
#62411=CARTESIAN_POINT('Ctrl Pts',(-16.1411134573278,16.865175788199,7.20369221675809));
#62412=CARTESIAN_POINT('Ctrl Pts',(-15.7948569320189,18.0953910933679,6.84743092050601));
#62413=CARTESIAN_POINT('Ctrl Pts',(-16.9805353881954,18.2045266761679,7.43242501444395));
#62414=CARTESIAN_POINT('Ctrl Pts',(-16.179873357956,16.8543648698465,7.12609670173211));
#62415=CARTESIAN_POINT('Ctrl Pts',(-15.8164668360564,18.1007300607159,6.79160558134888));
#62416=CARTESIAN_POINT('Ctrl Pts',(-17.0211518386022,18.1967038372177,7.37197466884147));
#62417=CARTESIAN_POINT('Ctrl Pts',(-16.1926678712388,16.851037084605,7.1000844945737));
#62418=CARTESIAN_POINT('Ctrl Pts',(-15.8235412294377,18.1027139619363,6.77302390988603));
#62419=CARTESIAN_POINT('Ctrl Pts',(-17.0345634258717,18.1942996744008,7.35171329796697));
#62420=CARTESIAN_POINT('Ctrl Pts',(-16.2180004190603,16.8449478242919,7.04775905974781));
#62421=CARTESIAN_POINT('Ctrl Pts',(-15.8374071874885,18.1070733465416,6.73600069327743));
#62422=CARTESIAN_POINT('Ctrl Pts',(-17.0611266078686,18.1899089301747,7.31096259568511));
#62423=CARTESIAN_POINT('Ctrl Pts',(-16.2305410528683,16.8421866209048,7.021438990984));
#62424=CARTESIAN_POINT('Ctrl Pts',(-15.8441979516698,18.1094515393965,6.71755750861181));
#62425=CARTESIAN_POINT('Ctrl Pts',(-17.0742809443064,18.1879225621902,7.29046794760879));
#62426=CARTESIAN_POINT('Ctrl Pts',(-16.2922822294683,16.8298893484966,6.88973237378449));
#62427=CARTESIAN_POINT('Ctrl Pts',(-15.8775127685803,18.1223215324931,6.6255585108361));
#62428=CARTESIAN_POINT('Ctrl Pts',(-17.1390667357784,18.1791017859522,7.18792777564085));
#62429=CARTESIAN_POINT('Ctrl Pts',(-16.3388527132311,16.82480604532,6.78351336529713));
#62430=CARTESIAN_POINT('Ctrl Pts',(-15.9012994364871,18.1354945701909,6.55484584731165));
#62431=CARTESIAN_POINT('Ctrl Pts',(-17.1880086635335,18.1755473529931,7.105281360654));
#62432=CARTESIAN_POINT('Ctrl Pts',(-16.42625671668,16.8244865951818,6.56935996317588));
#62433=CARTESIAN_POINT('Ctrl Pts',(-15.9444744339779,18.166665793471,6.41786159094849));
#62434=CARTESIAN_POINT('Ctrl Pts',(-17.2800328788574,18.175687345345,6.93874263504849));
#62435=CARTESIAN_POINT('Ctrl Pts',(-16.4670907877957,16.8292488785245,6.46142568826117));
#62436=CARTESIAN_POINT('Ctrl Pts',(-15.9637438210817,18.1847031383132,6.35181980812632));
#62437=CARTESIAN_POINT('Ctrl Pts',(-17.3231157119331,18.1793806176926,6.85485042618645));
#62438=CARTESIAN_POINT('Ctrl Pts',(-16.5428322128861,16.8492020210022,6.24380857126078));
#62439=CARTESIAN_POINT('Ctrl Pts',(-15.998670856686,18.2247711780283,6.2238904177288));
#62440=CARTESIAN_POINT('Ctrl Pts',(-17.4032368975643,18.1944406370503,6.685783601792));
#62441=CARTESIAN_POINT('Ctrl Pts',(-16.5777406346628,16.8643899311763,6.13412597445859));
#62442=CARTESIAN_POINT('Ctrl Pts',(-16.0142343185671,18.2467999928255,6.16223101846773));
#62443=CARTESIAN_POINT('Ctrl Pts',(-17.4402763132042,18.2058052131984,6.60060918559835));
#62444=CARTESIAN_POINT('Ctrl Pts',(-16.6135037166622,16.887843870671,6.00971363205832));
#62445=CARTESIAN_POINT('Ctrl Pts',(-16.0301006340142,18.2733421491226,6.09509973493942));
#62446=CARTESIAN_POINT('Ctrl Pts',(-17.4783728672101,18.2232745427781,6.50403280278535));
#62447=CARTESIAN_POINT('Ctrl Pts',(-16.6174285656065,16.8905385400829,5.99587585692918));
#62448=CARTESIAN_POINT('Ctrl Pts',(-16.0318496897817,18.2763319679881,6.08763237324531));
#62449=CARTESIAN_POINT('Ctrl Pts',(-17.4825561029328,18.225280813882,6.49329158746432));
#62450=CARTESIAN_POINT('Ctrl Pts',(-16.6251798307496,16.8961074160593,5.96817177686506));
#62451=CARTESIAN_POINT('Ctrl Pts',(-16.0353047841429,18.2823634442865,6.07275077263818));
#62452=CARTESIAN_POINT('Ctrl Pts',(-17.4908223733553,18.2294254288441,6.47178799400402));
#62453=CARTESIAN_POINT('Ctrl Pts',(-16.6290088701947,16.8989837089351,5.95429578968276));
#62454=CARTESIAN_POINT('Ctrl Pts',(-16.0370118502271,18.2854071690753,6.06533182326545));
#62455=CARTESIAN_POINT('Ctrl Pts',(-17.4949082093827,18.2315653247675,6.46101810150374));
#62456=CARTESIAN_POINT('Ctrl Pts',(-16.640327690256,16.9078699152518,5.9126963948273));
#62457=CARTESIAN_POINT('Ctrl Pts',(-16.0420655799591,18.2946050780723,6.04317482379761));
#62458=CARTESIAN_POINT('Ctrl Pts',(-17.5069934597519,18.2381741848721,6.42873203287291));
#62459=CARTESIAN_POINT('Ctrl Pts',(-16.6476390588876,16.9141283412814,5.88504004653775));
#62460=CARTESIAN_POINT('Ctrl Pts',(-16.0453328192631,18.3008046027441,6.02858871996637));
#62461=CARTESIAN_POINT('Ctrl Pts',(-17.5148098007386,18.2428257703185,6.40726933694612));
#62462=CARTESIAN_POINT('Ctrl Pts',(-16.668876924417,16.9339042773692,5.8023015083001));
#62463=CARTESIAN_POINT('Ctrl Pts',(-16.0548762168224,18.3196280402113,5.9852540398304));
#62464=CARTESIAN_POINT('Ctrl Pts',(-17.53754506196,18.2575159307706,6.34306548117756));
#62465=CARTESIAN_POINT('Ctrl Pts',(-16.6821074672649,16.9484219473983,5.74744970190452));
#62466=CARTESIAN_POINT('Ctrl Pts',(-16.0608653387976,18.3324239286334,5.95705652973751));
#62467=CARTESIAN_POINT('Ctrl Pts',(-17.5517505124874,18.2682895399416,6.30050845290031));
#62468=CARTESIAN_POINT('Ctrl Pts',(-16.7190627591152,16.9959765026082,5.58382645621117));
#62469=CARTESIAN_POINT('Ctrl Pts',(-16.0779779753248,18.3716198957327,5.87385449259152));
#62470=CARTESIAN_POINT('Ctrl Pts',(-17.5915635598182,18.3035512121968,6.17357906259382));
#62471=CARTESIAN_POINT('Ctrl Pts',(-16.7400555978829,17.0330066603434,5.47598507636511));
#62472=CARTESIAN_POINT('Ctrl Pts',(-16.0881503846021,18.3985925034547,5.82073746488337));
#62473=CARTESIAN_POINT('Ctrl Pts',(-17.614372369325,18.3309739871534,6.08994669325491));
#62474=CARTESIAN_POINT('Ctrl Pts',(-16.7748996695109,17.1179178086824,5.26288874533716));
#62475=CARTESIAN_POINT('Ctrl Pts',(-16.1068711035242,18.4545293431909,5.71670683995154));
#62476=CARTESIAN_POINT('Ctrl Pts',(-17.6526840179692,18.3937954811266,5.92472292226959));
#62477=CARTESIAN_POINT('Ctrl Pts',(-16.7887511957117,17.165797405872,5.15763334311937));
#62478=CARTESIAN_POINT('Ctrl Pts',(-16.1153790545225,18.4834009489052,5.6659869756034));
#62479=CARTESIAN_POINT('Ctrl Pts',(-17.6681871322247,18.4291931720276,5.84313118244005));
#62480=CARTESIAN_POINT('Ctrl Pts',(-16.8041731774862,17.2461122278424,5.00182303805251));
#62481=CARTESIAN_POINT('Ctrl Pts',(-16.1271293851317,18.5287334432286,5.59018616575563));
#62482=CARTESIAN_POINT('Ctrl Pts',(-17.6859716250702,18.488536683831,5.72236773806957));
#62483=CARTESIAN_POINT('Ctrl Pts',(-16.80842012977,17.2743020559593,4.95023234528506));
#62484=CARTESIAN_POINT('Ctrl Pts',(-16.1308693537085,18.5441726270768,5.56499312469953));
#62485=CARTESIAN_POINT('Ctrl Pts',(-17.6909869150959,18.5093607347263,5.68238443728928));
#62486=CARTESIAN_POINT('Ctrl Pts',(-16.8134387928951,17.3187824429628,4.87338836572715));
#62487=CARTESIAN_POINT('Ctrl Pts',(-16.1362139667238,18.5679584891248,5.52711906840436));
#62488=CARTESIAN_POINT('Ctrl Pts',(-17.6971302169662,18.5422117789673,5.62283295445145));
#62489=CARTESIAN_POINT('Ctrl Pts',(-16.8148874382565,17.3339975860732,4.84782944445022));
#62490=CARTESIAN_POINT('Ctrl Pts',(-16.1379523469422,18.5759993141217,5.51446949942686));
#62491=CARTESIAN_POINT('Ctrl Pts',(-17.6989495862611,18.5534478320083,5.60302622434831));
#62492=CARTESIAN_POINT('Ctrl Pts',(-16.8173177844478,17.3649734626395,4.79721739740923));
#62493=CARTESIAN_POINT('Ctrl Pts',(-16.1413150962685,18.5922074383504,5.48928101372498));
#62494=CARTESIAN_POINT('Ctrl Pts',(-17.7021076435685,18.5763207522729,5.56380568192218));
#62495=CARTESIAN_POINT('Ctrl Pts',(-16.81830211771,17.3807509529757,4.77213331007082));
#62496=CARTESIAN_POINT('Ctrl Pts',(-16.1429414050274,18.6003821235283,5.47672970918627));
#62497=CARTESIAN_POINT('Ctrl Pts',(-17.703449425713,18.5879699978769,5.54436787357638));
#62498=CARTESIAN_POINT('Ctrl Pts',(-16.8220954270744,17.4610719963788,4.64781136383888));
#62499=CARTESIAN_POINT('Ctrl Pts',(-16.1507859818905,18.64162416143,5.41417782127868));
#62500=CARTESIAN_POINT('Ctrl Pts',(-17.7089990632976,18.6472699541193,5.44803201127134));
#62501=CARTESIAN_POINT('Ctrl Pts',(-16.8215276491358,17.5299062590181,4.55186134052271));
#62502=CARTESIAN_POINT('Ctrl Pts',(-16.1561810404284,18.6758805436289,5.36460911067975));
#62503=CARTESIAN_POINT('Ctrl Pts',(-17.709737672067,18.6980744122179,5.37368742584704));
#62504=CARTESIAN_POINT('Ctrl Pts',(-16.8137088203987,17.6765330986877,4.36681604087379));
#62505=CARTESIAN_POINT('Ctrl Pts',(-16.1648649353469,18.7484754011972,5.26511564077504));
#62506=CARTESIAN_POINT('Ctrl Pts',(-17.7043582887925,18.8062737645121,5.23031280416359));
#62507=CARTESIAN_POINT('Ctrl Pts',(-16.8064567973355,17.7543260220656,4.27772105086972));
#62508=CARTESIAN_POINT('Ctrl Pts',(-16.1681498046237,18.7866860991184,5.21534216184175));
#62509=CARTESIAN_POINT('Ctrl Pts',(-17.6982392734343,18.863668906634,5.16128300573129));
#62510=CARTESIAN_POINT('Ctrl Pts',(-16.7908108551635,17.8777735500095,4.14924084351727));
#62511=CARTESIAN_POINT('Ctrl Pts',(-16.1710402262194,18.8483363059671,5.13994566835684));
#62512=CARTESIAN_POINT('Ctrl Pts',(-17.6841764321443,18.9547385014575,5.06173621213073));
#62513=CARTESIAN_POINT('Ctrl Pts',(-16.7847994760353,17.9200509798971,4.10727592102829));
#62514=CARTESIAN_POINT('Ctrl Pts',(-16.1716622035887,18.869516190848,5.11480160040562));
#62515=CARTESIAN_POINT('Ctrl Pts',(-17.6786733100718,18.9859259149757,5.02922140144999));
#62516=CARTESIAN_POINT('Ctrl Pts',(-16.7763053981147,17.9743268356373,4.05591029156792));
#62517=CARTESIAN_POINT('Ctrl Pts',(-16.171956931833,18.8970271211957,5.08321199995914));
#62518=CARTESIAN_POINT('Ctrl Pts',(-17.6707913903831,19.0259631606368,4.98942219883545));
#62519=CARTESIAN_POINT('Ctrl Pts',(-16.7745575630922,17.9852534999052,4.04569172176441));
#62520=CARTESIAN_POINT('Ctrl Pts',(-16.1719917095952,18.9025678356017,5.07690116321743));
#62521=CARTESIAN_POINT('Ctrl Pts',(-17.6691648279995,19.0340232881386,4.98150459759356));
#62522=CARTESIAN_POINT('Ctrl Pts',(-16.7709641270619,18.0072504455116,4.02536414779665));
#62523=CARTESIAN_POINT('Ctrl Pts',(-16.1720115721074,18.9137499738595,5.06427051983082));
#62524=CARTESIAN_POINT('Ctrl Pts',(-17.6658116455112,19.050249378955,4.9657542197225));
#62525=CARTESIAN_POINT('Ctrl Pts',(-16.7691176506656,18.0183255954815,4.01525090736688));
#62526=CARTESIAN_POINT('Ctrl Pts',(-16.1719966680687,18.9193935894147,5.05794822246791));
#62527=CARTESIAN_POINT('Ctrl Pts',(-17.6640841987627,19.0584189335486,4.95791816069434));
#62528=CARTESIAN_POINT('Ctrl Pts',(-16.7634483218102,18.0516727098935,3.98516089302837));
#62529=CARTESIAN_POINT('Ctrl Pts',(-16.1718758121784,18.9364205373016,5.03903418912846));
#62530=CARTESIAN_POINT('Ctrl Pts',(-17.6587675705056,19.0830172109,4.93460335385762));
#62531=CARTESIAN_POINT('Ctrl Pts',(-16.7594911869187,18.0740941534329,3.965407621031));
#62532=CARTESIAN_POINT('Ctrl Pts',(-16.171694082726,18.9479341486161,5.02645603071105));
#62533=CARTESIAN_POINT('Ctrl Pts',(-17.6550400294926,19.09955606405,4.91929767070209));
#62534=CARTESIAN_POINT('Ctrl Pts',(-16.7388442855259,18.1871389326756,3.86814986546794));
#62535=CARTESIAN_POINT('Ctrl Pts',(-16.1702666252171,19.0060927232367,4.9640131612077));
#62536=CARTESIAN_POINT('Ctrl Pts',(-17.635514525068,19.182941342502,4.84393739128064));
#62537=CARTESIAN_POINT('Ctrl Pts',(-16.719579385685,18.2805678928541,3.79515926871854));
#62538=CARTESIAN_POINT('Ctrl Pts',(-16.1674668650467,19.0553583202436,4.91452255413311));
#62539=CARTESIAN_POINT('Ctrl Pts',(-17.6170620237919,19.251855614714,4.7873778337322));
#62540=CARTESIAN_POINT('Ctrl Pts',(-16.6760920287696,18.4732081087098,3.65836854066126));
#62541=CARTESIAN_POINT('Ctrl Pts',(-16.1580801288288,19.1600515548782,4.81721936383231));
#62542=CARTESIAN_POINT('Ctrl Pts',(-17.5750533192918,19.3939530516457,4.68137555884256));
#62543=CARTESIAN_POINT('Ctrl Pts',(-16.6518681727065,18.5724200982118,3.59456982019734));
#62544=CARTESIAN_POINT('Ctrl Pts',(-16.1515441951085,19.2153318690365,4.76945799524684));
#62545=CARTESIAN_POINT('Ctrl Pts',(-17.5514956562874,19.4671367442649,4.63193394000491));
#62546=CARTESIAN_POINT('Ctrl Pts',(-16.6120711601853,18.7255472795203,3.50564398372098));
#62547=CARTESIAN_POINT('Ctrl Pts',(-16.1385914317911,19.3035904494646,4.69942714954636));
#62548=CARTESIAN_POINT('Ctrl Pts',(-17.5126004219238,19.5800987486598,4.56301866603759));
#62549=CARTESIAN_POINT('Ctrl Pts',(-16.598227256611,18.7773090937269,3.47713276907664));
#62550=CARTESIAN_POINT('Ctrl Pts',(-16.1337817240602,19.3337268967015,4.6764723023167));
#62551=CARTESIAN_POINT('Ctrl Pts',(-17.4990408092191,19.6182847258373,4.54092302367441));
#62552=CARTESIAN_POINT('Ctrl Pts',(-16.5766147929995,18.8560382528438,3.43606457582562));
#62553=CARTESIAN_POINT('Ctrl Pts',(-16.125752890255,19.3803013963805,4.64253099430504));
#62554=CARTESIAN_POINT('Ctrl Pts',(-17.4778314381254,19.6763676751938,4.50909627003073));
#62555=CARTESIAN_POINT('Ctrl Pts',(-16.5692661085865,18.882474353998,3.42265254898412));
#62556=CARTESIAN_POINT('Ctrl Pts',(-16.1229478535309,19.3960191571751,4.63132270544163));
#62557=CARTESIAN_POINT('Ctrl Pts',(-17.4706132806969,19.6958714905778,4.49870236157246));
#62558=CARTESIAN_POINT('Ctrl Pts',(-16.5543030537792,18.9356607661424,3.39642157189387));
#62559=CARTESIAN_POINT('Ctrl Pts',(-16.1170726225119,19.4278597569896,4.60912436043551));
#62560=CARTESIAN_POINT('Ctrl Pts',(-17.455903407128,19.7351118543264,4.47837438560283));
#62561=CARTESIAN_POINT('Ctrl Pts',(-16.5467098413558,18.9623361970568,3.38363919167274));
#62562=CARTESIAN_POINT('Ctrl Pts',(-16.1140117884356,19.4439357929648,4.59816504831983));
#62563=CARTESIAN_POINT('Ctrl Pts',(-17.4484324969103,19.7547931562087,4.46846865770835));
#62564=CARTESIAN_POINT('Ctrl Pts',(-16.508202977113,19.0961201099036,3.3213639916356));
#62565=CARTESIAN_POINT('Ctrl Pts',(-16.098169889326,19.524689281414,4.54436605394745));
#62566=CARTESIAN_POINT('Ctrl Pts',(-17.4105164892993,19.8535022542627,4.42020926695778));
#62567=CARTESIAN_POINT('Ctrl Pts',(-16.4756732929089,19.2044463729661,3.27676843062349));
#62568=CARTESIAN_POINT('Ctrl Pts',(-16.0834884075578,19.5920801013394,4.50338912963289));
#62569=CARTESIAN_POINT('Ctrl Pts',(-17.3783936837892,19.9334359956607,4.38565331806935));
#62570=CARTESIAN_POINT('Ctrl Pts',(-16.4075080632038,19.4236276169736,3.19750638204053));
#62571=CARTESIAN_POINT('Ctrl Pts',(-16.0501955905981,19.7318341839477,4.42667684719545));
#62572=CARTESIAN_POINT('Ctrl Pts',(-17.3109257615026,20.0951899517967,4.32425010281472));
#62573=CARTESIAN_POINT('Ctrl Pts',(-16.3718715237024,19.5344829234921,3.16284173499306));
#62574=CARTESIAN_POINT('Ctrl Pts',(-16.0316406956358,19.8041162452577,4.39087890945558));
#62575=CARTESIAN_POINT('Ctrl Pts',(-17.2755796078532,20.1770103953973,4.29740425493055));
#62576=CARTESIAN_POINT('Ctrl Pts',(-16.297689249875,19.7587108437685,3.10321810060762));
#62577=CARTESIAN_POINT('Ctrl Pts',(-15.9906690323896,19.9534816196041,4.32512422071333));
#62578=CARTESIAN_POINT('Ctrl Pts',(-17.2018700972943,20.3425337283146,4.25125855596935));
#62579=CARTESIAN_POINT('Ctrl Pts',(-16.2591431712307,19.8720835434029,3.07825968438735));
#62580=CARTESIAN_POINT('Ctrl Pts',(-15.9683052469682,20.0304964466515,4.29509127689048));
#62581=CARTESIAN_POINT('Ctrl Pts',(-17.163506384661,20.4262366718118,4.23195913303276));
#62582=CARTESIAN_POINT('Ctrl Pts',(-16.2091884282023,20.0153974657703,3.05314750912563));
#62583=CARTESIAN_POINT('Ctrl Pts',(-15.9378084682126,20.13015180225,4.26142632520722));
#62584=CARTESIAN_POINT('Ctrl Pts',(-17.1137137415339,20.5320627708622,4.21257430606212));
#62585=CARTESIAN_POINT('Ctrl Pts',(-16.1991200546222,20.0441069891588,3.0484364867405));
#62586=CARTESIAN_POINT('Ctrl Pts',(-15.9316281716696,20.1501045344835,4.2549337075549));
#62587=CARTESIAN_POINT('Ctrl Pts',(-17.1036744360849,20.5532633748179,4.20893982211271));
#62588=CARTESIAN_POINT('Ctrl Pts',(-16.1788950376696,20.101436421715,3.03965994049603));
#62589=CARTESIAN_POINT('Ctrl Pts',(-15.9190872506462,20.1901176618968,4.24241030450447));
#62590=CARTESIAN_POINT('Ctrl Pts',(-17.0835007615317,20.5956001829815,4.20217346458416));
#62591=CARTESIAN_POINT('Ctrl Pts',(-16.1687290012613,20.1300833200632,3.03558960937044));
#62592=CARTESIAN_POINT('Ctrl Pts',(-15.9127214251302,20.2101966625484,4.23637156842712));
#62593=CARTESIAN_POINT('Ctrl Pts',(-17.0733570306589,20.6167563162349,4.19903787894888));
#62594=CARTESIAN_POINT('Ctrl Pts',(-16.1380734967344,20.2159716731412,3.02431921476223));
#62595=CARTESIAN_POINT('Ctrl Pts',(-15.8933731832392,20.270545713034,4.21895892653054));
#62596=CARTESIAN_POINT('Ctrl Pts',(-17.0427584915315,20.680188767493,4.1903639156326));
#62597=CARTESIAN_POINT('Ctrl Pts',(-16.1174268255799,20.27316083266,3.01805921896905));
#62598=CARTESIAN_POINT('Ctrl Pts',(-15.8800805679254,20.3111220050017,4.20822312872908));
#62599=CARTESIAN_POINT('Ctrl Pts',(-17.0221365311604,20.7224291906978,4.18555791480855));
#62600=CARTESIAN_POINT('Ctrl Pts',(-16.0965766384649,20.3302824207005,3.01302436959042));
#62601=CARTESIAN_POINT('Ctrl Pts',(-15.8663823430535,20.3520823377266,4.19836680673276));
#62602=CARTESIAN_POINT('Ctrl Pts',(-17.0012980588419,20.7646233900099,4.18170722839425));
#62603=CARTESIAN_POINT('Origin',(-31.4,21.,7.));
#62604=CARTESIAN_POINT('',(-31.7,19.3924770032404,8.64926829419482));
#62605=CARTESIAN_POINT('Ctrl Pts',(-31.4046869279001,19.0836514699531,8.7616715958928));
#62606=CARTESIAN_POINT('Ctrl Pts',(-31.4396270223971,19.0842071229975,8.76146935472406));
#62607=CARTESIAN_POINT('Ctrl Pts',(-31.4796949749373,19.0925507901701,8.75843250822859));
#62608=CARTESIAN_POINT('Ctrl Pts',(-31.5457246229044,19.1194392293618,8.74864591671695));
#62609=CARTESIAN_POINT('Ctrl Pts',(-31.5824397836614,19.143919114572,8.73973596716218));
#62610=CARTESIAN_POINT('Ctrl Pts',(-31.6356608467856,19.1964897272736,8.72060182894167));
#62611=CARTESIAN_POINT('Ctrl Pts',(-31.6609177668595,19.2344479852018,8.70678615291121));
#62612=CARTESIAN_POINT('Ctrl Pts',(-31.6908725620847,19.3060567911241,8.68072267904415));
#62613=CARTESIAN_POINT('Ctrl Pts',(-31.7,19.3528406701053,8.66369473965147));
#62614=CARTESIAN_POINT('Ctrl Pts',(-31.7,19.3924770032404,8.64926829419483));
#62615=CARTESIAN_POINT('',(-31.7,23.291563283411,7.23011694737699));
#62616=CARTESIAN_POINT('Ctrl Pts',(-31.7,23.291563283411,7.23011694737701));
#62617=CARTESIAN_POINT('Ctrl Pts',(-31.7,23.3311996165461,7.21569050192038));
#62618=CARTESIAN_POINT('Ctrl Pts',(-31.6908725620847,23.3779834955273,7.1986625625277));
#62619=CARTESIAN_POINT('Ctrl Pts',(-31.6609177668595,23.4495923014496,7.17259908866064));
#62620=CARTESIAN_POINT('Ctrl Pts',(-31.6356608467856,23.4875505593778,7.15878341263018));
#62621=CARTESIAN_POINT('Ctrl Pts',(-31.5824397836614,23.5401211720794,7.13964927440967));
#62622=CARTESIAN_POINT('Ctrl Pts',(-31.5457246229044,23.5646010572896,7.1307393248549));
#62623=CARTESIAN_POINT('Ctrl Pts',(-31.4796949749373,23.5914894964812,7.12095273334326));
#62624=CARTESIAN_POINT('Ctrl Pts',(-31.4396270223971,23.5998331636539,7.11791588684779));
#62625=CARTESIAN_POINT('Ctrl Pts',(-31.4046869279001,23.6003888166983,7.11771364567905));
#62626=CARTESIAN_POINT('Origin',(-31.7,21.,7.));
#62627=CARTESIAN_POINT('Origin',(-29.,20.5,7.));
#62628=CARTESIAN_POINT('Origin',(-29.,21.5,7.));
#62629=CARTESIAN_POINT('Origin',(-31.7,21.,7.));
#62630=CARTESIAN_POINT('',(-31.7,23.6912516952905,7.08464226247173));
#62631=CARTESIAN_POINT('Origin',(-31.7,23.6912516952905,7.08464226247173));
#62632=CARTESIAN_POINT('Origin',(-50.,41.5,-36.5));
#62633=CARTESIAN_POINT('',(-35.6221012801966,49.1231323076242,-24.5));
#62634=CARTESIAN_POINT('',(-50.,49.1231323076242,-24.5));
#62635=CARTESIAN_POINT('',(-27.3778987198034,49.1231323076242,-24.5));
#62636=CARTESIAN_POINT('Origin',(-31.5,50.9282032302755,-21.6585366490161));
#62637=CARTESIAN_POINT('',(-50.,49.1231323076242,-24.5));
#62638=CARTESIAN_POINT('Origin',(-31.5,50.9282032302755,-35.7491074993019));
#62639=CARTESIAN_POINT('Origin',(-31.5,50.9282032302755,-24.5));
#62640=CARTESIAN_POINT('Origin',(-37.,54.4282032302755,-24.5));
#62641=CARTESIAN_POINT('',(0.,0.,0.));
#62642=CARTESIAN_POINT('Origin',(35.8,21.,6.000000094481));
#62643=CARTESIAN_POINT('',(35.8,21.,2.500000094481));
#62644=CARTESIAN_POINT('Origin',(35.8,21.,6.000000094481));
#62645=CARTESIAN_POINT('',(35.,21.,2.500000094481));
#62646=CARTESIAN_POINT('',(35.8,21.,2.500000094481));
#62647=CARTESIAN_POINT('Origin',(35.,21.,6.000000094481));
#62648=CARTESIAN_POINT('Origin',(36.41,21.,6.000000094481));
#62649=CARTESIAN_POINT('',(35.,21.,4.400000094481));
#62650=CARTESIAN_POINT('Origin',(35.,21.,6.000000094481));
#62651=CARTESIAN_POINT('',(35.8,21.,4.400000094481));
#62652=CARTESIAN_POINT('',(36.41,21.,4.400000094481));
#62653=CARTESIAN_POINT('Origin',(35.8,21.,6.000000094481));
#62654=CARTESIAN_POINT('Origin',(35.,21.,6.000000094481));
#62655=CARTESIAN_POINT('Origin',(35.8,21.,6.000000094481));
#62656=CARTESIAN_POINT('',(0.,0.,0.));
#62657=CARTESIAN_POINT('Origin',(0.,51.8,23.999999203644));
#62658=CARTESIAN_POINT('',(3.12478456555985,51.8,23.6022286430957));
#62659=CARTESIAN_POINT('',(3.12421373757276,51.8,24.4022286430957));
#62660=CARTESIAN_POINT('Origin',(0.,51.8,23.999999203644));
#62661=CARTESIAN_POINT('',(3.32630103585967,52.,23.6022286430957));
#62662=CARTESIAN_POINT('Ctrl Pts',(3.32630103585966,52.,23.6022286430957));
#62663=CARTESIAN_POINT('Ctrl Pts',(3.30138091333298,52.,23.6022286430957));
#62664=CARTESIAN_POINT('Ctrl Pts',(3.2720456700574,51.9941946996912,23.6022286430957));
#62665=CARTESIAN_POINT('Ctrl Pts',(3.22604606522074,51.9752251584662,23.6022286430957));
#62666=CARTESIAN_POINT('Ctrl Pts',(3.20122053120427,51.9587321016509,23.6022286430957));
#62667=CARTESIAN_POINT('Ctrl Pts',(3.1660925751105,51.9237716124592,23.6022286430957));
#62668=CARTESIAN_POINT('Ctrl Pts',(3.14954178912886,51.8991500075979,23.6022286430957));
#62669=CARTESIAN_POINT('Ctrl Pts',(3.13058236701996,51.853593258103,23.6022286430957));
#62670=CARTESIAN_POINT('Ctrl Pts',(3.12478456555985,51.8246216782777,23.6022286430957));
#62671=CARTESIAN_POINT('Ctrl Pts',(3.12478456555985,51.8,23.6022286430957));
#62672=CARTESIAN_POINT('',(3.32576479595873,52.,24.4022286430957));
#62673=CARTESIAN_POINT('Origin',(0.,52.,23.999999203644));
#62674=CARTESIAN_POINT('Ctrl Pts',(3.12421373757277,51.8,24.4022286430957));
#62675=CARTESIAN_POINT('Ctrl Pts',(3.12421373757277,51.824620291812,24.4022286430957));
#62676=CARTESIAN_POINT('Ctrl Pts',(3.13001197949707,51.8535900867339,24.4022286430957));
#62677=CARTESIAN_POINT('Ctrl Pts',(3.1489729516324,51.8991456790208,24.4022286430957));
#62678=CARTESIAN_POINT('Ctrl Pts',(3.16552590642155,51.9237671470348,24.4022286430957));
#62679=CARTESIAN_POINT('Ctrl Pts',(3.20065890912318,51.9587288606451,24.4022286430957));
#62680=CARTESIAN_POINT('Ctrl Pts',(3.2254889592639,51.9752227683353,24.4022286430957));
#62681=CARTESIAN_POINT('Ctrl Pts',(3.27149750609936,51.9941940883332,24.4022286430957));
#62682=CARTESIAN_POINT('Ctrl Pts',(3.30083925571873,52.,24.4022286430957));
#62683=CARTESIAN_POINT('Ctrl Pts',(3.32576479595873,52.,24.4022286430957));
#62684=CARTESIAN_POINT('Origin',(3.30681662608079E-15,51.8,23.999999203644));
#62685=CARTESIAN_POINT('',(5.58585522379171,52.,23.6022286430957));
#62686=CARTESIAN_POINT('',(5.58553591681572,52.,24.4022286430957));
#62687=CARTESIAN_POINT('Origin',(3.30681662608079E-15,52.,23.999999203644));
#62688=CARTESIAN_POINT('',(5.78634414645043,51.8,23.6022286430957));
#62689=CARTESIAN_POINT('Ctrl Pts',(5.78634414645042,51.8,23.6022286430957));
#62690=CARTESIAN_POINT('Ctrl Pts',(5.78634414645042,51.8246637229722,23.6022286430957));
#62691=CARTESIAN_POINT('Ctrl Pts',(5.78056058173252,51.8536895954238,23.6022286430957));
#62692=CARTESIAN_POINT('Ctrl Pts',(5.76165032214247,51.8992805452974,23.6022286430957));
#62693=CARTESIAN_POINT('Ctrl Pts',(5.74516733469338,51.923905255687,23.6022286430957));
#62694=CARTESIAN_POINT('Ctrl Pts',(5.71019378482186,51.958828241931,23.6022286430957));
#62695=CARTESIAN_POINT('Ctrl Pts',(5.68550434648015,51.9752951055667,23.6022286430957));
#62696=CARTESIAN_POINT('Ctrl Pts',(5.63976742956776,51.9942130655933,23.6022286430957));
#62697=CARTESIAN_POINT('Ctrl Pts',(5.61061936503537,52.,23.6022286430957));
#62698=CARTESIAN_POINT('Ctrl Pts',(5.58585522379171,52.,23.6022286430957));
#62699=CARTESIAN_POINT('',(5.78603590362507,51.8,24.4022286430957));
#62700=CARTESIAN_POINT('Origin',(3.30681662608079E-15,51.8,23.999999203644));
#62701=CARTESIAN_POINT('Ctrl Pts',(5.58553591681572,52.,24.4022286430957));
#62702=CARTESIAN_POINT('Ctrl Pts',(5.61030190157576,52.,24.4022286430957));
#62703=CARTESIAN_POINT('Ctrl Pts',(5.63945218333164,51.9942128733221,24.4022286430957));
#62704=CARTESIAN_POINT('Ctrl Pts',(5.68519202491141,51.9752943110313,24.4022286430957));
#62705=CARTESIAN_POINT('Ctrl Pts',(5.70988286438085,51.9588271924047,24.4022286430957));
#62706=CARTESIAN_POINT('Ctrl Pts',(5.7448579281656,51.9239038363323,24.4022286430957));
#62707=CARTESIAN_POINT('Ctrl Pts',(5.76134153541181,51.8992791894732,24.4022286430957));
#62708=CARTESIAN_POINT('Ctrl Pts',(5.78025222289073,51.8536886182006,24.4022286430957));
#62709=CARTESIAN_POINT('Ctrl Pts',(5.78603590362507,51.8246632938888,24.4022286430957));
#62710=CARTESIAN_POINT('Ctrl Pts',(5.78603590362507,51.8,24.4022286430957));
#62711=CARTESIAN_POINT('Origin',(3.30681662608079E-15,50.6,23.999999203644));
#62712=CARTESIAN_POINT('',(5.78634414645043,50.6,23.6022286430957));
#62713=CARTESIAN_POINT('',(5.78603590362507,50.6,24.4022286430957));
#62714=CARTESIAN_POINT('Origin',(3.30681662608079E-15,50.6,23.999999203644));
#62715=CARTESIAN_POINT('',(5.58585522379171,50.4,23.6022286430957));
#62716=CARTESIAN_POINT('Ctrl Pts',(5.5858552237917,50.4,23.6022286430957));
#62717=CARTESIAN_POINT('Ctrl Pts',(5.61061936503536,50.4,23.6022286430957));
#62718=CARTESIAN_POINT('Ctrl Pts',(5.63976742956776,50.4057869344067,23.6022286430957));
#62719=CARTESIAN_POINT('Ctrl Pts',(5.68550434648015,50.4247048944333,23.6022286430957));
#62720=CARTESIAN_POINT('Ctrl Pts',(5.71019378482186,50.441171758069,23.6022286430957));
#62721=CARTESIAN_POINT('Ctrl Pts',(5.74516733469338,50.476094744313,23.6022286430957));
#62722=CARTESIAN_POINT('Ctrl Pts',(5.76165032214247,50.5007194547026,23.6022286430957));
#62723=CARTESIAN_POINT('Ctrl Pts',(5.78056058173252,50.5463104045762,23.6022286430957));
#62724=CARTESIAN_POINT('Ctrl Pts',(5.78634414645042,50.5753362770278,23.6022286430957));
#62725=CARTESIAN_POINT('Ctrl Pts',(5.78634414645042,50.6,23.6022286430957));
#62726=CARTESIAN_POINT('',(5.58553591681572,50.4,24.4022286430957));
#62727=CARTESIAN_POINT('Origin',(3.30681662608079E-15,50.4,23.999999203644));
#62728=CARTESIAN_POINT('Ctrl Pts',(5.78603590362507,50.6,24.4022286430957));
#62729=CARTESIAN_POINT('Ctrl Pts',(5.78603590362507,50.5753367061112,24.4022286430957));
#62730=CARTESIAN_POINT('Ctrl Pts',(5.78025222289073,50.5463113817994,24.4022286430957));
#62731=CARTESIAN_POINT('Ctrl Pts',(5.76134153541181,50.5007208105268,24.4022286430957));
#62732=CARTESIAN_POINT('Ctrl Pts',(5.7448579281656,50.4760961636677,24.4022286430957));
#62733=CARTESIAN_POINT('Ctrl Pts',(5.70988286438085,50.4411728075953,24.4022286430957));
#62734=CARTESIAN_POINT('Ctrl Pts',(5.68519202491141,50.4247056889687,24.4022286430957));
#62735=CARTESIAN_POINT('Ctrl Pts',(5.63945218333164,50.4057871266779,24.4022286430957));
#62736=CARTESIAN_POINT('Ctrl Pts',(5.61030190157576,50.4,24.4022286430957));
#62737=CARTESIAN_POINT('Ctrl Pts',(5.58553591681572,50.4,24.4022286430957));
#62738=CARTESIAN_POINT('Origin',(0.,50.6,23.999999203644));
#62739=CARTESIAN_POINT('',(3.32630103585967,50.4,23.6022286430957));
#62740=CARTESIAN_POINT('',(3.32576479595873,50.4,24.4022286430957));
#62741=CARTESIAN_POINT('Origin',(0.,50.4,23.999999203644));
#62742=CARTESIAN_POINT('',(3.12478456555985,50.6,23.6022286430957));
#62743=CARTESIAN_POINT('Ctrl Pts',(3.12478456555985,50.6,23.6022286430957));
#62744=CARTESIAN_POINT('Ctrl Pts',(3.12478456555985,50.5753783217223,23.6022286430957));
#62745=CARTESIAN_POINT('Ctrl Pts',(3.13058236701996,50.546406741897,23.6022286430957));
#62746=CARTESIAN_POINT('Ctrl Pts',(3.14954178912886,50.5008499924022,23.6022286430957));
#62747=CARTESIAN_POINT('Ctrl Pts',(3.1660925751105,50.4762283875408,23.6022286430957));
#62748=CARTESIAN_POINT('Ctrl Pts',(3.20122053120427,50.4412678983491,23.6022286430957));
#62749=CARTESIAN_POINT('Ctrl Pts',(3.22604606522074,50.4247748415338,23.6022286430957));
#62750=CARTESIAN_POINT('Ctrl Pts',(3.2720456700574,50.4058053003088,23.6022286430957));
#62751=CARTESIAN_POINT('Ctrl Pts',(3.30138091333298,50.4,23.6022286430957));
#62752=CARTESIAN_POINT('Ctrl Pts',(3.32630103585966,50.4,23.6022286430957));
#62753=CARTESIAN_POINT('',(3.12421373757276,50.6,24.4022286430957));
#62754=CARTESIAN_POINT('Origin',(0.,50.6,23.999999203644));
#62755=CARTESIAN_POINT('Ctrl Pts',(3.32576479595873,50.4,24.4022286430957));
#62756=CARTESIAN_POINT('Ctrl Pts',(3.30083925571873,50.4,24.4022286430957));
#62757=CARTESIAN_POINT('Ctrl Pts',(3.27149750609936,50.4058059116668,24.4022286430957));
#62758=CARTESIAN_POINT('Ctrl Pts',(3.2254889592639,50.4247772316647,24.4022286430957));
#62759=CARTESIAN_POINT('Ctrl Pts',(3.20065890912318,50.4412711393549,24.4022286430957));
#62760=CARTESIAN_POINT('Ctrl Pts',(3.16552590642155,50.4762328529652,24.4022286430957));
#62761=CARTESIAN_POINT('Ctrl Pts',(3.1489729516324,50.5008543209792,24.4022286430957));
#62762=CARTESIAN_POINT('Ctrl Pts',(3.13001197949707,50.5464099132661,24.4022286430957));
#62763=CARTESIAN_POINT('Ctrl Pts',(3.12421373757277,50.575379708188,24.4022286430957));
#62764=CARTESIAN_POINT('Ctrl Pts',(3.12421373757277,50.6,24.4022286430957));
#62765=CARTESIAN_POINT('Origin',(3.30681662608079E-15,52.,23.999999203644));
#62766=CARTESIAN_POINT('',(5.78603590362507,52.,24.4022286430957));
#62767=CARTESIAN_POINT('',(3.12478456555985,52.,23.6022286430957));
#62768=CARTESIAN_POINT('Origin',(3.30681662608079E-15,50.4,23.999999203644));
#62769=CARTESIAN_POINT('',(5.78603590362507,50.4,24.4022286430957));
#62770=CARTESIAN_POINT('',(3.12478456555985,50.4,23.6022286430957));
#62771=CARTESIAN_POINT('Origin',(0.,50.4,23.999999203644));
#62772=CARTESIAN_POINT('',(3.12478456555985,50.4,23.6022286430957));
#62773=CARTESIAN_POINT('',(3.12421373757276,50.4,24.4022286430957));
#62774=CARTESIAN_POINT('Origin',(3.30681662608079E-15,50.4,23.999999203644));
#62775=CARTESIAN_POINT('',(5.78634414645043,50.4,23.6022286430957));
#62776=CARTESIAN_POINT('',(5.78603590362507,50.4,24.4022286430957));
#62777=CARTESIAN_POINT('Origin',(3.12478456555985,50.4,23.6022286430957));
#62778=CARTESIAN_POINT('Origin',(5.78603590362507,50.4,24.4022286430957));
#62779=CARTESIAN_POINT('',(0.,0.,0.));
#62780=CARTESIAN_POINT('Origin',(-2.00081E-7,47.4,24.));
#62781=CARTESIAN_POINT('',(-2.00080999566319E-7,48.8433756729741,24.));
#62782=CARTESIAN_POINT('',(-2.00081E-7,47.4,21.5));
#62783=CARTESIAN_POINT('',(-2.00080999693838E-7,47.4,21.5));
#62784=CARTESIAN_POINT('',(2.16506330938012,47.4,22.75));
#62785=CARTESIAN_POINT('Origin',(-2.00081E-7,47.4,24.));
#62786=CARTESIAN_POINT('',(2.16506330938012,47.4,25.25));
#62787=CARTESIAN_POINT('Origin',(-2.00081E-7,47.4,24.));
#62788=CARTESIAN_POINT('',(-2.00081E-7,47.4,26.5));
#62789=CARTESIAN_POINT('Origin',(-2.00081E-7,47.4,24.));
#62790=CARTESIAN_POINT('',(-2.16506370954212,47.4,25.25));
#62791=CARTESIAN_POINT('Origin',(-2.00081E-7,47.4,24.));
#62792=CARTESIAN_POINT('',(-2.16506370954212,47.4,22.75));
#62793=CARTESIAN_POINT('Origin',(-2.00081E-7,47.4,24.));
#62794=CARTESIAN_POINT('Origin',(-2.00081E-7,47.4,24.));
#62795=CARTESIAN_POINT('Origin',(-2.00081E-7,44.4,24.));
#62796=CARTESIAN_POINT('',(1.42982496405621,44.4,26.5));
#62797=CARTESIAN_POINT('',(-1.42982536421821,44.4,26.5));
#62798=CARTESIAN_POINT('Ctrl Pts',(-1.42982536421823,44.4,26.5));
#62799=CARTESIAN_POINT('Ctrl Pts',(-2.00081006429542E-7,44.8098385035873,
26.5));
#62800=CARTESIAN_POINT('Ctrl Pts',(1.42982496405621,44.4,26.5));
#62801=CARTESIAN_POINT('Origin',(-2.00081E-7,44.4,24.));
#62802=CARTESIAN_POINT('Origin',(-2.00081E-7,45.0000000000001,24.));
#62803=CARTESIAN_POINT('',(-2.00080999461155E-7,44.4,19.6));
#62804=CARTESIAN_POINT('Origin',(-2.00081E-7,44.4,24.));
#62805=CARTESIAN_POINT('',(-2.00080999387677E-7,45.,19.));
#62806=CARTESIAN_POINT('Origin',(-2.00080999461155E-7,45.0000000000001,
19.6000000000001));
#62807=CARTESIAN_POINT('',(-2.00080999387677E-7,45.,29.));
#62808=CARTESIAN_POINT('Origin',(-2.00081E-7,45.,24.));
#62809=CARTESIAN_POINT('Origin',(-2.00081E-7,45.,24.));
#62810=CARTESIAN_POINT('Origin',(-2.00081E-7,62.4,24.));
#62811=CARTESIAN_POINT('',(-2.00081000612323E-7,50.4,29.));
#62812=CARTESIAN_POINT('',(-2.00081000612323E-7,62.4,29.));
#62813=CARTESIAN_POINT('Origin',(-2.00081E-7,50.4,24.));
#62814=CARTESIAN_POINT('Origin',(-2.00081E-7,51.0799999999998,24.));
#62815=CARTESIAN_POINT('',(-2.00080999630898E-7,50.9976569609204,20.9860500453614));
#62816=CARTESIAN_POINT('Origin',(-2.00081E-7,50.9976569609204,24.));
#62817=CARTESIAN_POINT('',(-2.00080999632606E-7,51.0799999999998,21.));
#62818=CARTESIAN_POINT('Origin',(-2.0008099960199E-7,51.0799999999998,20.7500000000018));
#62819=CARTESIAN_POINT('',(-2.00080999632606E-7,51.0799999999998,27.));
#62820=CARTESIAN_POINT('Origin',(-2.00081E-7,51.0799999999998,24.));
#62821=CARTESIAN_POINT('Origin',(-2.00081E-7,51.0799999999998,24.));
#62822=CARTESIAN_POINT('Origin',(-2.00081E-7,62.4,24.));
#62823=CARTESIAN_POINT('',(-2.00081000367394E-7,61.7865,27.));
#62824=CARTESIAN_POINT('',(-2.00081000367394E-7,62.4,27.));
#62825=CARTESIAN_POINT('',(-2.00081000367394E-7,61.7865,21.));
#62826=CARTESIAN_POINT('Origin',(-2.00081E-7,61.7865,24.));
#62827=CARTESIAN_POINT('Origin',(-2.00081E-7,61.7865,24.));
#62828=CARTESIAN_POINT('Origin',(-2.00081E-7,50.6499999999998,24.));
#62829=CARTESIAN_POINT('',(-2.0008099958362E-7,50.4,20.6));
#62830=CARTESIAN_POINT('Origin',(-2.00081E-7,50.4,24.));
#62831=CARTESIAN_POINT('',(-2.00080999612528E-7,50.5676569609204,20.8360500453614));
#62832=CARTESIAN_POINT('Origin',(-2.0008099958362E-7,50.6499999999998,20.6000000000001));
#62833=CARTESIAN_POINT('Origin',(-2.00081E-7,50.5676569609204,24.));
#62834=CARTESIAN_POINT('Origin',(-2.00081E-7,61.7865,24.));
#62835=CARTESIAN_POINT('',(-2.00080999707738E-7,62.4,21.6135));
#62836=CARTESIAN_POINT('',(-2.00080999632606E-7,61.7865,21.));
#62837=CARTESIAN_POINT('Origin',(-2.00081E-7,62.4,24.));
#62838=CARTESIAN_POINT('Origin',(-2.00081E-7,50.9976569609204,24.));
#62839=CARTESIAN_POINT('',(-2.00080999630898E-7,50.9976569609204,20.9860500453614));
#62840=CARTESIAN_POINT('Origin',(-2.00081E-7,62.4,21.6135));
#62841=CARTESIAN_POINT('Origin',(-2.00081E-7,44.4,24.));
#62842=CARTESIAN_POINT('',(-1.42982536421821,44.4,21.5));
#62843=CARTESIAN_POINT('',(1.42982496405621,44.4,21.5));
#62844=CARTESIAN_POINT('Ctrl Pts',(-1.42982536421821,44.4,21.5));
#62845=CARTESIAN_POINT('Ctrl Pts',(-2.00081004042563E-7,44.8098385035873,
21.5));
#62846=CARTESIAN_POINT('Ctrl Pts',(1.4298249640562,44.4,21.5));
#62847=CARTESIAN_POINT('Origin',(-2.00081E-7,44.4,24.));
#62848=CARTESIAN_POINT('Origin',(-2.00081E-7,44.4,24.));
#62849=CARTESIAN_POINT('',(-2.8799762916107,44.4,23.9882649151131));
#62850=CARTESIAN_POINT('',(-1.45015112747354,44.4,21.511735084887));
#62851=CARTESIAN_POINT('Ctrl Pts',(-2.87997629161071,44.4,23.9882649151131));
#62852=CARTESIAN_POINT('Ctrl Pts',(-2.16506370954213,44.8098385035873,22.7500000000001));
#62853=CARTESIAN_POINT('Ctrl Pts',(-1.45015112747356,44.4,21.511735084887));
#62854=CARTESIAN_POINT('Origin',(-2.00081E-7,44.4,24.));
#62855=CARTESIAN_POINT('Origin',(-2.00081E-7,44.4,24.));
#62856=CARTESIAN_POINT('',(1.45015072731155,44.4,21.511735084887));
#62857=CARTESIAN_POINT('',(2.8799758914487,44.4,23.9882649151131));
#62858=CARTESIAN_POINT('Ctrl Pts',(1.45015072731154,44.4,21.511735084887));
#62859=CARTESIAN_POINT('Ctrl Pts',(2.16506330938013,44.8098385035873,22.75));
#62860=CARTESIAN_POINT('Ctrl Pts',(2.8799758914487,44.4,23.9882649151131));
#62861=CARTESIAN_POINT('Origin',(-2.00081E-7,44.4,24.));
#62862=CARTESIAN_POINT('Origin',(-2.500000200081,47.4,24.));
#62863=CARTESIAN_POINT('',(-1.4433758730551,47.4,26.5));
#62864=CARTESIAN_POINT('',(-2.8867515460291,47.4,24.));
#62865=CARTESIAN_POINT('',(-1.4433758730551,47.4,26.5));
#62866=CARTESIAN_POINT('Origin',(-2.00081E-7,44.4,24.));
#62867=CARTESIAN_POINT('',(-1.45015112747355,44.4,26.488264915113));
#62868=CARTESIAN_POINT('',(-2.8799762916107,44.4,24.0117350848869));
#62869=CARTESIAN_POINT('Ctrl Pts',(-1.45015112747355,44.4,26.488264915113));
#62870=CARTESIAN_POINT('Ctrl Pts',(-2.16506370954212,44.8098385035873,25.25));
#62871=CARTESIAN_POINT('Ctrl Pts',(-2.8799762916107,44.4,24.0117350848869));
#62872=CARTESIAN_POINT('Origin',(-2.00081E-7,44.4,24.));
#62873=CARTESIAN_POINT('Origin',(-2.00081E-7,44.4,24.));
#62874=CARTESIAN_POINT('',(2.8799758914487,44.4,24.0117350848869));
#62875=CARTESIAN_POINT('',(1.45015072731154,44.4,26.488264915113));
#62876=CARTESIAN_POINT('Ctrl Pts',(2.8799758914487,44.4,24.0117350848869));
#62877=CARTESIAN_POINT('Ctrl Pts',(2.16506330938012,44.8098385035873,25.25));
#62878=CARTESIAN_POINT('Ctrl Pts',(1.45015072731155,44.4,26.488264915113));
#62879=CARTESIAN_POINT('Origin',(-2.00081E-7,44.4,24.));
#62880=CARTESIAN_POINT('Origin',(-2.500000200081,47.4,24.));
#62881=CARTESIAN_POINT('',(1.4433754728931,47.4,26.5));
#62882=CARTESIAN_POINT('',(-1.4433758730551,47.4,26.5));
#62883=CARTESIAN_POINT('',(1.4433754728931,47.4,26.5));
#62884=CARTESIAN_POINT('Origin',(-2.500000200081,47.4,24.));
#62885=CARTESIAN_POINT('',(2.8867511458671,47.4,24.));
#62886=CARTESIAN_POINT('',(1.4433754728931,47.4,26.5));
#62887=CARTESIAN_POINT('',(2.8867511458671,47.4,24.));
#62888=CARTESIAN_POINT('Origin',(-2.00081E-7,50.4,19.));
#62889=CARTESIAN_POINT('Origin',(-1.4433758730551,47.4,26.5));
#62890=CARTESIAN_POINT('',(-1.4433758730551,44.4,26.5));
#62891=CARTESIAN_POINT('',(-1.4433758730551,44.4,26.5));
#62892=CARTESIAN_POINT('',(-1.4433758730551,47.4,26.5));
#62893=CARTESIAN_POINT('',(1.4433754728931,44.4,26.5));
#62894=CARTESIAN_POINT('',(1.4433754728931,47.4,26.5));
#62895=CARTESIAN_POINT('',(-2.00081E-7,44.4,26.5));
#62896=CARTESIAN_POINT('Origin',(1.4433754728931,47.4,26.5));
#62897=CARTESIAN_POINT('',(1.4433754728931,44.4,26.5));
#62898=CARTESIAN_POINT('',(2.8867511458671,44.4,24.));
#62899=CARTESIAN_POINT('',(2.8867511458671,47.4,24.));
#62900=CARTESIAN_POINT('',(2.16506330938012,44.4,25.25));
#62901=CARTESIAN_POINT('Origin',(2.8867511458671,47.4,24.));
#62902=CARTESIAN_POINT('',(2.8867511458671,44.4,24.));
#62903=CARTESIAN_POINT('',(1.4433754728931,47.4,21.5));
#62904=CARTESIAN_POINT('',(2.8867511458671,47.4,24.));
#62905=CARTESIAN_POINT('',(1.4433754728931,44.4,21.5));
#62906=CARTESIAN_POINT('',(1.4433754728931,47.4,21.5));
#62907=CARTESIAN_POINT('',(2.16506330938012,44.4,22.75));
#62908=CARTESIAN_POINT('Origin',(1.4433754728931,47.4,21.5));
#62909=CARTESIAN_POINT('',(1.4433754728931,44.4,21.5));
#62910=CARTESIAN_POINT('',(1.4433754728931,47.4,21.5));
#62911=CARTESIAN_POINT('',(-1.4433758730551,47.4,21.5));
#62912=CARTESIAN_POINT('',(1.4433754728931,47.4,21.5));
#62913=CARTESIAN_POINT('',(-1.4433758730551,44.4,21.5));
#62914=CARTESIAN_POINT('',(-1.4433758730551,47.4,21.5));
#62915=CARTESIAN_POINT('',(-2.00081E-7,44.4,21.5));
#62916=CARTESIAN_POINT('Origin',(-2.8867515460291,47.4,24.));
#62917=CARTESIAN_POINT('',(-2.8867515460291,44.4,24.));
#62918=CARTESIAN_POINT('',(-2.8867515460291,44.4,24.));
#62919=CARTESIAN_POINT('',(-2.8867515460291,47.4,24.));
#62920=CARTESIAN_POINT('',(-2.8867515460291,47.4,24.));
#62921=CARTESIAN_POINT('',(-2.8867515460291,47.4,24.));
#62922=CARTESIAN_POINT('',(-2.16506370954212,44.4,25.25));
#62923=CARTESIAN_POINT('Origin',(-1.4433758730551,47.4,21.5));
#62924=CARTESIAN_POINT('',(-1.4433758730551,44.4,21.5));
#62925=CARTESIAN_POINT('',(-1.4433758730551,47.4,21.5));
#62926=CARTESIAN_POINT('',(-1.4433758730551,47.4,21.5));
#62927=CARTESIAN_POINT('',(-2.16506370954212,44.4,22.75));
#62928=CARTESIAN_POINT('Origin',(-2.500000200081,47.4,24.));
#62929=CARTESIAN_POINT('Origin',(-2.500000200081,47.4,24.));
#62930=CARTESIAN_POINT('Origin',(-2.00081E-7,44.4,24.));
#62931=CARTESIAN_POINT('Origin',(-2.500000200081,47.4,24.));
#62932=CARTESIAN_POINT('',(0.,0.,0.));
#62933=CARTESIAN_POINT('',(0.,0.,0.));
#62934=CARTESIAN_POINT('',(0.,0.,0.));
#62935=CARTESIAN_POINT('',(0.,0.,0.));
#62936=CARTESIAN_POINT('',(0.,0.,0.));
#62937=CARTESIAN_POINT('',(0.,0.,0.));
#62938=CARTESIAN_POINT('',(0.,0.,0.));
#62939=CARTESIAN_POINT('',(0.,0.,0.));
#62940=CARTESIAN_POINT('',(0.,0.,0.));
#62941=CARTESIAN_POINT('',(0.,0.,0.));
#62942=CARTESIAN_POINT('',(0.,0.,0.));
#62943=CARTESIAN_POINT('',(0.,0.,0.));
#62944=CARTESIAN_POINT('',(-21.6241260836584,97.0988789235201,41.6228028588816));
#62945=CARTESIAN_POINT('',(6.93889390390723E-15,0.,-47.999999203644));
#62946=CARTESIAN_POINT('',(0.123196188190229,-6.93889390390723E-15,-47.9185269563116));
#62947=UNCERTAINTY_MEASURE_WITH_UNIT(LENGTH_MEASURE(0.01),#62975,
'DISTANCE_ACCURACY_VALUE',
'Maximum model space distance between geometric entities at asserted c
onnectivities');
#62948=UNCERTAINTY_MEASURE_WITH_UNIT(LENGTH_MEASURE(0.01),#62975,
'DISTANCE_ACCURACY_VALUE',
'Maximum model space distance between geometric entities at asserted c
onnectivities');
#62949=UNCERTAINTY_MEASURE_WITH_UNIT(LENGTH_MEASURE(0.01),#62975,
'DISTANCE_ACCURACY_VALUE',
'Maximum model space distance between geometric entities at asserted c
onnectivities');
#62950=UNCERTAINTY_MEASURE_WITH_UNIT(LENGTH_MEASURE(0.01),#62975,
'DISTANCE_ACCURACY_VALUE',
'Maximum model space distance between geometric entities at asserted c
onnectivities');
#62951=UNCERTAINTY_MEASURE_WITH_UNIT(LENGTH_MEASURE(0.01),#62975,
'DISTANCE_ACCURACY_VALUE',
'Maximum model space distance between geometric entities at asserted c
onnectivities');
#62952=UNCERTAINTY_MEASURE_WITH_UNIT(LENGTH_MEASURE(0.01),#62975,
'DISTANCE_ACCURACY_VALUE',
'Maximum model space distance between geometric entities at asserted c
onnectivities');
#62953=UNCERTAINTY_MEASURE_WITH_UNIT(LENGTH_MEASURE(0.01),#62975,
'DISTANCE_ACCURACY_VALUE',
'Maximum model space distance between geometric entities at asserted c
onnectivities');
#62954=UNCERTAINTY_MEASURE_WITH_UNIT(LENGTH_MEASURE(0.01),#62975,
'DISTANCE_ACCURACY_VALUE',
'Maximum model space distance between geometric entities at asserted c
onnectivities');
#62955=UNCERTAINTY_MEASURE_WITH_UNIT(LENGTH_MEASURE(0.01),#62975,
'DISTANCE_ACCURACY_VALUE',
'Maximum model space distance between geometric entities at asserted c
onnectivities');
#62956=UNCERTAINTY_MEASURE_WITH_UNIT(LENGTH_MEASURE(0.01),#62975,
'DISTANCE_ACCURACY_VALUE',
'Maximum model space distance between geometric entities at asserted c
onnectivities');
#62957=UNCERTAINTY_MEASURE_WITH_UNIT(LENGTH_MEASURE(0.01),#62975,
'DISTANCE_ACCURACY_VALUE',
'Maximum model space distance between geometric entities at asserted c
onnectivities');
#62958=UNCERTAINTY_MEASURE_WITH_UNIT(LENGTH_MEASURE(0.01),#62975,
'DISTANCE_ACCURACY_VALUE',
'Maximum model space distance between geometric entities at asserted c
onnectivities');
#62959=UNCERTAINTY_MEASURE_WITH_UNIT(LENGTH_MEASURE(0.01),#62975,
'DISTANCE_ACCURACY_VALUE',
'Maximum model space distance between geometric entities at asserted c
onnectivities');
#62960=UNCERTAINTY_MEASURE_WITH_UNIT(LENGTH_MEASURE(0.01),#62975,
'DISTANCE_ACCURACY_VALUE',
'Maximum model space distance between geometric entities at asserted c
onnectivities');
#62961=(
GEOMETRIC_REPRESENTATION_CONTEXT(3)
GLOBAL_UNCERTAINTY_ASSIGNED_CONTEXT((#62947))
GLOBAL_UNIT_ASSIGNED_CONTEXT((#62975,#62977,#62978))
REPRESENTATION_CONTEXT('','3D')
);
#62962=(
GEOMETRIC_REPRESENTATION_CONTEXT(3)
GLOBAL_UNCERTAINTY_ASSIGNED_CONTEXT((#62948))
GLOBAL_UNIT_ASSIGNED_CONTEXT((#62975,#62977,#62978))
REPRESENTATION_CONTEXT('','3D')
);
#62963=(
GEOMETRIC_REPRESENTATION_CONTEXT(3)
GLOBAL_UNCERTAINTY_ASSIGNED_CONTEXT((#62949))
GLOBAL_UNIT_ASSIGNED_CONTEXT((#62975,#62977,#62978))
REPRESENTATION_CONTEXT('','3D')
);
#62964=(
GEOMETRIC_REPRESENTATION_CONTEXT(3)
GLOBAL_UNCERTAINTY_ASSIGNED_CONTEXT((#62950))
GLOBAL_UNIT_ASSIGNED_CONTEXT((#62975,#62977,#62978))
REPRESENTATION_CONTEXT('','3D')
);
#62965=(
GEOMETRIC_REPRESENTATION_CONTEXT(3)
GLOBAL_UNCERTAINTY_ASSIGNED_CONTEXT((#62951))
GLOBAL_UNIT_ASSIGNED_CONTEXT((#62975,#62977,#62978))
REPRESENTATION_CONTEXT('','3D')
);
#62966=(
GEOMETRIC_REPRESENTATION_CONTEXT(3)
GLOBAL_UNCERTAINTY_ASSIGNED_CONTEXT((#62952))
GLOBAL_UNIT_ASSIGNED_CONTEXT((#62975,#62977,#62978))
REPRESENTATION_CONTEXT('','3D')
);
#62967=(
GEOMETRIC_REPRESENTATION_CONTEXT(3)
GLOBAL_UNCERTAINTY_ASSIGNED_CONTEXT((#62953))
GLOBAL_UNIT_ASSIGNED_CONTEXT((#62975,#62977,#62978))
REPRESENTATION_CONTEXT('','3D')
);
#62968=(
GEOMETRIC_REPRESENTATION_CONTEXT(3)
GLOBAL_UNCERTAINTY_ASSIGNED_CONTEXT((#62954))
GLOBAL_UNIT_ASSIGNED_CONTEXT((#62975,#62977,#62978))
REPRESENTATION_CONTEXT('','3D')
);
#62969=(
GEOMETRIC_REPRESENTATION_CONTEXT(3)
GLOBAL_UNCERTAINTY_ASSIGNED_CONTEXT((#62955))
GLOBAL_UNIT_ASSIGNED_CONTEXT((#62975,#62977,#62978))
REPRESENTATION_CONTEXT('','3D')
);
#62970=(
GEOMETRIC_REPRESENTATION_CONTEXT(3)
GLOBAL_UNCERTAINTY_ASSIGNED_CONTEXT((#62956))
GLOBAL_UNIT_ASSIGNED_CONTEXT((#62975,#62977,#62978))
REPRESENTATION_CONTEXT('','3D')
);
#62971=(
GEOMETRIC_REPRESENTATION_CONTEXT(3)
GLOBAL_UNCERTAINTY_ASSIGNED_CONTEXT((#62957))
GLOBAL_UNIT_ASSIGNED_CONTEXT((#62975,#62977,#62978))
REPRESENTATION_CONTEXT('','3D')
);
#62972=(
GEOMETRIC_REPRESENTATION_CONTEXT(3)
GLOBAL_UNCERTAINTY_ASSIGNED_CONTEXT((#62958))
GLOBAL_UNIT_ASSIGNED_CONTEXT((#62975,#62977,#62978))
REPRESENTATION_CONTEXT('','3D')
);
#62973=(
GEOMETRIC_REPRESENTATION_CONTEXT(3)
GLOBAL_UNCERTAINTY_ASSIGNED_CONTEXT((#62959))
GLOBAL_UNIT_ASSIGNED_CONTEXT((#62975,#62977,#62978))
REPRESENTATION_CONTEXT('','3D')
);
#62974=(
GEOMETRIC_REPRESENTATION_CONTEXT(3)
GLOBAL_UNCERTAINTY_ASSIGNED_CONTEXT((#62960))
GLOBAL_UNIT_ASSIGNED_CONTEXT((#62975,#62977,#62978))
REPRESENTATION_CONTEXT('','3D')
);
#62975=(
LENGTH_UNIT()
NAMED_UNIT(*)
SI_UNIT(.MILLI.,.METRE.)
);
#62976=(
LENGTH_UNIT()
NAMED_UNIT(*)
SI_UNIT($,.METRE.)
);
#62977=(
NAMED_UNIT(*)
PLANE_ANGLE_UNIT()
SI_UNIT($,.RADIAN.)
);
#62978=(
NAMED_UNIT(*)
SI_UNIT($,.STERADIAN.)
SOLID_ANGLE_UNIT()
);
#62979=SHAPE_DEFINITION_REPRESENTATION(#62992,#63020);
#62980=SHAPE_DEFINITION_REPRESENTATION(#62993,#63021);
#62981=SHAPE_DEFINITION_REPRESENTATION(#62994,#63022);
#62982=SHAPE_DEFINITION_REPRESENTATION(#62995,#63023);
#62983=SHAPE_DEFINITION_REPRESENTATION(#62996,#63024);
#62984=SHAPE_DEFINITION_REPRESENTATION(#62997,#63025);
#62985=SHAPE_DEFINITION_REPRESENTATION(#62998,#63026);
#62986=SHAPE_DEFINITION_REPRESENTATION(#62999,#63027);
#62987=SHAPE_DEFINITION_REPRESENTATION(#63000,#63028);
#62988=SHAPE_DEFINITION_REPRESENTATION(#63001,#63029);
#62989=SHAPE_DEFINITION_REPRESENTATION(#63002,#63030);
#62990=SHAPE_DEFINITION_REPRESENTATION(#63003,#63031);
#62991=SHAPE_DEFINITION_REPRESENTATION(#63004,#63032);
#62992=PRODUCT_DEFINITION_SHAPE('',$,#63034);
#62993=PRODUCT_DEFINITION_SHAPE('',$,#63035);
#62994=PRODUCT_DEFINITION_SHAPE('',$,#63036);
#62995=PRODUCT_DEFINITION_SHAPE('',$,#63037);
#62996=PRODUCT_DEFINITION_SHAPE('',$,#63038);
#62997=PRODUCT_DEFINITION_SHAPE('',$,#63039);
#62998=PRODUCT_DEFINITION_SHAPE('',$,#63040);
#62999=PRODUCT_DEFINITION_SHAPE('',$,#63041);
#63000=PRODUCT_DEFINITION_SHAPE('',$,#63042);
#63001=PRODUCT_DEFINITION_SHAPE('',$,#63043);
#63002=PRODUCT_DEFINITION_SHAPE('',$,#63044);
#63003=PRODUCT_DEFINITION_SHAPE('',$,#63045);
#63004=PRODUCT_DEFINITION_SHAPE('',$,#63046);
#63005=PRODUCT_DEFINITION_SHAPE($,$,#56);
#63006=PRODUCT_DEFINITION_SHAPE($,$,#57);
#63007=PRODUCT_DEFINITION_SHAPE($,$,#58);
#63008=PRODUCT_DEFINITION_SHAPE($,$,#59);
#63009=PRODUCT_DEFINITION_SHAPE($,$,#60);
#63010=PRODUCT_DEFINITION_SHAPE($,$,#61);
#63011=PRODUCT_DEFINITION_SHAPE($,$,#62);
#63012=PRODUCT_DEFINITION_SHAPE($,$,#63);
#63013=PRODUCT_DEFINITION_SHAPE($,$,#64);
#63014=PRODUCT_DEFINITION_SHAPE($,$,#65);
#63015=PRODUCT_DEFINITION_SHAPE($,$,#66);
#63016=PRODUCT_DEFINITION_SHAPE($,$,#67);
#63017=PRODUCT_DEFINITION_SHAPE($,$,#68);
#63018=PRODUCT_DEFINITION_SHAPE($,$,#69);
#63019=PRODUCT_DEFINITION_SHAPE($,$,#70);
#63020=SHAPE_REPRESENTATION('',(#15337,#16941,#16942,#16943,#16944,#16945,
#16946,#16947,#16948,#16949,#16950,#16951,#16952,#16953,#16954,#16955),
#62961);
#63021=SHAPE_REPRESENTATION('',(#15338),#62962);
#63022=SHAPE_REPRESENTATION('',(#15471),#62963);
#63023=SHAPE_REPRESENTATION('',(#15531),#62964);
#63024=SHAPE_REPRESENTATION('',(#15679),#62965);
#63025=SHAPE_REPRESENTATION('',(#15858),#62966);
#63026=SHAPE_REPRESENTATION('',(#16176),#62967);
#63027=SHAPE_REPRESENTATION('',(#16214),#62968);
#63028=SHAPE_REPRESENTATION('',(#16388),#62969);
#63029=SHAPE_REPRESENTATION('',(#16488),#62970);
#63030=SHAPE_REPRESENTATION('',(#16856),#62971);
#63031=SHAPE_REPRESENTATION('',(#16865),#62972);
#63032=SHAPE_REPRESENTATION('',(#16884),#62973);
#63033=PRODUCT_DEFINITION_CONTEXT('part definition',#63074,'design');
#63034=PRODUCT_DEFINITION('EFI',
'MAS-617',#63047,#63033);
#63035=PRODUCT_DEFINITION('Fuel Injector & Bracket',
'Fuel Injector & Bracket',#63048,#63033);
#63036=PRODUCT_DEFINITION('DIN 7985 M4x20','DIN 7985 M4x20',#63049,#63033);
#63037=PRODUCT_DEFINITION('Throttle Shaft & Butterfly Valve',
'Throttle Shaft & Butterfly Valve',#63050,#63033);
#63038=PRODUCT_DEFINITION('TPS - Throttle Position Sensor',
'TPS - Throttle Position Sensor',#63051,#63033);
#63039=PRODUCT_DEFINITION('Throttle Actuation Mechanism Spring',
'Throttle Actuation Mechanism Spring',#63052,#63033);
#63040=PRODUCT_DEFINITION('DIN 7985 M3x10','DIN 7985 M3x10',#63053,#63033);
#63041=PRODUCT_DEFINITION('MAP Sensor & Vacuum Tube',
'MAP Sensor & Vacuum Tube',#63054,#63033);
#63042=PRODUCT_DEFINITION('Intake Manifold Flange',
'Intake Manifold Flange',#63055,#63033);
#63043=PRODUCT_DEFINITION('Throttle Body Housing',
'Throttle Body Housing',#63056,#63033);
#63044=PRODUCT_DEFINITION('DIN 125','DIN 125',#63057,#63033);
#63045=PRODUCT_DEFINITION('DIN 127','DIN 127',#63058,#63033);
#63046=PRODUCT_DEFINITION('DIN 912 M6x12','DIN 912 M6x12',#63059,#63033);
#63047=PRODUCT_DEFINITION_FORMATION('',$,#63076);
#63048=PRODUCT_DEFINITION_FORMATION('',$,#63077);
#63049=PRODUCT_DEFINITION_FORMATION('',$,#63078);
#63050=PRODUCT_DEFINITION_FORMATION('',$,#63079);
#63051=PRODUCT_DEFINITION_FORMATION('',$,#63080);
#63052=PRODUCT_DEFINITION_FORMATION('',$,#63081);
#63053=PRODUCT_DEFINITION_FORMATION('',$,#63082);
#63054=PRODUCT_DEFINITION_FORMATION('',$,#63083);
#63055=PRODUCT_DEFINITION_FORMATION('',$,#63084);
#63056=PRODUCT_DEFINITION_FORMATION('',$,#63085);
#63057=PRODUCT_DEFINITION_FORMATION('',$,#63086);
#63058=PRODUCT_DEFINITION_FORMATION('',$,#63087);
#63059=PRODUCT_DEFINITION_FORMATION('',$,#63088);
#63060=PRODUCT_RELATED_PRODUCT_CATEGORY(
'MAS-617',
'MAS-617',(#63076));
#63061=PRODUCT_RELATED_PRODUCT_CATEGORY('Fuel Injector & Bracket',
'Fuel Injector & Bracket',(#63077));
#63062=PRODUCT_RELATED_PRODUCT_CATEGORY('DIN 7985 M4x20',
'DIN 7985 M4x20',(#63078));
#63063=PRODUCT_RELATED_PRODUCT_CATEGORY(
'Throttle Shaft & Butterfly Valve','Throttle Shaft & Butterfly Valve',(#63079));
#63064=PRODUCT_RELATED_PRODUCT_CATEGORY(
'TPS - Throttle Position Sensor','TPS - Throttle Position Sensor',(#63080));
#63065=PRODUCT_RELATED_PRODUCT_CATEGORY(
'Throttle Actuation Mechanism Spring',
'Throttle Actuation Mechanism Spring',(#63081));
#63066=PRODUCT_RELATED_PRODUCT_CATEGORY('DIN 7985 M3x10',
'DIN 7985 M3x10',(#63082));
#63067=PRODUCT_RELATED_PRODUCT_CATEGORY('MAP Sensor & Vacuum Tube',
'MAP Sensor & Vacuum Tube',(#63083));
#63068=PRODUCT_RELATED_PRODUCT_CATEGORY('Intake Manifold Flange',
'Intake Manifold Flange',(#63084));
#63069=PRODUCT_RELATED_PRODUCT_CATEGORY('Throttle Body Housing',
'Throttle Body Housing',(#63085));
#63070=PRODUCT_RELATED_PRODUCT_CATEGORY('DIN 125','DIN 125',(#63086));
#63071=PRODUCT_RELATED_PRODUCT_CATEGORY('DIN 127','DIN 127',(#63087));
#63072=PRODUCT_RELATED_PRODUCT_CATEGORY('DIN 912 M6x12','DIN 912 M6x12',
(#63088));
#63073=APPLICATION_PROTOCOL_DEFINITION('international standard',
'automotive_design',2009,#63074);
#63074=APPLICATION_CONTEXT(
'Core Data for Automotive Mechanical Design Process');
#63075=PRODUCT_CONTEXT('part definition',#63074,'mechanical');
#63076=PRODUCT('EFI','MAS-617',
'STEP AP214',(#63075));
#63077=PRODUCT('Fuel Injector & Bracket','Fuel Injector & Bracket',$,(#63075));
#63078=PRODUCT('DIN 7985 M4x20','DIN 7985 M4x20',$,(#63075));
#63079=PRODUCT('Throttle Shaft & Butterfly Valve',
'Throttle Shaft & Butterfly Valve',$,(#63075));
#63080=PRODUCT('TPS - Throttle Position Sensor',
'TPS - Throttle Position Sensor',$,(#63075));
#63081=PRODUCT('Throttle Actuation Mechanism Spring',
'Throttle Actuation Mechanism Spring',$,(#63075));
#63082=PRODUCT('DIN 7985 M3x10','DIN 7985 M3x10',$,(#63075));
#63083=PRODUCT('MAP Sensor & Vacuum Tube','MAP Sensor & Vacuum Tube',$,
(#63075));
#63084=PRODUCT('Intake Manifold Flange','Intake Manifold Flange',$,(#63075));
#63085=PRODUCT('Throttle Body Housing','Throttle Body Housing',$,(#63075));
#63086=PRODUCT('DIN 125','DIN 125',$,(#63075));
#63087=PRODUCT('DIN 127','DIN 127',$,(#63075));
#63088=PRODUCT('DIN 912 M6x12','DIN 912 M6x12',$,(#63075));
#63089=PRESENTATION_STYLE_ASSIGNMENT((#63091));
#63090=PRESENTATION_STYLE_ASSIGNMENT((#63092));
#63091=SURFACE_STYLE_USAGE(.BOTH.,#63093);
#63092=SURFACE_STYLE_USAGE(.BOTH.,#63094);
#63093=SURFACE_SIDE_STYLE('',(#63095));
#63094=SURFACE_SIDE_STYLE('',(#63096));
#63095=SURFACE_STYLE_FILL_AREA(#63097);
#63096=SURFACE_STYLE_FILL_AREA(#63098);
#63097=FILL_AREA_STYLE('Steel - Satin',(#63099));
#63098=FILL_AREA_STYLE('Opaque(202,209,238)',(#63100));
#63099=FILL_AREA_STYLE_COLOUR('Steel - Satin',#63101);
#63100=FILL_AREA_STYLE_COLOUR('Opaque(202,209,238)',#63102);
#63101=COLOUR_RGB('Steel - Satin', 0.66274510, 0.83137255, 0.94901961);
#63102=COLOUR_RGB('Opaque(202,209,238)', 0.66274510, 0.83137255, 0.94901961);
ENDSEC;
END-ISO-10303-21;
